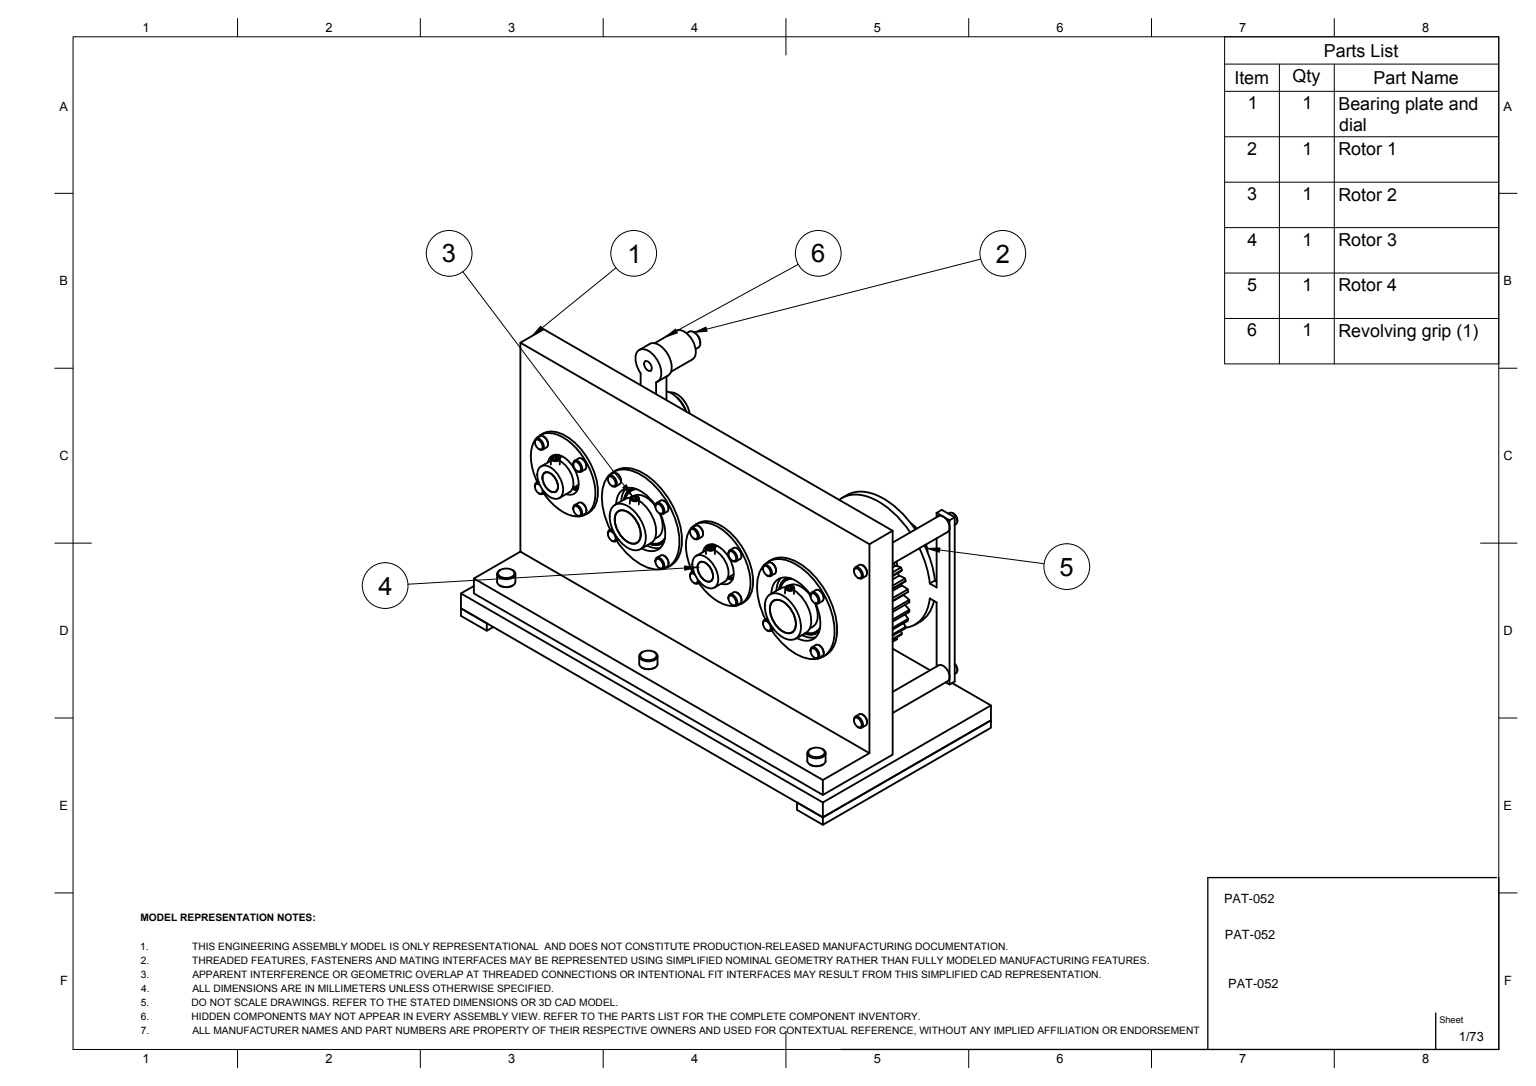
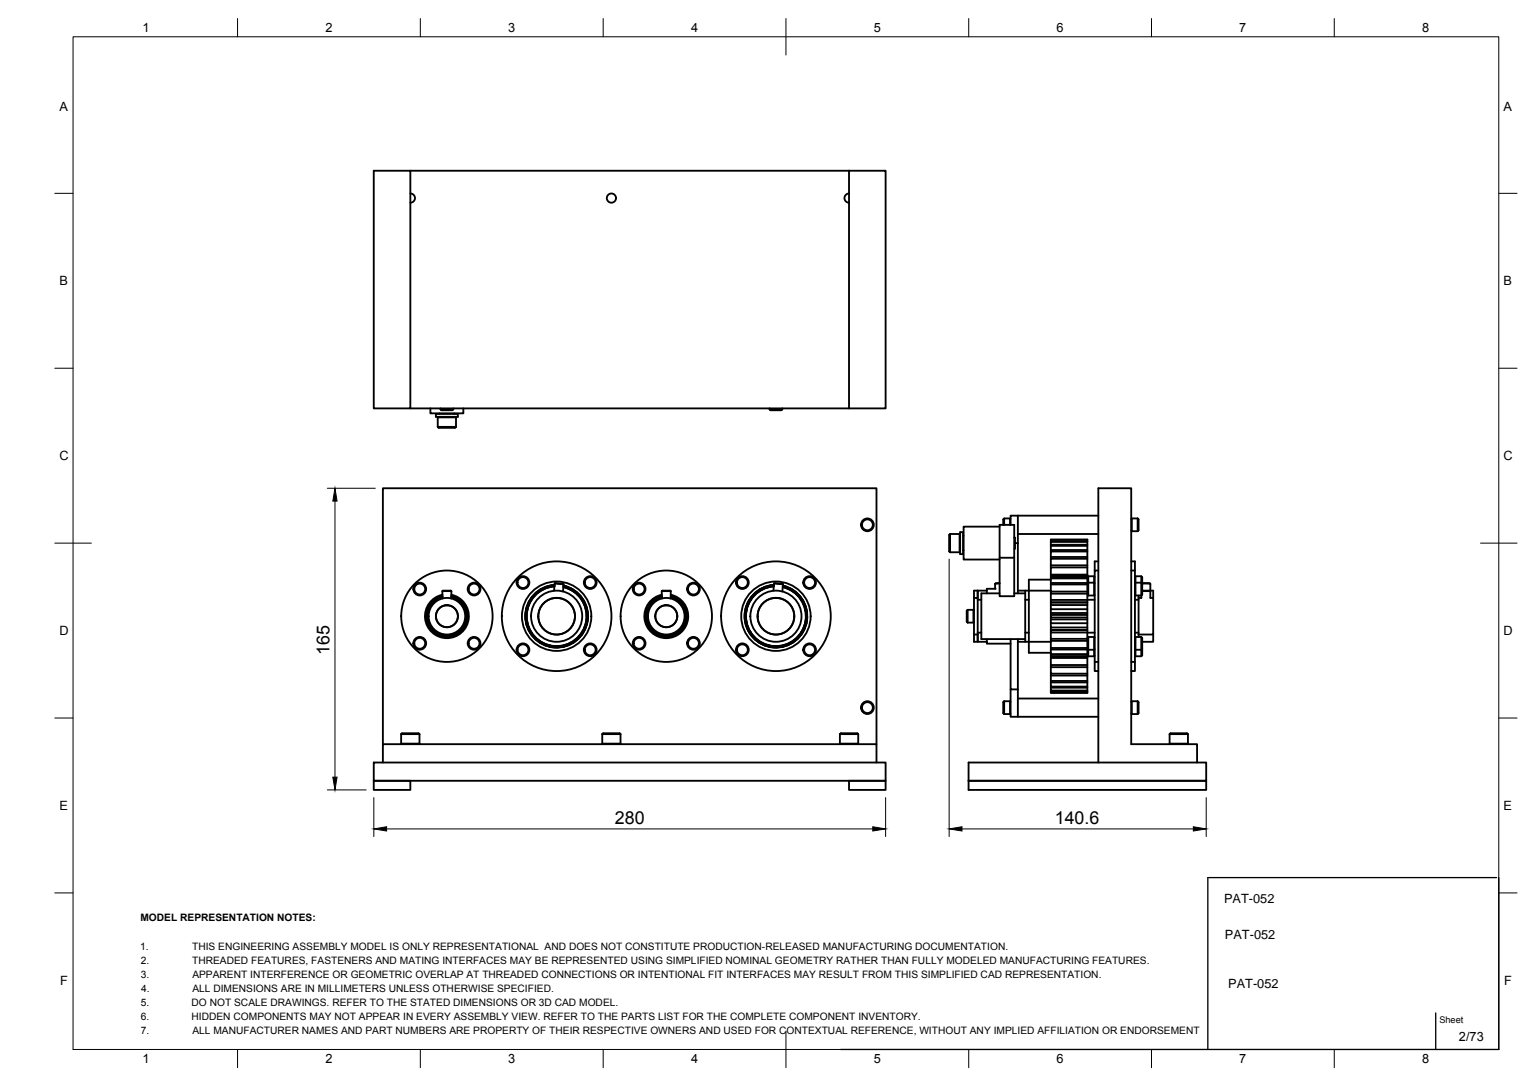
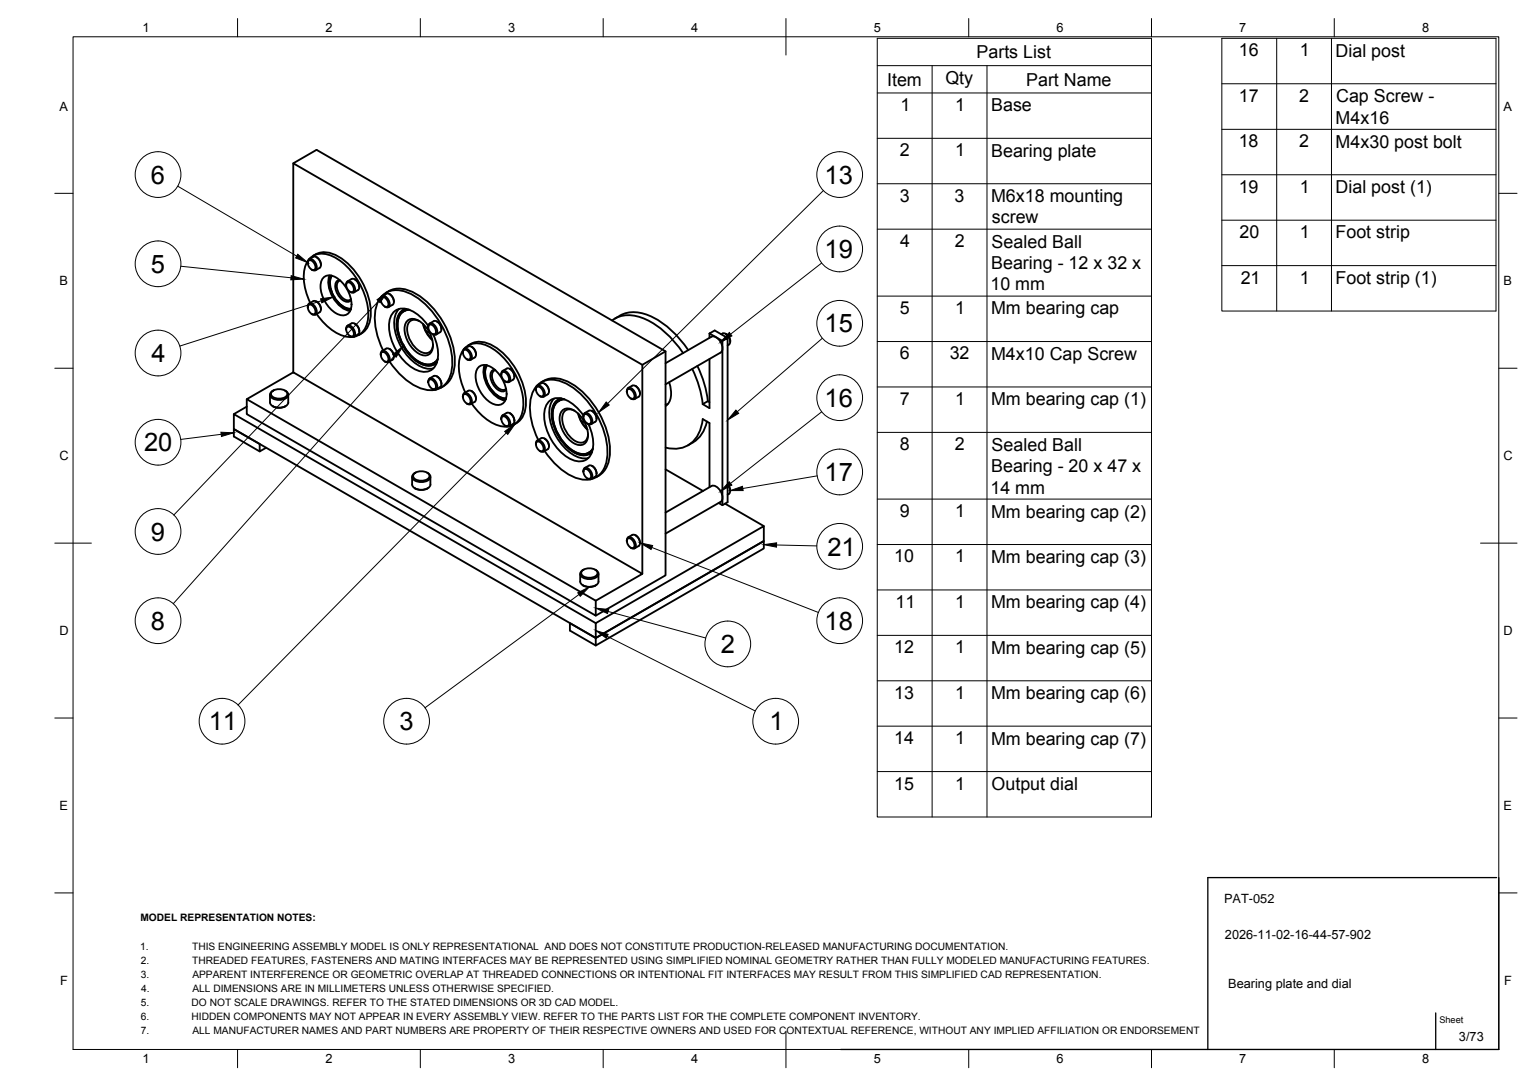
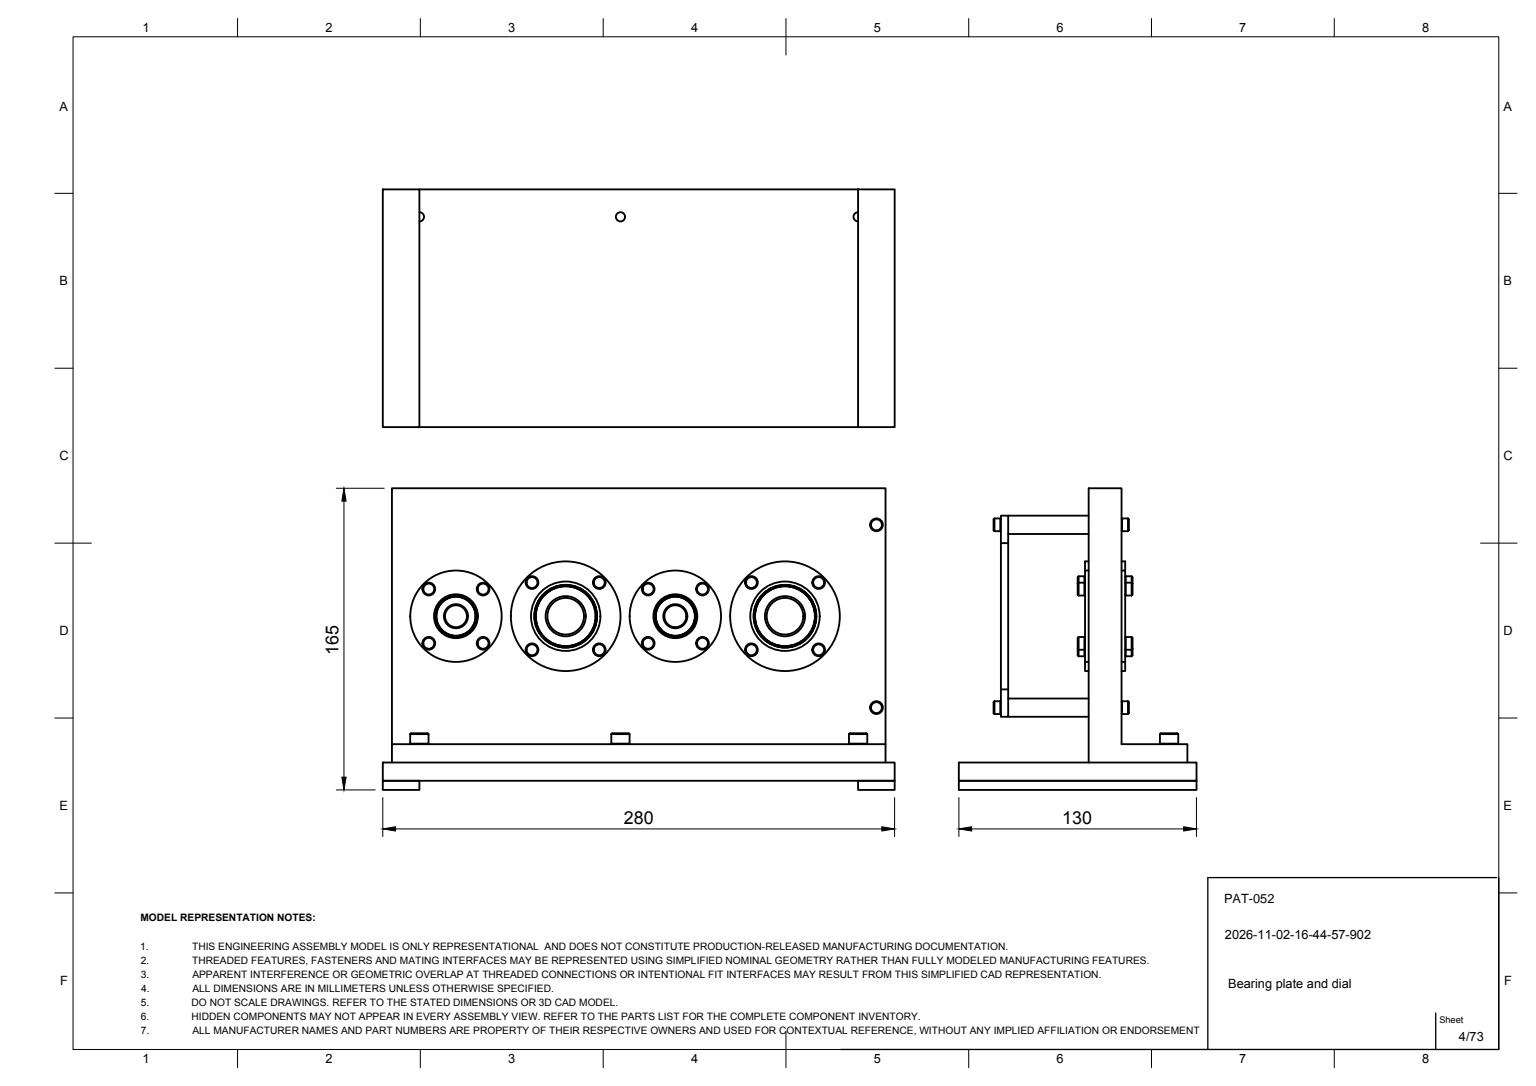
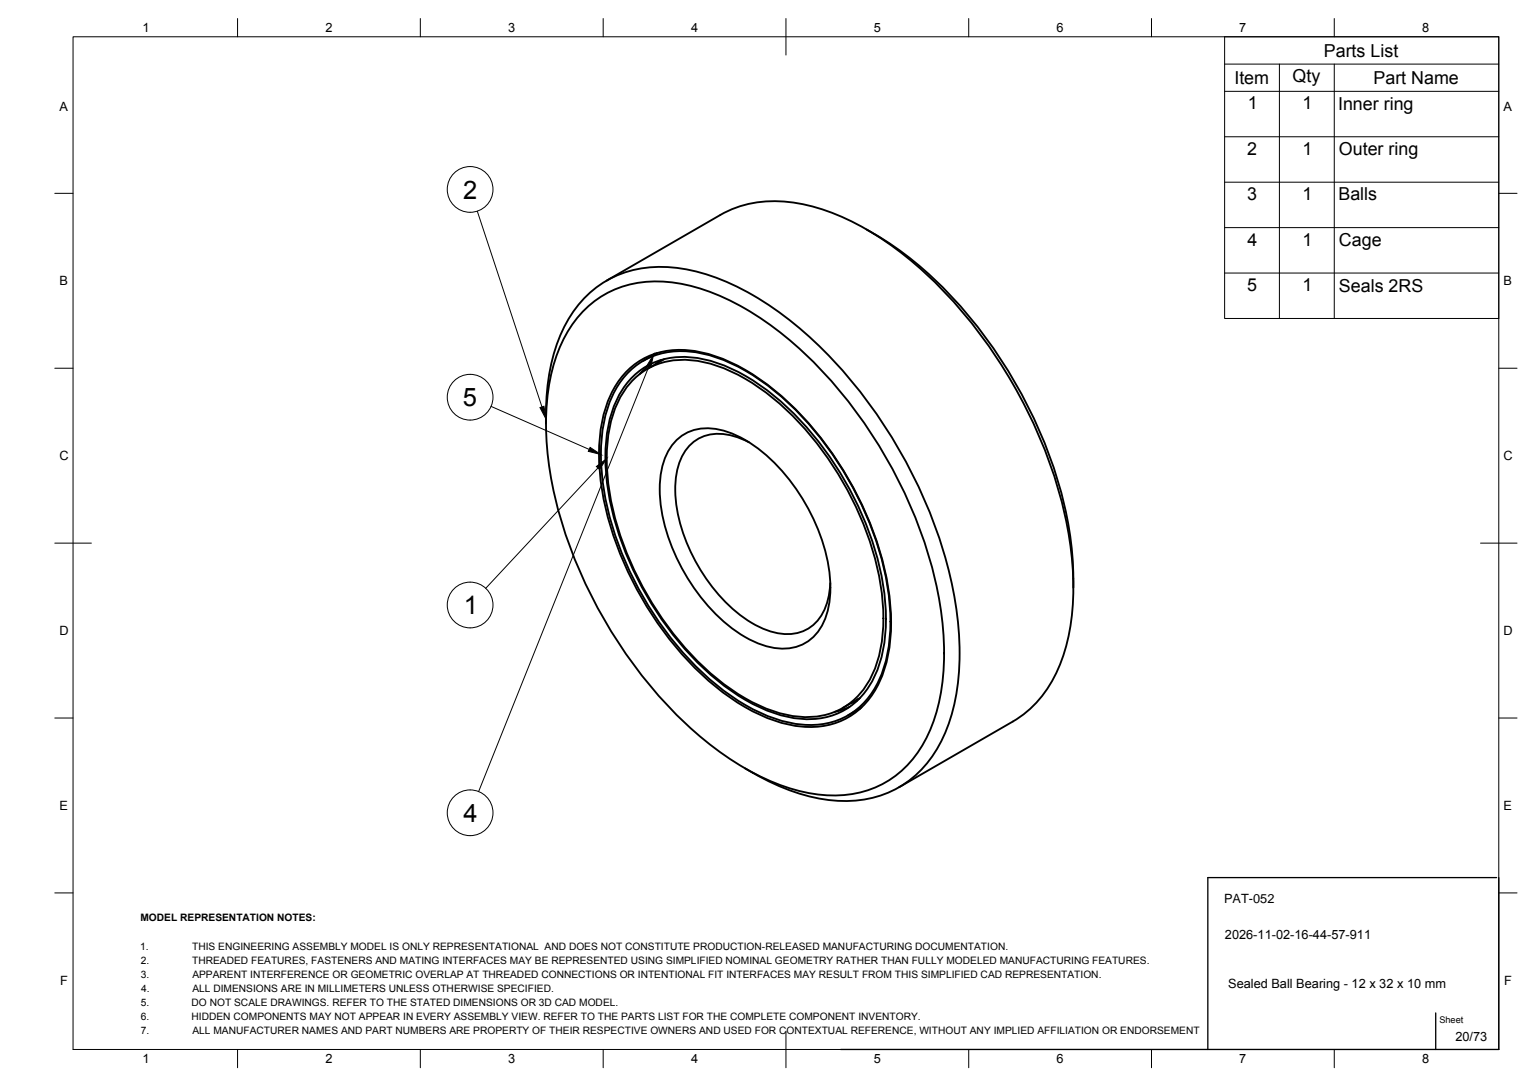
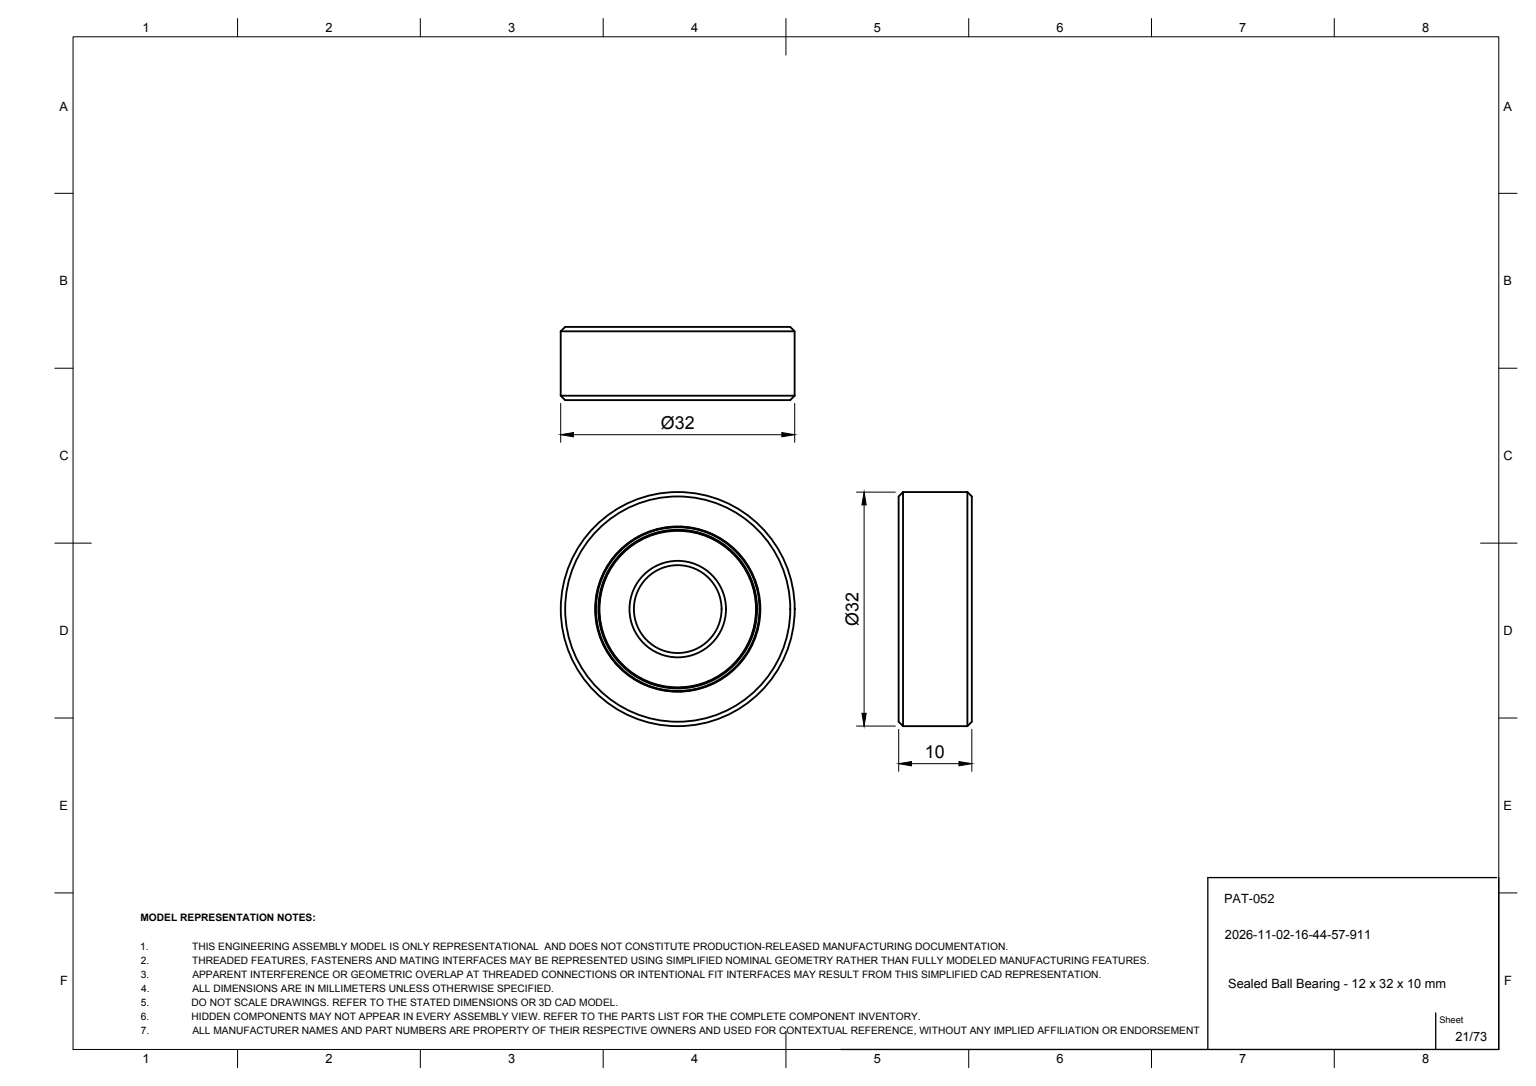
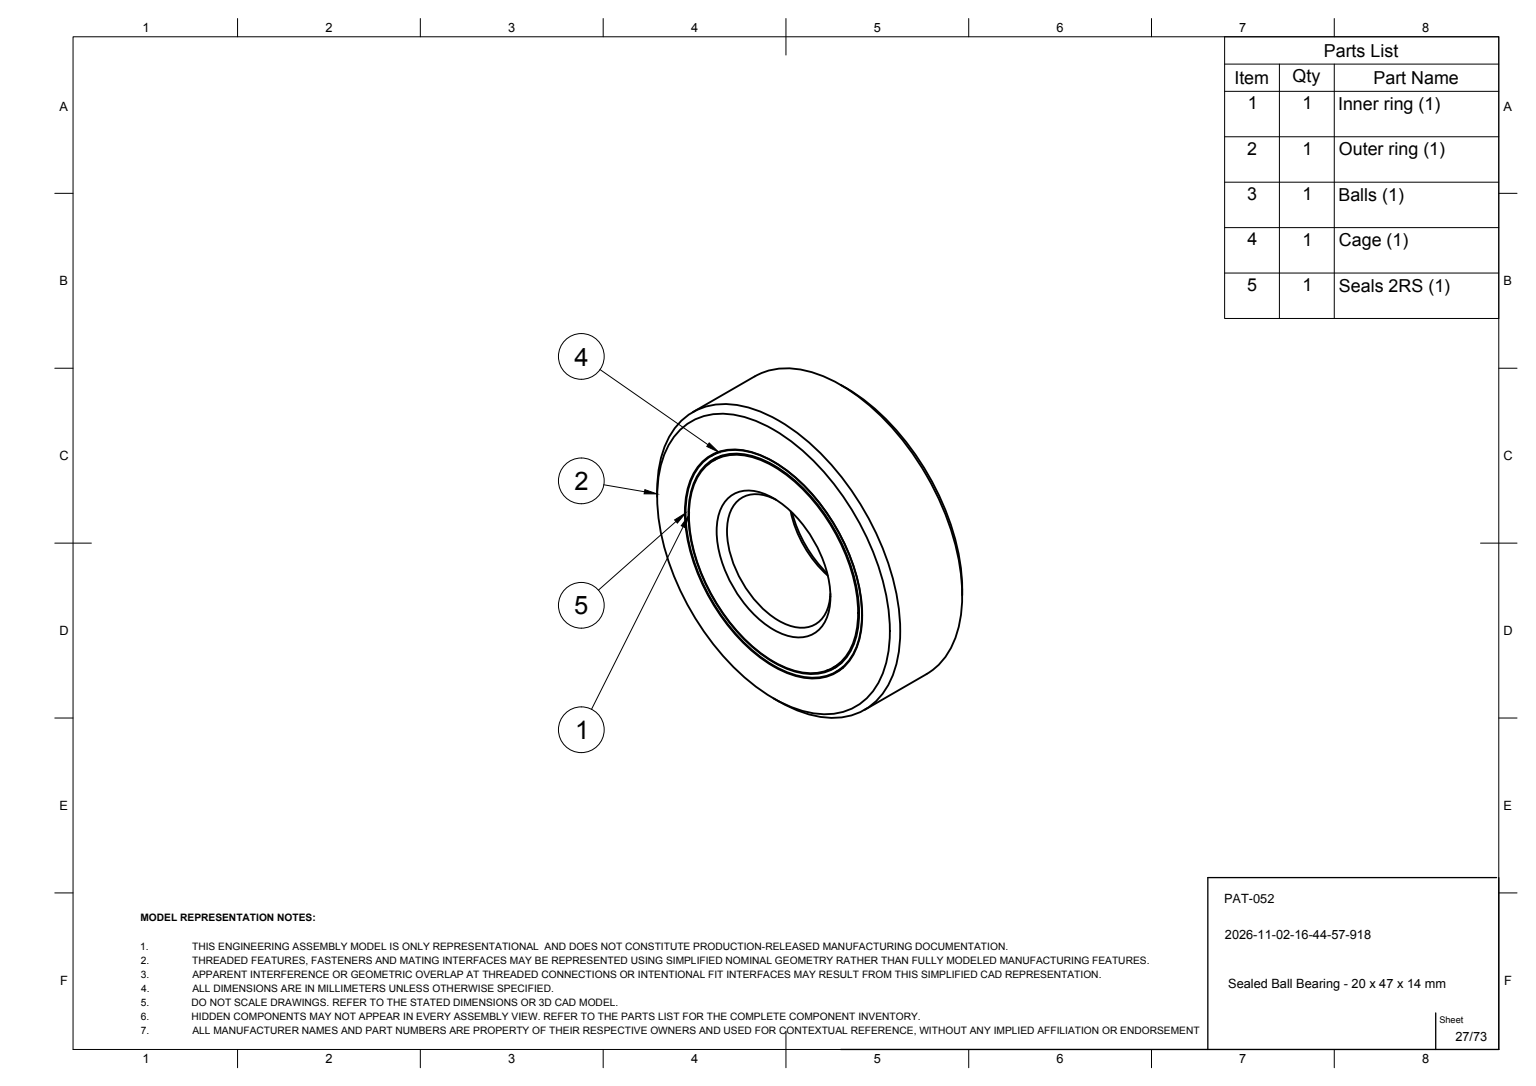
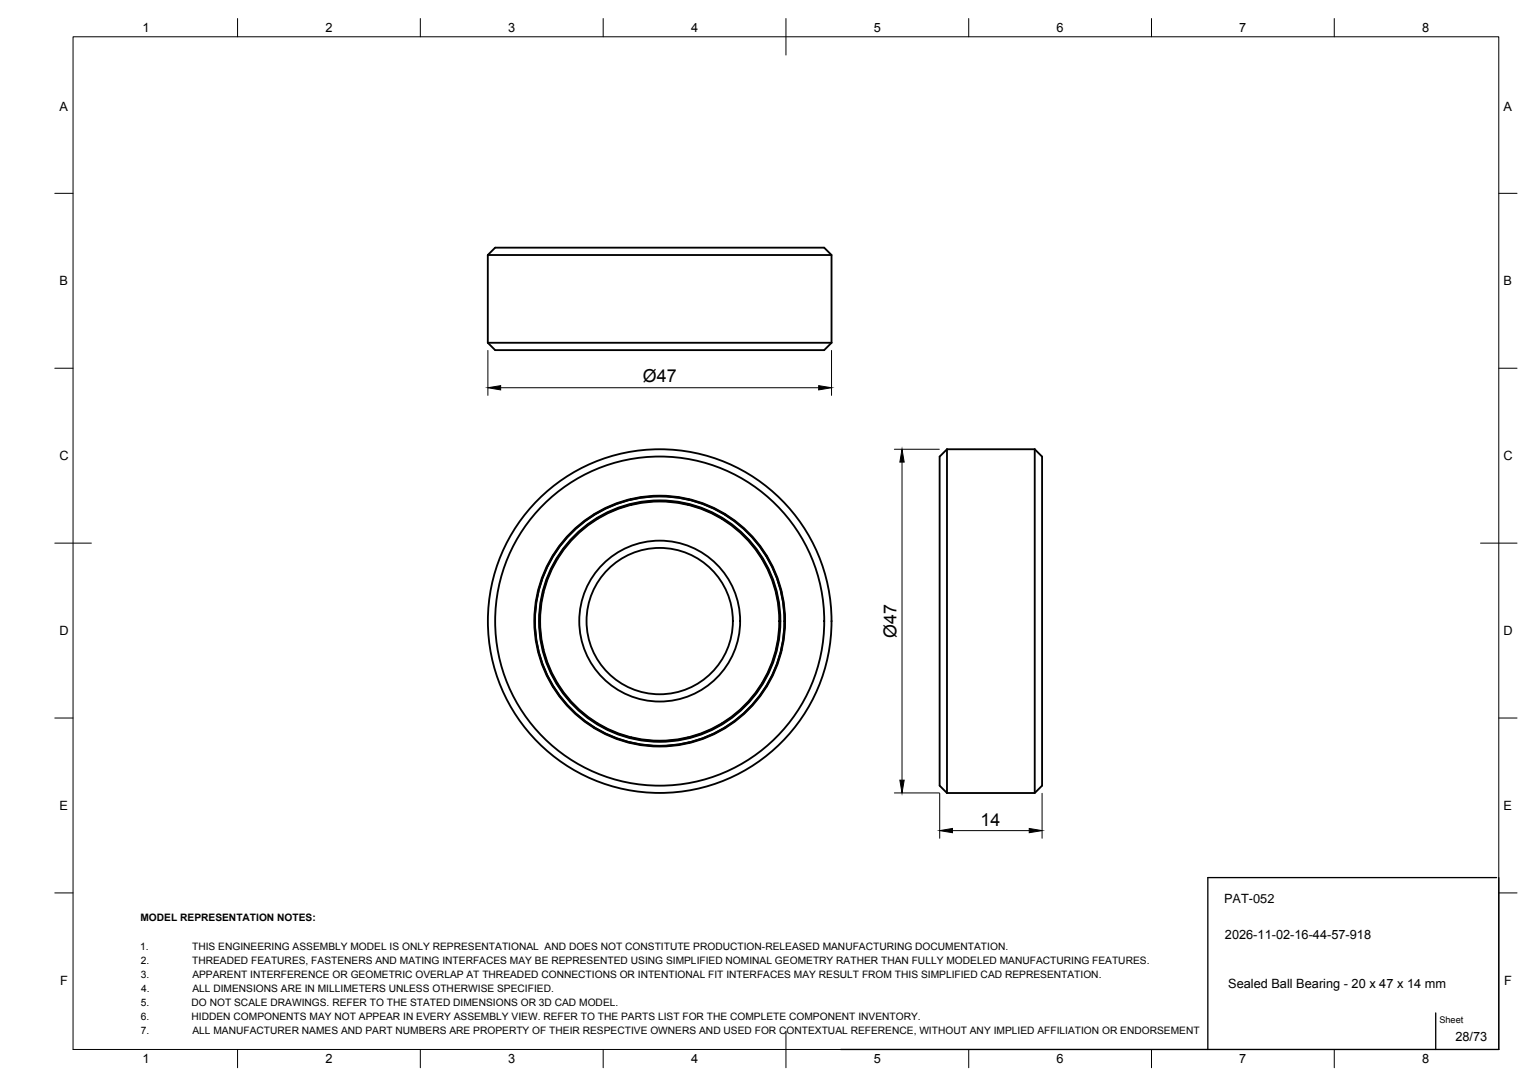
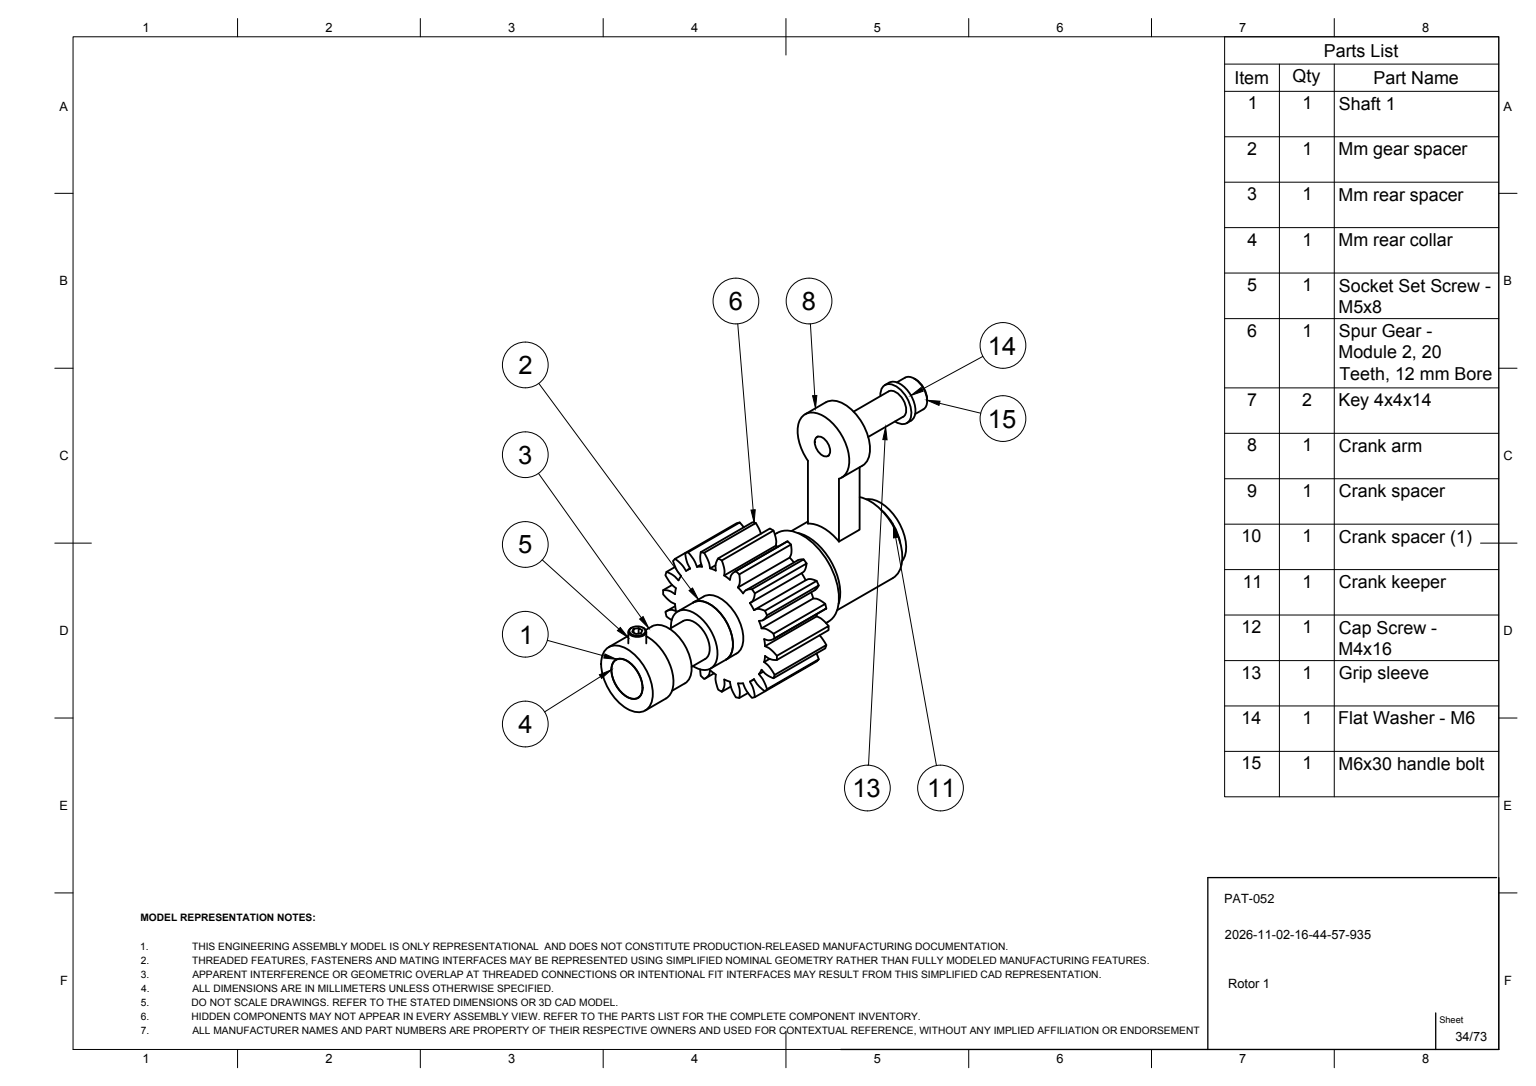
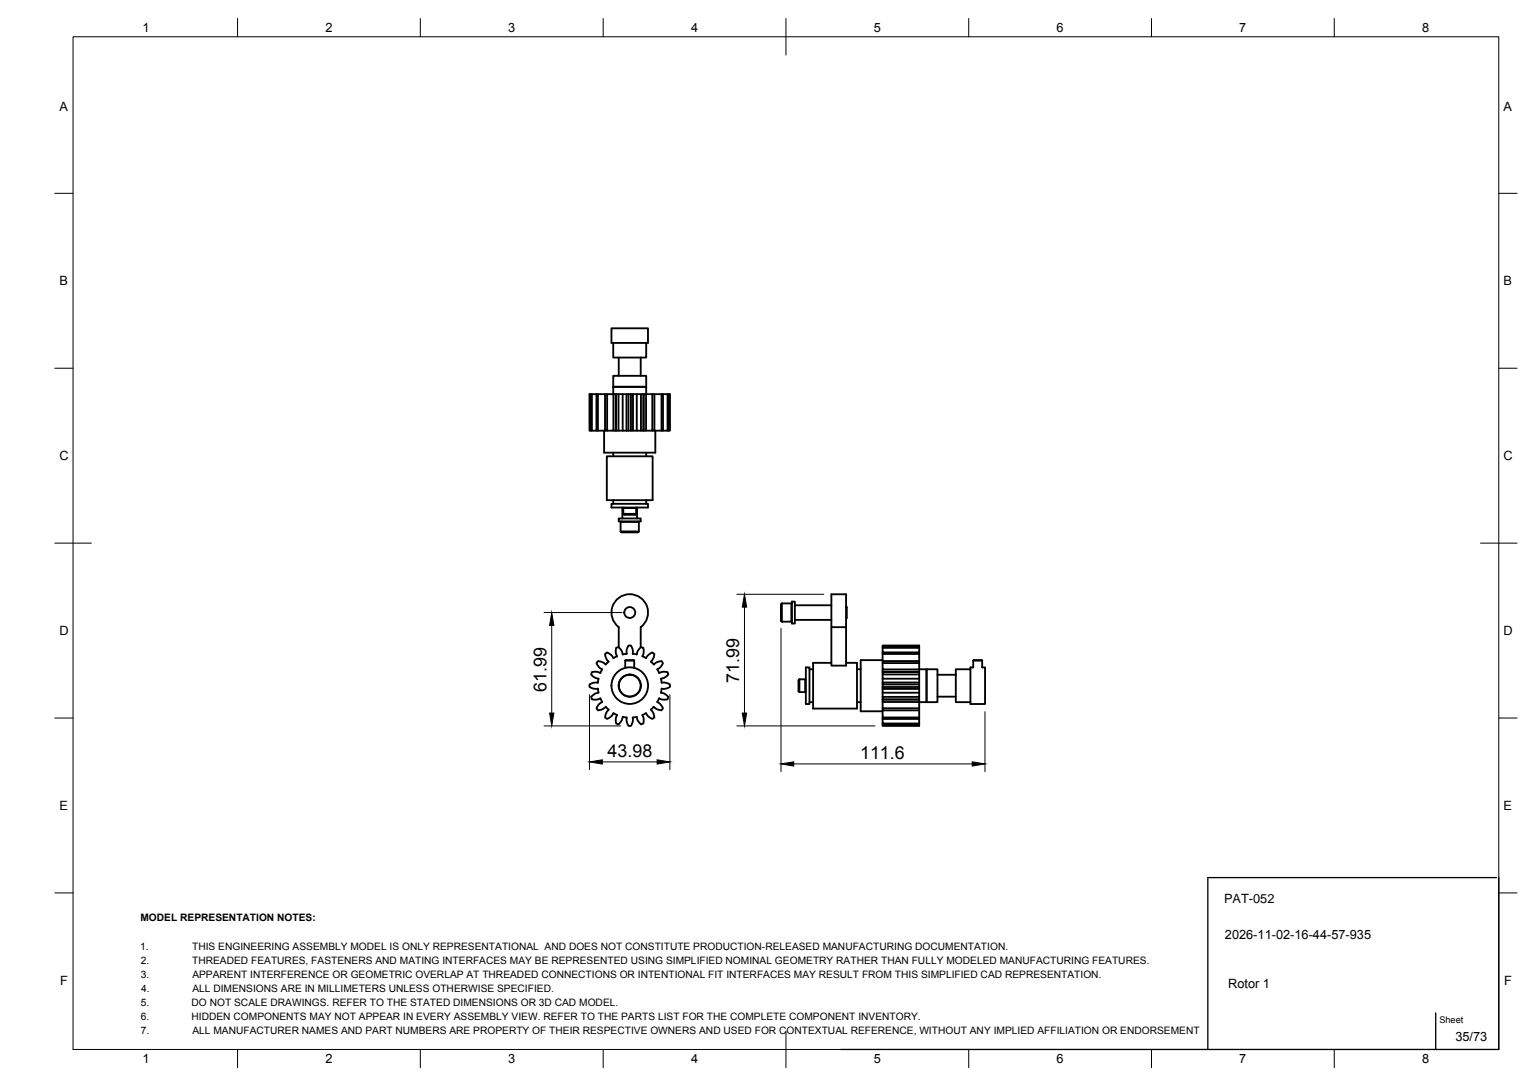
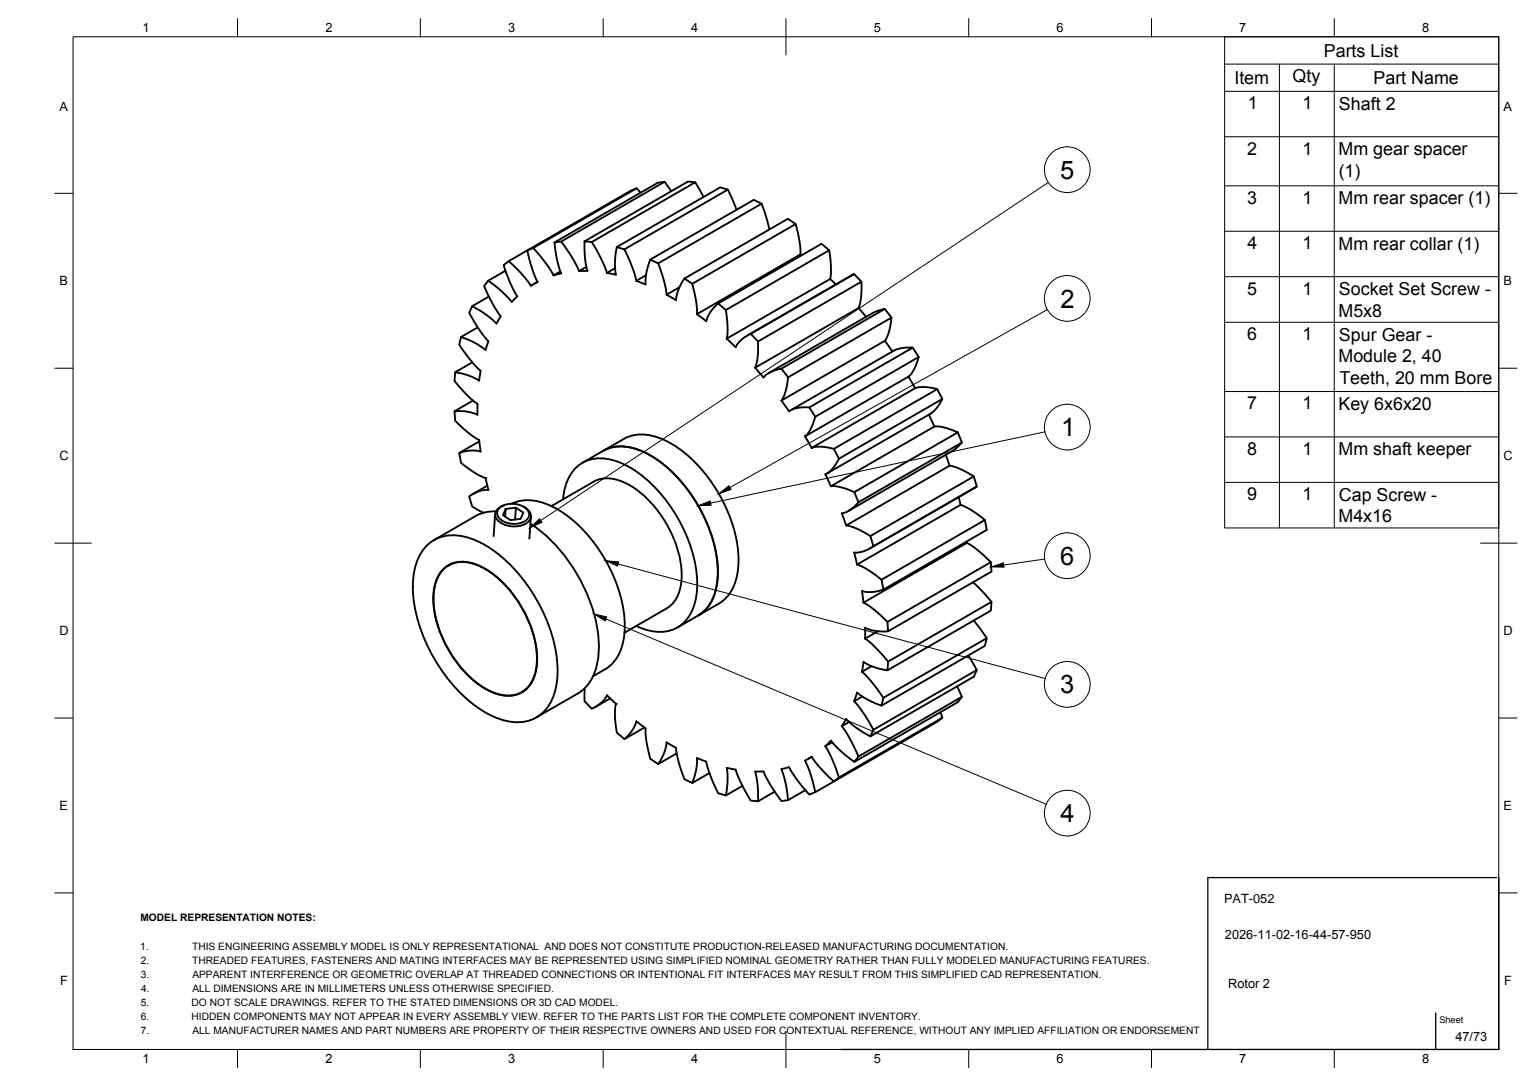
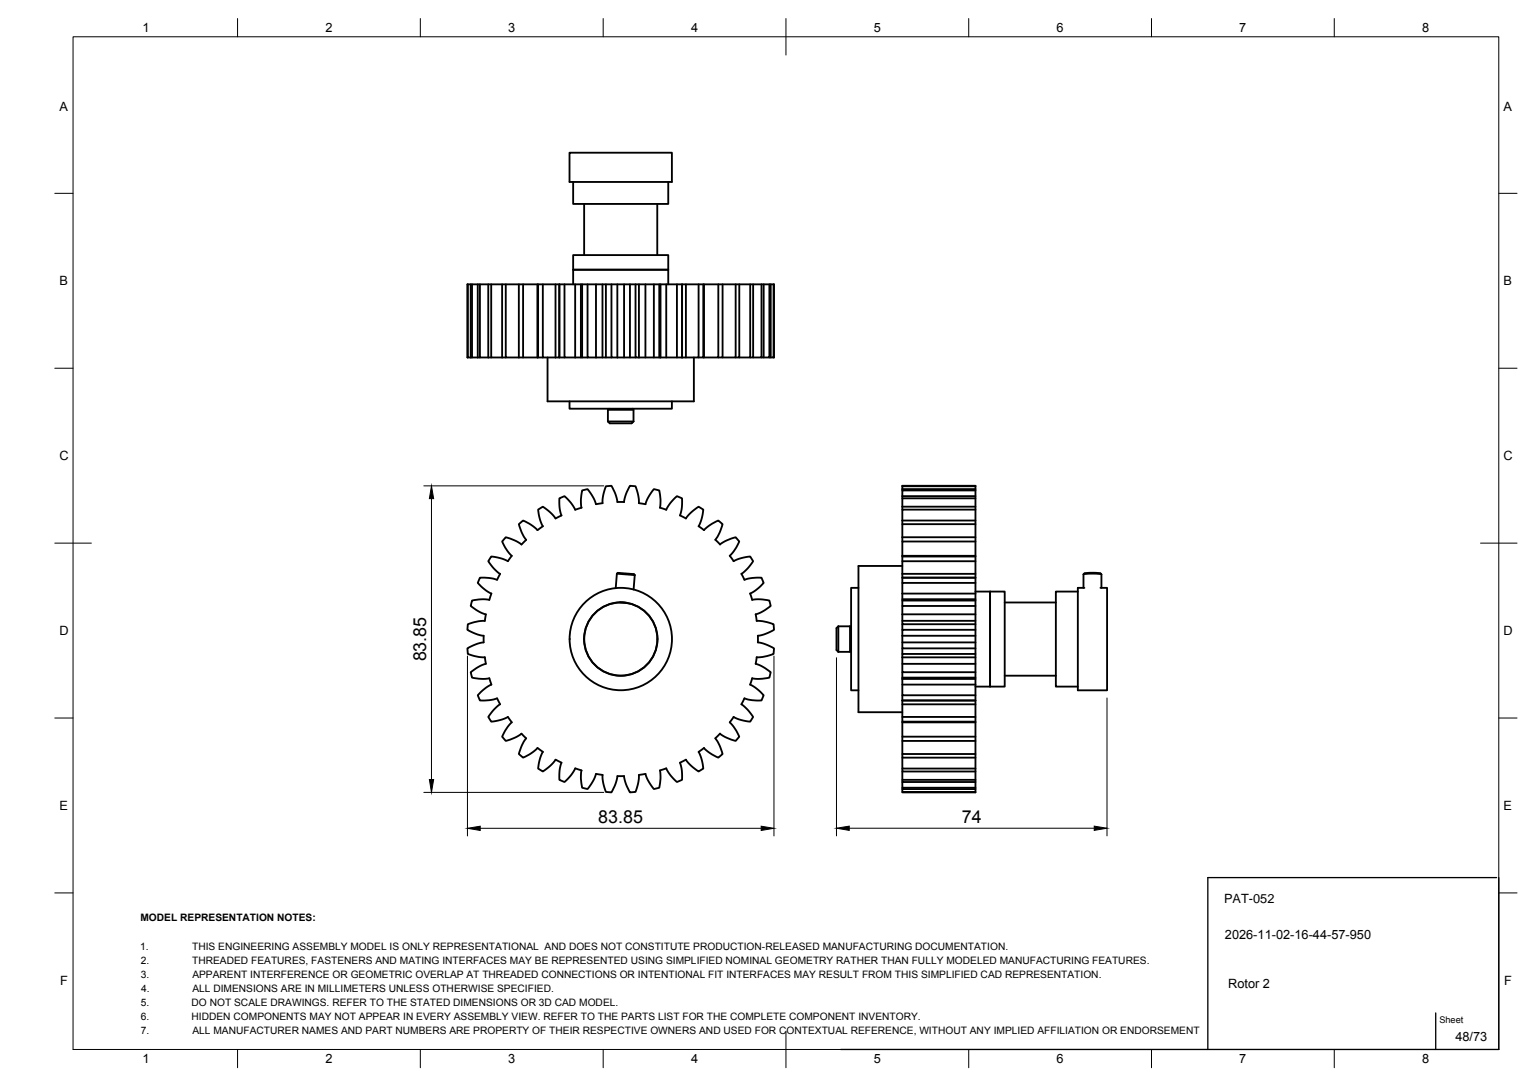
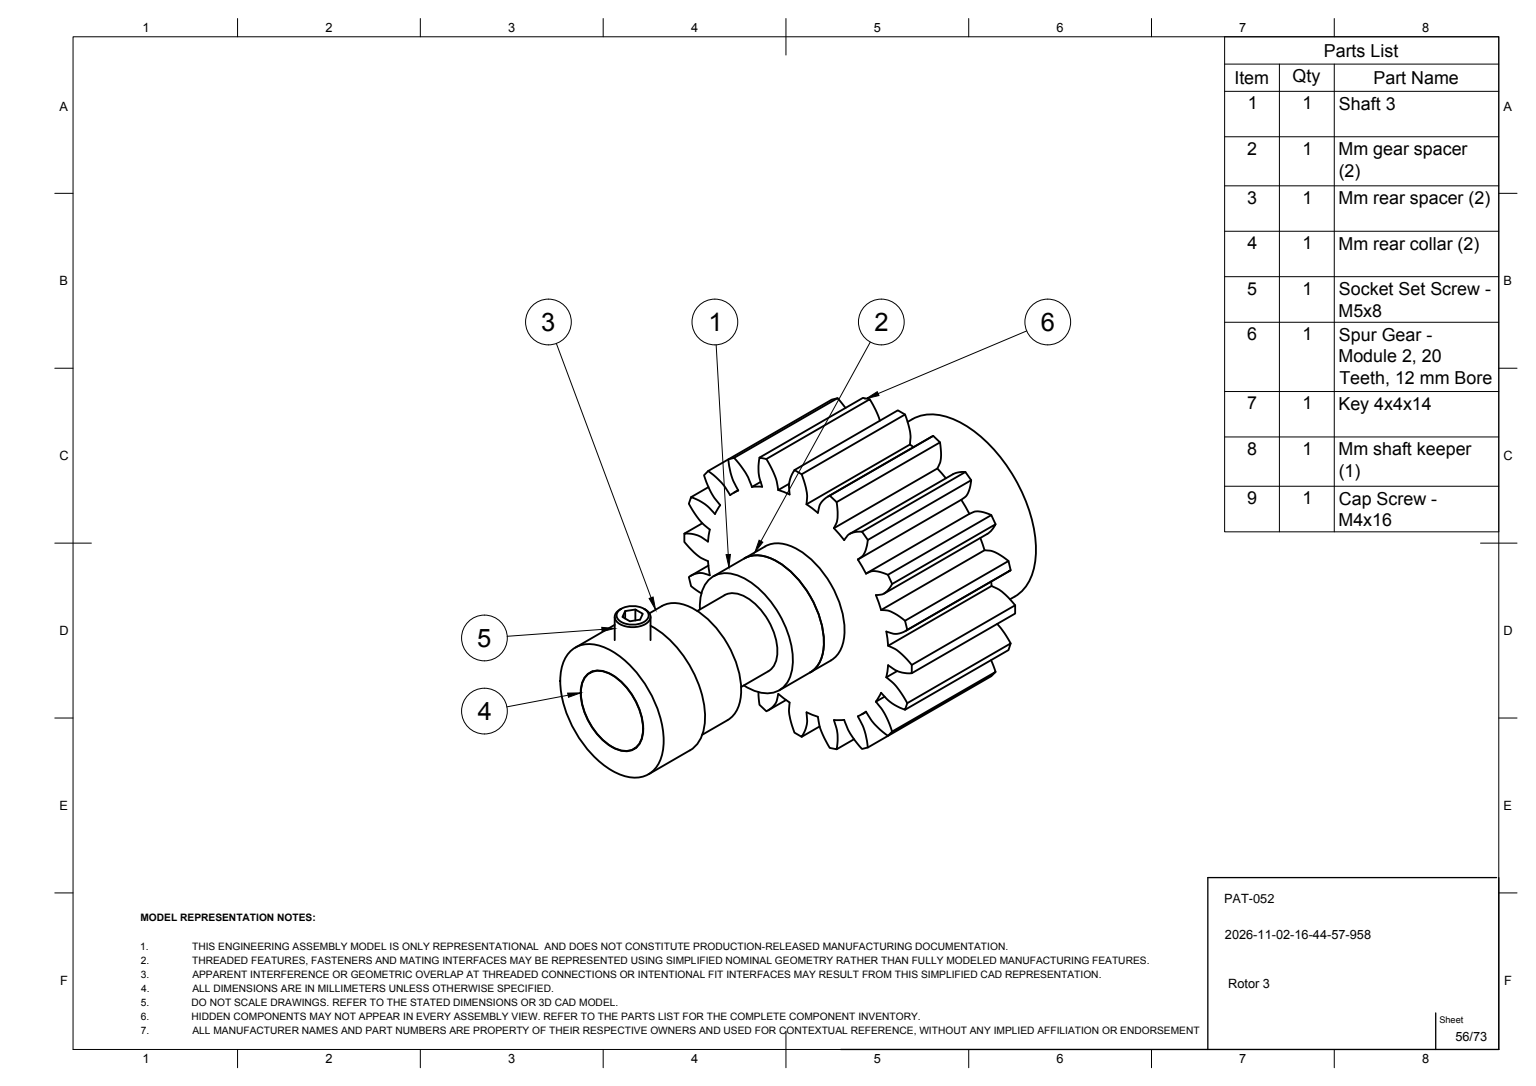
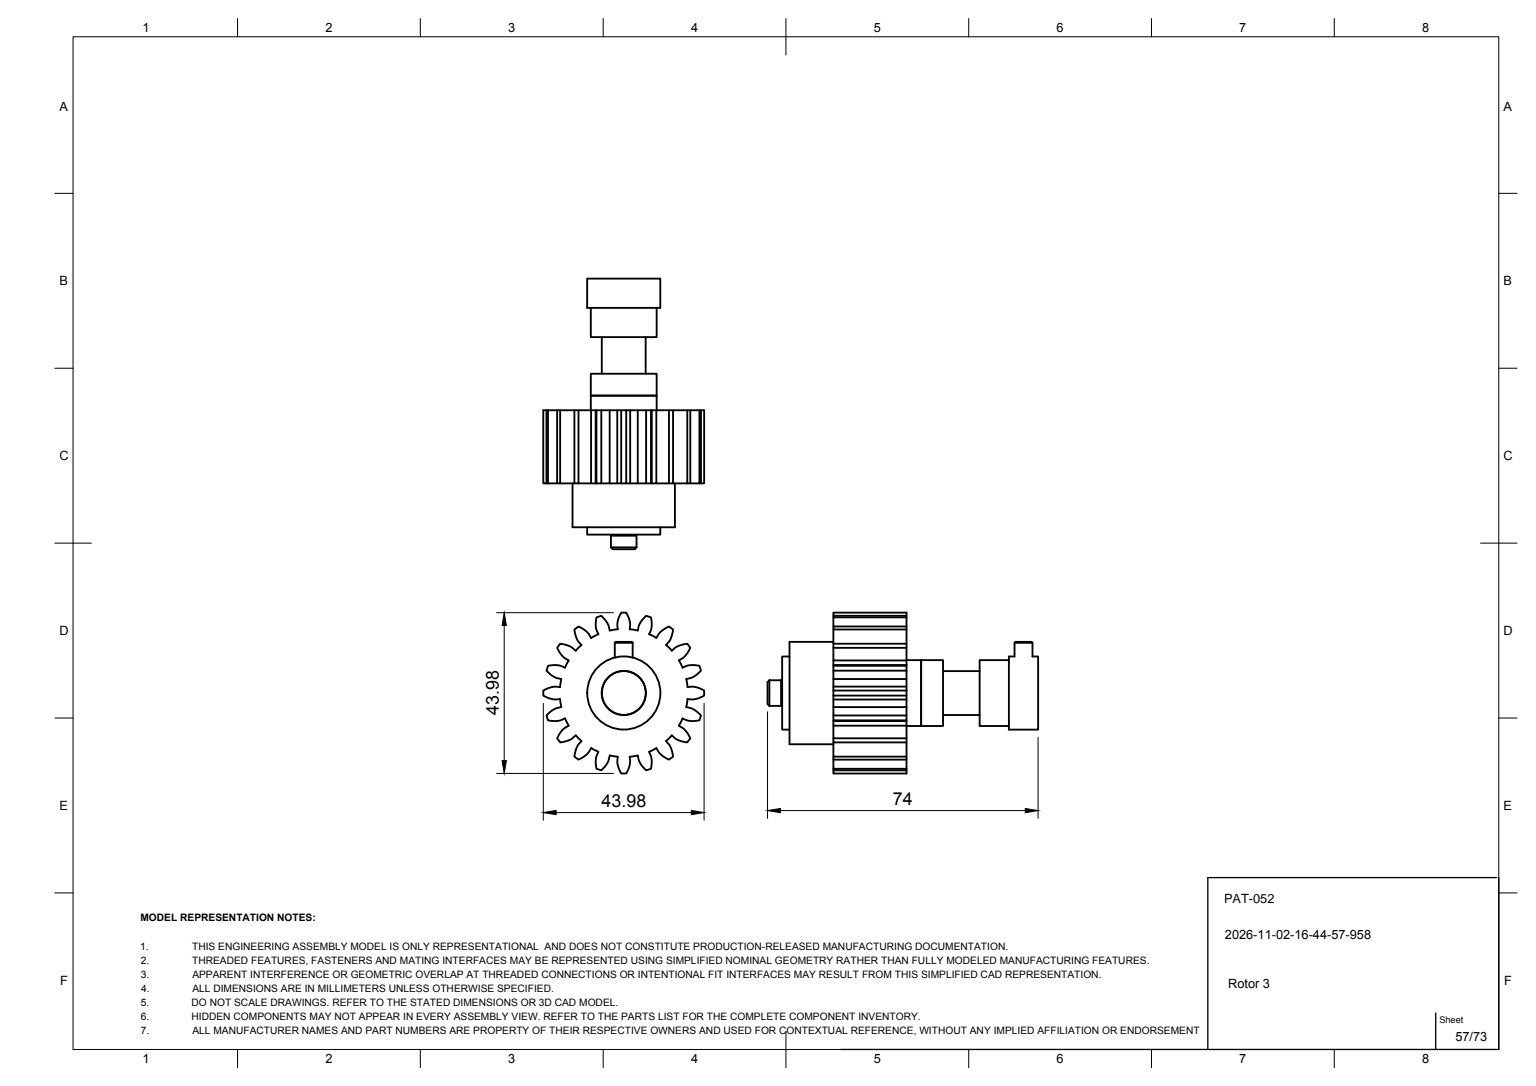
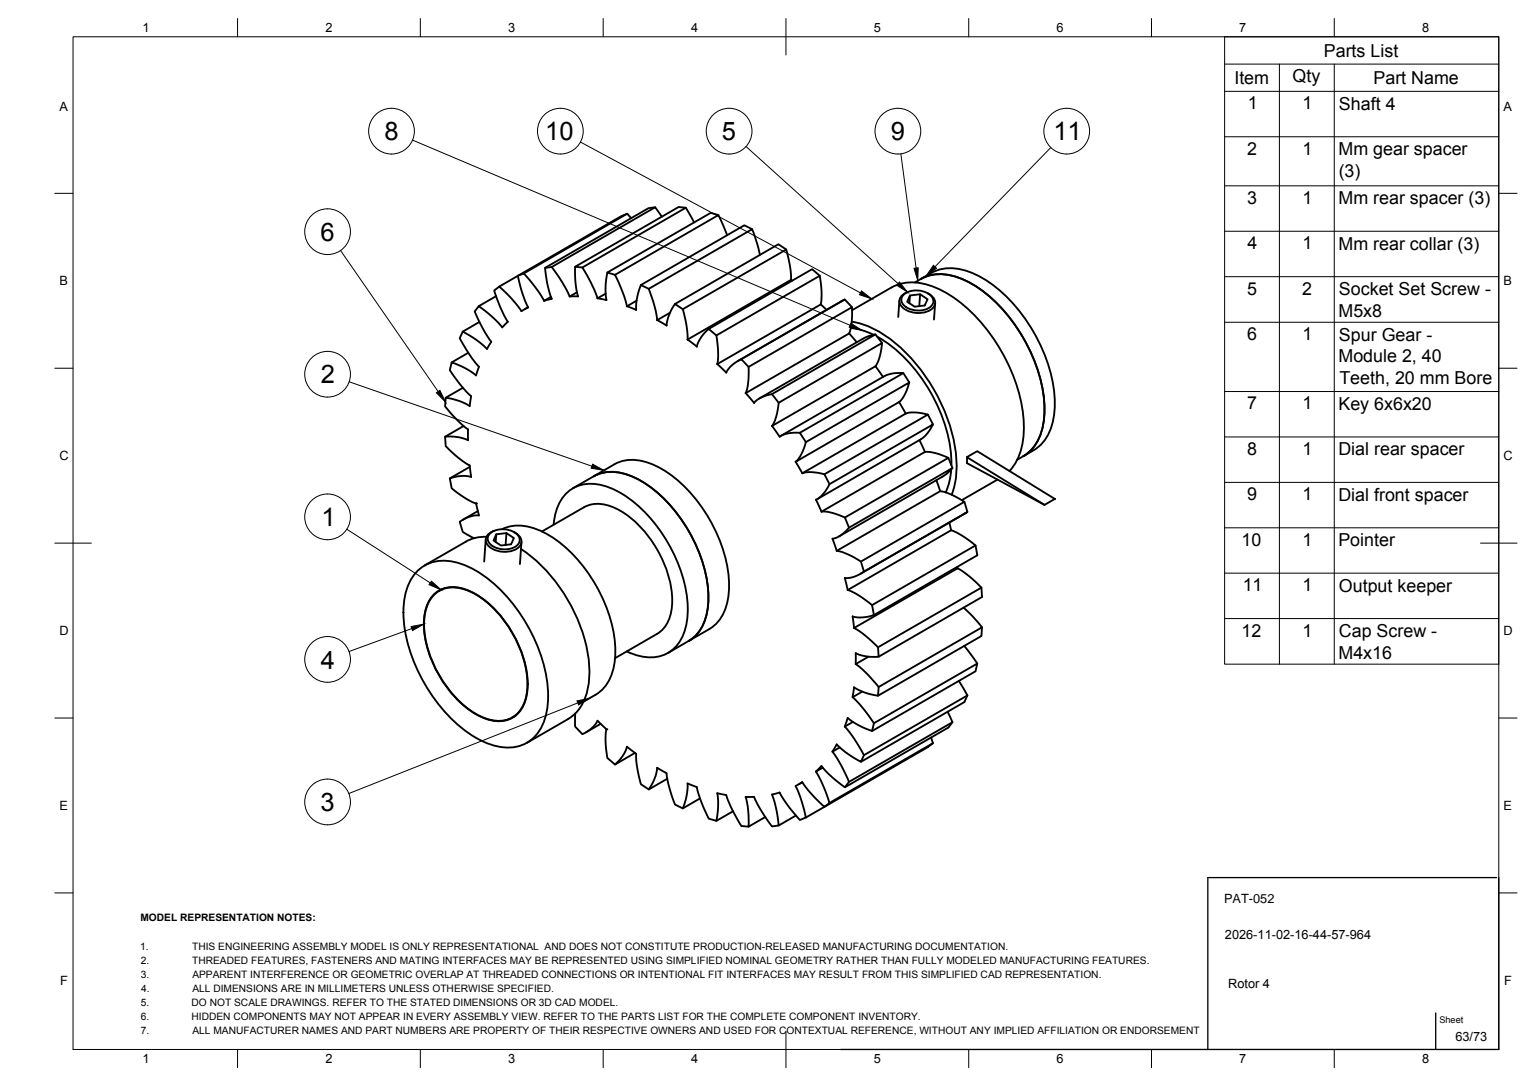
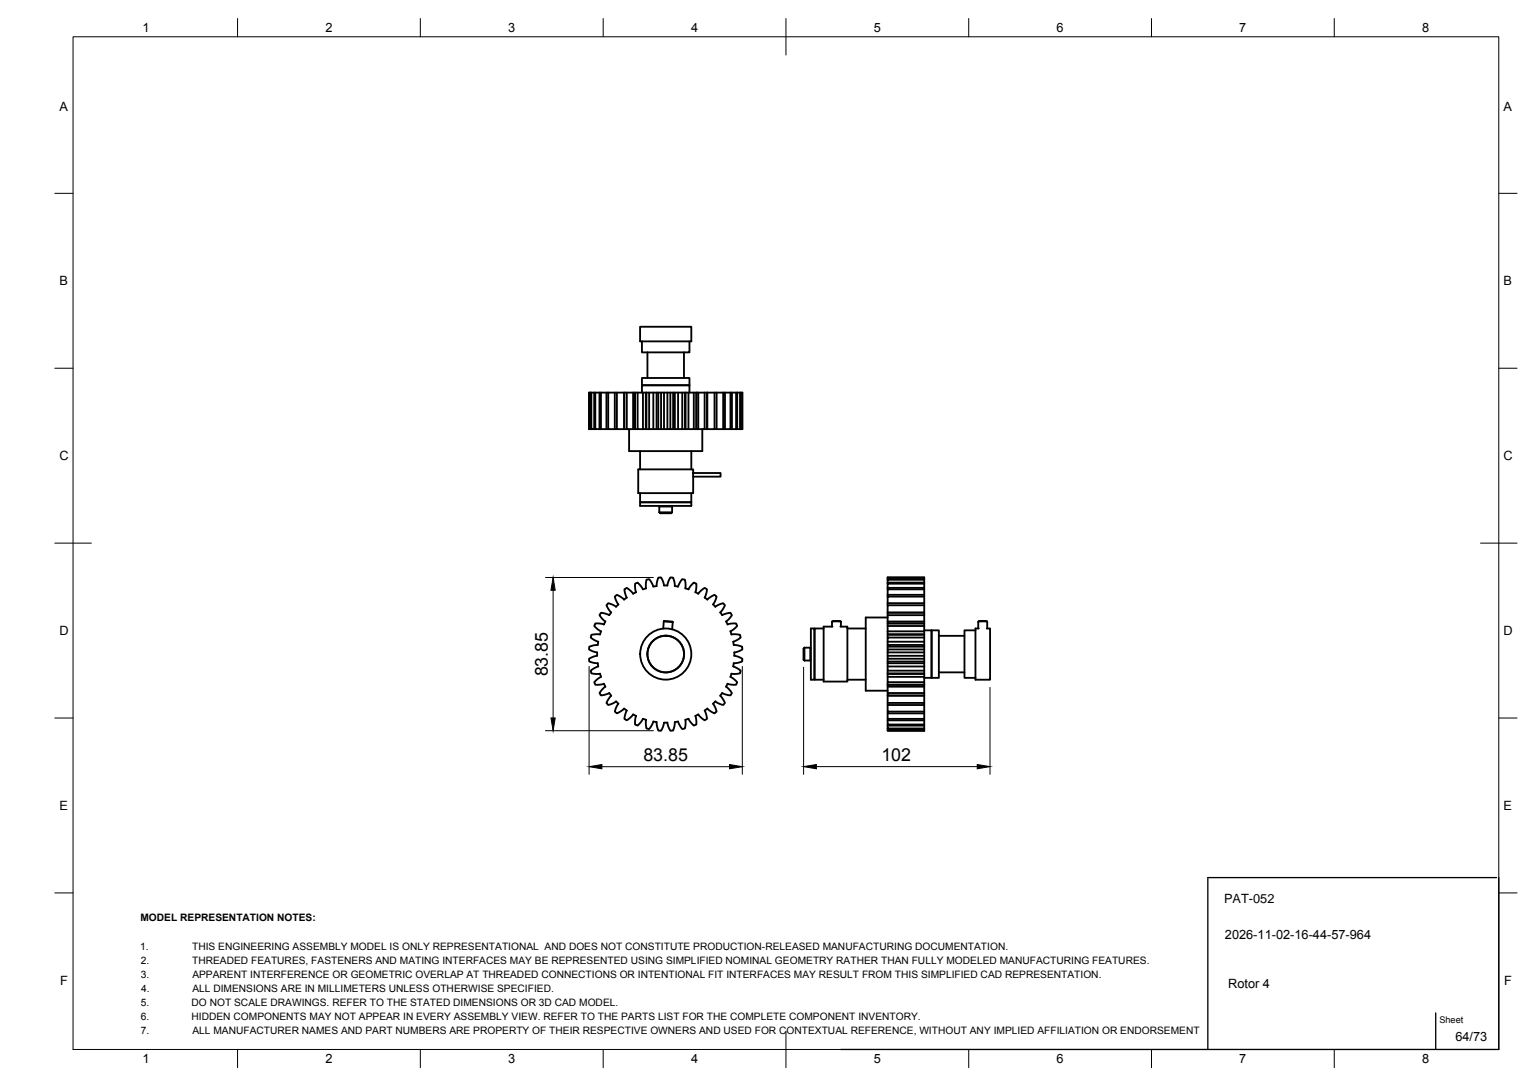
ISO-10303-21;
HEADER;
/* Generated by software containing ST-Developer
 * from STEP Tools, Inc. (www.steptools.com) 
 */

FILE_DESCRIPTION(
/* description */ ('Hand-crank gear train demonstrator'),
/* implementation_level */ '2;1');

FILE_NAME(
/* name */ 'PAT-052',
/* time_stamp */ '2026-10-28T03:22:13-07:00',
/* author */ (''),
/* organization */ (''),
/* preprocessor_version */ 'ST-DEVELOPER v20.2',
/* originating_system */ 'Autodesk Translation Framework v15.17.0.0',
/* authorisation */ '');

FILE_SCHEMA (('AUTOMOTIVE_DESIGN { 1 0 10303 214 3 1 1 }'));
ENDSEC;

DATA;
#10=MECHANICAL_DESIGN_GEOMETRIC_PRESENTATION_REPRESENTATION('',(#1189,#1190,
#1191,#1192,#1193,#1194,#1195,#1196,#1197,#1198,#1199,#1200,#1201,#1202,
#1203,#1204,#1205,#1206,#1207,#1208,#1209,#1210,#1211,#1212,#1213,#1214,
#1215,#1216,#1217,#1218,#1219,#1220,#1221,#1222,#1223,#1224,#1225,#1226,
#1227,#1228,#1229,#1230,#1231,#1232,#1233,#1234,#1235,#1236,#1237,#1238,
#1239,#1240,#1241,#1242,#1243,#1244,#1245,#1246,#1247,#1248,#1249,#1250,
#1251,#1252,#1253,#1254,#1255,#1256,#1257,#1258,#1259,#1260,#1261,#1262,
#1263,#1264,#1265,#1266,#1267),#62758);
#11=(
BOUNDED_SURFACE()
B_SPLINE_SURFACE(5,1,((#29730,#29731),(#29732,#29733),(#29734,#29735),(#29736,
#29737),(#29738,#29739),(#29740,#29741),(#29742,#29743),(#29744,#29745),
(#29746,#29747),(#29748,#29749),(#29750,#29751),(#29752,#29753),(#29754,
#29755),(#29756,#29757),(#29758,#29759),(#29760,#29761),(#29762,#29763),
(#29764,#29765),(#29766,#29767),(#29768,#29769),(#29770,#29771),(#29772,
#29773),(#29774,#29775),(#29776,#29777),(#29778,#29779),(#29780,#29781),
(#29782,#29783),(#29784,#29785),(#29786,#29787),(#29788,#29789),(#29790,
#29791),(#29792,#29793),(#29794,#29795),(#29796,#29797),(#29798,#29799),
(#29800,#29801),(#29802,#29803),(#29804,#29805),(#29806,#29807),(#29808,
#29809),(#29810,#29811),(#29812,#29813),(#29814,#29815),(#29816,#29817),
(#29818,#29819),(#29820,#29821),(#29822,#29823),(#29824,#29825),(#29826,
#29827),(#29828,#29829),(#29830,#29831),(#29832,#29833),(#29834,#29835),
(#29836,#29837),(#29838,#29839),(#29840,#29841),(#29842,#29843),(#29844,
#29845),(#29846,#29847),(#29848,#29849),(#29850,#29851),(#29852,#29853),
(#29854,#29855),(#29856,#29857),(#29858,#29859),(#29860,#29861),(#29862,
#29863),(#29864,#29865),(#29866,#29867),(#29868,#29869)),.UNSPECIFIED.,
 .F.,.F.,.F.)
B_SPLINE_SURFACE_WITH_KNOTS((6,1,1,1,1,1,1,1,1,1,1,1,1,1,1,1,1,1,1,1,1,
1,1,1,1,1,1,1,1,1,1,1,1,1,1,1,1,1,1,1,1,1,1,1,1,1,1,1,1,1,1,1,1,1,1,1,1,
1,1,1,1,1,1,1,1,6),(2,2),(-1.,-0.984615384615383,-0.969230769230768,-0.953846153846152,
-0.938461538461537,-0.923076923076922,-0.907692307692306,-0.892307692307691,
-0.876923076923076,-0.86153846153846,-0.846153846153845,-0.83076923076923,
-0.815384615384614,-0.799999999999999,-0.784615384615384,-0.769230769230768,
-0.753846153846153,-0.738461538461538,-0.723076923076922,-0.707692307692307,
-0.692307692307692,-0.676923076923076,-0.661538461538461,-0.646153846153846,
-0.63076923076923,-0.615384615384615,-0.6,-0.584615384615384,-0.569230769230769,
-0.553846153846154,-0.538461538461538,-0.523076923076923,-0.507692307692308,
-0.492307692307692,-0.476923076923077,-0.461538461538462,-0.446153846153846,
-0.430769230769231,-0.415384615384615,-0.4,-0.384615384615385,-0.369230769230769,
-0.353846153846154,-0.338461538461538,-0.323076923076923,-0.307692307692308,
-0.292307692307692,-0.276923076923077,-0.261538461538462,-0.246153846153846,
-0.230769230769231,-0.215384615384615,-0.2,-0.184615384615385,-0.169230769230769,
-0.153846153846154,-0.138461538461538,-0.123076923076923,-0.107692307692308,
-0.0923076923076923,-0.0769230769230769,-0.0615384615384615,-0.0461538461538462,
-0.0307692307692308,-0.0153846153846154,0.),(-1.,1.),.UNSPECIFIED.)
GEOMETRIC_REPRESENTATION_ITEM()
RATIONAL_B_SPLINE_SURFACE(((1.,1.),(1.,1.),(1.,1.),(1.,1.),(1.,1.),(1.,
1.),(1.,1.),(1.,1.),(1.,1.),(1.,1.),(1.,1.),(1.,1.),(1.,1.),(1.,1.),(1.,
1.),(1.,1.),(1.,1.),(1.,1.),(1.,1.),(1.,1.),(1.,1.),(1.,1.),(1.,1.),(1.,
1.),(1.,1.),(1.,1.),(1.,1.),(1.,1.),(1.,1.),(1.,1.),(1.,1.),(1.,1.),(1.,
1.),(1.,1.),(1.,1.),(1.,1.),(1.,1.),(1.,1.),(1.,1.),(1.,1.),(1.,1.),(1.,
1.),(1.,1.),(1.,1.),(1.,1.),(1.,1.),(1.,1.),(1.,1.),(1.,1.),(1.,1.),(1.,
1.),(1.,1.),(1.,1.),(1.,1.),(1.,1.),(1.,1.),(1.,1.),(1.,1.),(1.,1.),(1.,
1.),(1.,1.),(1.,1.),(1.,1.),(1.,1.),(1.,1.),(1.,1.),(1.,1.),(1.,1.),(1.,
1.),(1.,1.)))
REPRESENTATION_ITEM('')
SURFACE()
);
#12=(
BOUNDED_SURFACE()
B_SPLINE_SURFACE(5,1,((#29948,#29949),(#29950,#29951),(#29952,#29953),(#29954,
#29955),(#29956,#29957),(#29958,#29959),(#29960,#29961),(#29962,#29963),
(#29964,#29965),(#29966,#29967),(#29968,#29969),(#29970,#29971),(#29972,
#29973),(#29974,#29975),(#29976,#29977),(#29978,#29979),(#29980,#29981),
(#29982,#29983),(#29984,#29985),(#29986,#29987),(#29988,#29989),(#29990,
#29991),(#29992,#29993),(#29994,#29995),(#29996,#29997),(#29998,#29999),
(#30000,#30001),(#30002,#30003),(#30004,#30005),(#30006,#30007),(#30008,
#30009),(#30010,#30011),(#30012,#30013),(#30014,#30015),(#30016,#30017),
(#30018,#30019),(#30020,#30021),(#30022,#30023),(#30024,#30025),(#30026,
#30027),(#30028,#30029),(#30030,#30031),(#30032,#30033),(#30034,#30035),
(#30036,#30037),(#30038,#30039),(#30040,#30041),(#30042,#30043),(#30044,
#30045),(#30046,#30047),(#30048,#30049),(#30050,#30051),(#30052,#30053),
(#30054,#30055),(#30056,#30057),(#30058,#30059),(#30060,#30061),(#30062,
#30063),(#30064,#30065),(#30066,#30067),(#30068,#30069),(#30070,#30071),
(#30072,#30073),(#30074,#30075),(#30076,#30077),(#30078,#30079),(#30080,
#30081),(#30082,#30083),(#30084,#30085),(#30086,#30087)),.UNSPECIFIED.,
 .F.,.F.,.F.)
B_SPLINE_SURFACE_WITH_KNOTS((6,1,1,1,1,1,1,1,1,1,1,1,1,1,1,1,1,1,1,1,1,
1,1,1,1,1,1,1,1,1,1,1,1,1,1,1,1,1,1,1,1,1,1,1,1,1,1,1,1,1,1,1,1,1,1,1,1,
1,1,1,1,1,1,1,1,6),(2,2),(-1.,-0.984615384615383,-0.969230769230768,-0.953846153846152,
-0.938461538461537,-0.923076923076922,-0.907692307692306,-0.892307692307691,
-0.876923076923076,-0.86153846153846,-0.846153846153845,-0.83076923076923,
-0.815384615384614,-0.799999999999999,-0.784615384615384,-0.769230769230768,
-0.753846153846153,-0.738461538461538,-0.723076923076922,-0.707692307692307,
-0.692307692307692,-0.676923076923076,-0.661538461538461,-0.646153846153846,
-0.63076923076923,-0.615384615384615,-0.6,-0.584615384615384,-0.569230769230769,
-0.553846153846154,-0.538461538461538,-0.523076923076923,-0.507692307692308,
-0.492307692307692,-0.476923076923077,-0.461538461538462,-0.446153846153846,
-0.430769230769231,-0.415384615384615,-0.4,-0.384615384615385,-0.369230769230769,
-0.353846153846154,-0.338461538461538,-0.323076923076923,-0.307692307692308,
-0.292307692307692,-0.276923076923077,-0.261538461538462,-0.246153846153846,
-0.230769230769231,-0.215384615384615,-0.2,-0.184615384615385,-0.169230769230769,
-0.153846153846154,-0.138461538461538,-0.123076923076923,-0.107692307692308,
-0.0923076923076923,-0.0769230769230769,-0.0615384615384615,-0.0461538461538462,
-0.0307692307692308,-0.0153846153846154,0.),(-1.,1.),.UNSPECIFIED.)
GEOMETRIC_REPRESENTATION_ITEM()
RATIONAL_B_SPLINE_SURFACE(((1.,1.),(1.,1.),(1.,1.),(1.,1.),(1.,1.),(1.,
1.),(1.,1.),(1.,1.),(1.,1.),(1.,1.),(1.,1.),(1.,1.),(1.,1.),(1.,1.),(1.,
1.),(1.,1.),(1.,1.),(1.,1.),(1.,1.),(1.,1.),(1.,1.),(1.,1.),(1.,1.),(1.,
1.),(1.,1.),(1.,1.),(1.,1.),(1.,1.),(1.,1.),(1.,1.),(1.,1.),(1.,1.),(1.,
1.),(1.,1.),(1.,1.),(1.,1.),(1.,1.),(1.,1.),(1.,1.),(1.,1.),(1.,1.),(1.,
1.),(1.,1.),(1.,1.),(1.,1.),(1.,1.),(1.,1.),(1.,1.),(1.,1.),(1.,1.),(1.,
1.),(1.,1.),(1.,1.),(1.,1.),(1.,1.),(1.,1.),(1.,1.),(1.,1.),(1.,1.),(1.,
1.),(1.,1.),(1.,1.),(1.,1.),(1.,1.),(1.,1.),(1.,1.),(1.,1.),(1.,1.),(1.,
1.),(1.,1.)))
REPRESENTATION_ITEM('')
SURFACE()
);
#13=(
BOUNDED_SURFACE()
B_SPLINE_SURFACE(5,1,((#30164,#30165),(#30166,#30167),(#30168,#30169),(#30170,
#30171),(#30172,#30173),(#30174,#30175),(#30176,#30177),(#30178,#30179),
(#30180,#30181),(#30182,#30183),(#30184,#30185),(#30186,#30187),(#30188,
#30189),(#30190,#30191),(#30192,#30193),(#30194,#30195),(#30196,#30197),
(#30198,#30199),(#30200,#30201),(#30202,#30203),(#30204,#30205),(#30206,
#30207),(#30208,#30209),(#30210,#30211),(#30212,#30213),(#30214,#30215),
(#30216,#30217),(#30218,#30219),(#30220,#30221),(#30222,#30223),(#30224,
#30225),(#30226,#30227),(#30228,#30229),(#30230,#30231),(#30232,#30233),
(#30234,#30235),(#30236,#30237),(#30238,#30239),(#30240,#30241),(#30242,
#30243),(#30244,#30245),(#30246,#30247),(#30248,#30249),(#30250,#30251),
(#30252,#30253),(#30254,#30255),(#30256,#30257),(#30258,#30259),(#30260,
#30261),(#30262,#30263),(#30264,#30265),(#30266,#30267),(#30268,#30269),
(#30270,#30271),(#30272,#30273),(#30274,#30275),(#30276,#30277),(#30278,
#30279),(#30280,#30281),(#30282,#30283),(#30284,#30285),(#30286,#30287),
(#30288,#30289),(#30290,#30291),(#30292,#30293),(#30294,#30295),(#30296,
#30297),(#30298,#30299),(#30300,#30301),(#30302,#30303)),.UNSPECIFIED.,
 .F.,.F.,.F.)
B_SPLINE_SURFACE_WITH_KNOTS((6,1,1,1,1,1,1,1,1,1,1,1,1,1,1,1,1,1,1,1,1,
1,1,1,1,1,1,1,1,1,1,1,1,1,1,1,1,1,1,1,1,1,1,1,1,1,1,1,1,1,1,1,1,1,1,1,1,
1,1,1,1,1,1,1,1,6),(2,2),(-1.,-0.984615384615383,-0.969230769230768,-0.953846153846152,
-0.938461538461537,-0.923076923076922,-0.907692307692306,-0.892307692307691,
-0.876923076923076,-0.86153846153846,-0.846153846153845,-0.83076923076923,
-0.815384615384614,-0.799999999999999,-0.784615384615384,-0.769230769230768,
-0.753846153846153,-0.738461538461538,-0.723076923076922,-0.707692307692307,
-0.692307692307692,-0.676923076923076,-0.661538461538461,-0.646153846153846,
-0.63076923076923,-0.615384615384615,-0.6,-0.584615384615384,-0.569230769230769,
-0.553846153846154,-0.538461538461538,-0.523076923076923,-0.507692307692308,
-0.492307692307692,-0.476923076923077,-0.461538461538462,-0.446153846153846,
-0.430769230769231,-0.415384615384615,-0.4,-0.384615384615385,-0.369230769230769,
-0.353846153846154,-0.338461538461538,-0.323076923076923,-0.307692307692308,
-0.292307692307692,-0.276923076923077,-0.261538461538462,-0.246153846153846,
-0.230769230769231,-0.215384615384615,-0.2,-0.184615384615385,-0.169230769230769,
-0.153846153846154,-0.138461538461538,-0.123076923076923,-0.107692307692308,
-0.0923076923076923,-0.0769230769230769,-0.0615384615384615,-0.0461538461538462,
-0.0307692307692308,-0.0153846153846154,0.),(-1.,1.),.UNSPECIFIED.)
GEOMETRIC_REPRESENTATION_ITEM()
RATIONAL_B_SPLINE_SURFACE(((1.,1.),(1.,1.),(1.,1.),(1.,1.),(1.,1.),(1.,
1.),(1.,1.),(1.,1.),(1.,1.),(1.,1.),(1.,1.),(1.,1.),(1.,1.),(1.,1.),(1.,
1.),(1.,1.),(1.,1.),(1.,1.),(1.,1.),(1.,1.),(1.,1.),(1.,1.),(1.,1.),(1.,
1.),(1.,1.),(1.,1.),(1.,1.),(1.,1.),(1.,1.),(1.,1.),(1.,1.),(1.,1.),(1.,
1.),(1.,1.),(1.,1.),(1.,1.),(1.,1.),(1.,1.),(1.,1.),(1.,1.),(1.,1.),(1.,
1.),(1.,1.),(1.,1.),(1.,1.),(1.,1.),(1.,1.),(1.,1.),(1.,1.),(1.,1.),(1.,
1.),(1.,1.),(1.,1.),(1.,1.),(1.,1.),(1.,1.),(1.,1.),(1.,1.),(1.,1.),(1.,
1.),(1.,1.),(1.,1.),(1.,1.),(1.,1.),(1.,1.),(1.,1.),(1.,1.),(1.,1.),(1.,
1.),(1.,1.)))
REPRESENTATION_ITEM('')
SURFACE()
);
#14=(
BOUNDED_SURFACE()
B_SPLINE_SURFACE(5,1,((#30380,#30381),(#30382,#30383),(#30384,#30385),(#30386,
#30387),(#30388,#30389),(#30390,#30391),(#30392,#30393),(#30394,#30395),
(#30396,#30397),(#30398,#30399),(#30400,#30401),(#30402,#30403),(#30404,
#30405),(#30406,#30407),(#30408,#30409),(#30410,#30411),(#30412,#30413),
(#30414,#30415),(#30416,#30417),(#30418,#30419),(#30420,#30421),(#30422,
#30423),(#30424,#30425),(#30426,#30427),(#30428,#30429),(#30430,#30431),
(#30432,#30433),(#30434,#30435),(#30436,#30437),(#30438,#30439),(#30440,
#30441),(#30442,#30443),(#30444,#30445),(#30446,#30447),(#30448,#30449),
(#30450,#30451),(#30452,#30453),(#30454,#30455),(#30456,#30457),(#30458,
#30459),(#30460,#30461),(#30462,#30463),(#30464,#30465),(#30466,#30467),
(#30468,#30469),(#30470,#30471),(#30472,#30473),(#30474,#30475),(#30476,
#30477),(#30478,#30479),(#30480,#30481),(#30482,#30483),(#30484,#30485),
(#30486,#30487),(#30488,#30489),(#30490,#30491),(#30492,#30493),(#30494,
#30495),(#30496,#30497),(#30498,#30499),(#30500,#30501),(#30502,#30503),
(#30504,#30505),(#30506,#30507),(#30508,#30509),(#30510,#30511),(#30512,
#30513),(#30514,#30515),(#30516,#30517),(#30518,#30519)),.UNSPECIFIED.,
 .F.,.F.,.F.)
B_SPLINE_SURFACE_WITH_KNOTS((6,1,1,1,1,1,1,1,1,1,1,1,1,1,1,1,1,1,1,1,1,
1,1,1,1,1,1,1,1,1,1,1,1,1,1,1,1,1,1,1,1,1,1,1,1,1,1,1,1,1,1,1,1,1,1,1,1,
1,1,1,1,1,1,1,1,6),(2,2),(-1.,-0.984615384615383,-0.969230769230768,-0.953846153846152,
-0.938461538461537,-0.923076923076922,-0.907692307692306,-0.892307692307691,
-0.876923076923076,-0.86153846153846,-0.846153846153845,-0.83076923076923,
-0.815384615384614,-0.799999999999999,-0.784615384615384,-0.769230769230768,
-0.753846153846153,-0.738461538461538,-0.723076923076922,-0.707692307692307,
-0.692307692307692,-0.676923076923076,-0.661538461538461,-0.646153846153846,
-0.63076923076923,-0.615384615384615,-0.6,-0.584615384615384,-0.569230769230769,
-0.553846153846154,-0.538461538461538,-0.523076923076923,-0.507692307692308,
-0.492307692307692,-0.476923076923077,-0.461538461538462,-0.446153846153846,
-0.430769230769231,-0.415384615384615,-0.4,-0.384615384615385,-0.369230769230769,
-0.353846153846154,-0.338461538461538,-0.323076923076923,-0.307692307692308,
-0.292307692307692,-0.276923076923077,-0.261538461538462,-0.246153846153846,
-0.230769230769231,-0.215384615384615,-0.2,-0.184615384615385,-0.169230769230769,
-0.153846153846154,-0.138461538461538,-0.123076923076923,-0.107692307692308,
-0.0923076923076923,-0.0769230769230769,-0.0615384615384615,-0.0461538461538462,
-0.0307692307692308,-0.0153846153846154,0.),(-1.,1.),.UNSPECIFIED.)
GEOMETRIC_REPRESENTATION_ITEM()
RATIONAL_B_SPLINE_SURFACE(((1.,1.),(1.,1.),(1.,1.),(1.,1.),(1.,1.),(1.,
1.),(1.,1.),(1.,1.),(1.,1.),(1.,1.),(1.,1.),(1.,1.),(1.,1.),(1.,1.),(1.,
1.),(1.,1.),(1.,1.),(1.,1.),(1.,1.),(1.,1.),(1.,1.),(1.,1.),(1.,1.),(1.,
1.),(1.,1.),(1.,1.),(1.,1.),(1.,1.),(1.,1.),(1.,1.),(1.,1.),(1.,1.),(1.,
1.),(1.,1.),(1.,1.),(1.,1.),(1.,1.),(1.,1.),(1.,1.),(1.,1.),(1.,1.),(1.,
1.),(1.,1.),(1.,1.),(1.,1.),(1.,1.),(1.,1.),(1.,1.),(1.,1.),(1.,1.),(1.,
1.),(1.,1.),(1.,1.),(1.,1.),(1.,1.),(1.,1.),(1.,1.),(1.,1.),(1.,1.),(1.,
1.),(1.,1.),(1.,1.),(1.,1.),(1.,1.),(1.,1.),(1.,1.),(1.,1.),(1.,1.),(1.,
1.),(1.,1.)))
REPRESENTATION_ITEM('')
SURFACE()
);
#15=(
BOUNDED_SURFACE()
B_SPLINE_SURFACE(5,1,((#30596,#30597),(#30598,#30599),(#30600,#30601),(#30602,
#30603),(#30604,#30605),(#30606,#30607),(#30608,#30609),(#30610,#30611),
(#30612,#30613),(#30614,#30615),(#30616,#30617),(#30618,#30619),(#30620,
#30621),(#30622,#30623),(#30624,#30625),(#30626,#30627),(#30628,#30629),
(#30630,#30631),(#30632,#30633),(#30634,#30635),(#30636,#30637),(#30638,
#30639),(#30640,#30641),(#30642,#30643),(#30644,#30645),(#30646,#30647),
(#30648,#30649),(#30650,#30651),(#30652,#30653),(#30654,#30655),(#30656,
#30657),(#30658,#30659),(#30660,#30661),(#30662,#30663),(#30664,#30665),
(#30666,#30667),(#30668,#30669),(#30670,#30671),(#30672,#30673),(#30674,
#30675),(#30676,#30677),(#30678,#30679),(#30680,#30681),(#30682,#30683),
(#30684,#30685),(#30686,#30687),(#30688,#30689),(#30690,#30691),(#30692,
#30693),(#30694,#30695),(#30696,#30697),(#30698,#30699),(#30700,#30701),
(#30702,#30703),(#30704,#30705),(#30706,#30707),(#30708,#30709),(#30710,
#30711),(#30712,#30713),(#30714,#30715),(#30716,#30717),(#30718,#30719),
(#30720,#30721),(#30722,#30723),(#30724,#30725),(#30726,#30727),(#30728,
#30729),(#30730,#30731),(#30732,#30733),(#30734,#30735)),.UNSPECIFIED.,
 .F.,.F.,.F.)
B_SPLINE_SURFACE_WITH_KNOTS((6,1,1,1,1,1,1,1,1,1,1,1,1,1,1,1,1,1,1,1,1,
1,1,1,1,1,1,1,1,1,1,1,1,1,1,1,1,1,1,1,1,1,1,1,1,1,1,1,1,1,1,1,1,1,1,1,1,
1,1,1,1,1,1,1,1,6),(2,2),(-1.,-0.984615384615383,-0.969230769230768,-0.953846153846152,
-0.938461538461537,-0.923076923076922,-0.907692307692306,-0.892307692307691,
-0.876923076923076,-0.86153846153846,-0.846153846153845,-0.83076923076923,
-0.815384615384614,-0.799999999999999,-0.784615384615384,-0.769230769230768,
-0.753846153846153,-0.738461538461538,-0.723076923076922,-0.707692307692307,
-0.692307692307692,-0.676923076923076,-0.661538461538461,-0.646153846153846,
-0.63076923076923,-0.615384615384615,-0.6,-0.584615384615384,-0.569230769230769,
-0.553846153846154,-0.538461538461538,-0.523076923076923,-0.507692307692308,
-0.492307692307692,-0.476923076923077,-0.461538461538462,-0.446153846153846,
-0.430769230769231,-0.415384615384615,-0.4,-0.384615384615385,-0.369230769230769,
-0.353846153846154,-0.338461538461538,-0.323076923076923,-0.307692307692308,
-0.292307692307692,-0.276923076923077,-0.261538461538462,-0.246153846153846,
-0.230769230769231,-0.215384615384615,-0.2,-0.184615384615385,-0.169230769230769,
-0.153846153846154,-0.138461538461538,-0.123076923076923,-0.107692307692308,
-0.0923076923076923,-0.0769230769230769,-0.0615384615384615,-0.0461538461538462,
-0.0307692307692308,-0.0153846153846154,0.),(-1.,1.),.UNSPECIFIED.)
GEOMETRIC_REPRESENTATION_ITEM()
RATIONAL_B_SPLINE_SURFACE(((1.,1.),(1.,1.),(1.,1.),(1.,1.),(1.,1.),(1.,
1.),(1.,1.),(1.,1.),(1.,1.),(1.,1.),(1.,1.),(1.,1.),(1.,1.),(1.,1.),(1.,
1.),(1.,1.),(1.,1.),(1.,1.),(1.,1.),(1.,1.),(1.,1.),(1.,1.),(1.,1.),(1.,
1.),(1.,1.),(1.,1.),(1.,1.),(1.,1.),(1.,1.),(1.,1.),(1.,1.),(1.,1.),(1.,
1.),(1.,1.),(1.,1.),(1.,1.),(1.,1.),(1.,1.),(1.,1.),(1.,1.),(1.,1.),(1.,
1.),(1.,1.),(1.,1.),(1.,1.),(1.,1.),(1.,1.),(1.,1.),(1.,1.),(1.,1.),(1.,
1.),(1.,1.),(1.,1.),(1.,1.),(1.,1.),(1.,1.),(1.,1.),(1.,1.),(1.,1.),(1.,
1.),(1.,1.),(1.,1.),(1.,1.),(1.,1.),(1.,1.),(1.,1.),(1.,1.),(1.,1.),(1.,
1.),(1.,1.)))
REPRESENTATION_ITEM('')
SURFACE()
);
#16=(
BOUNDED_SURFACE()
B_SPLINE_SURFACE(5,1,((#30812,#30813),(#30814,#30815),(#30816,#30817),(#30818,
#30819),(#30820,#30821),(#30822,#30823),(#30824,#30825),(#30826,#30827),
(#30828,#30829),(#30830,#30831),(#30832,#30833),(#30834,#30835),(#30836,
#30837),(#30838,#30839),(#30840,#30841),(#30842,#30843),(#30844,#30845),
(#30846,#30847),(#30848,#30849),(#30850,#30851),(#30852,#30853),(#30854,
#30855),(#30856,#30857),(#30858,#30859),(#30860,#30861),(#30862,#30863),
(#30864,#30865),(#30866,#30867),(#30868,#30869),(#30870,#30871),(#30872,
#30873),(#30874,#30875),(#30876,#30877),(#30878,#30879),(#30880,#30881),
(#30882,#30883),(#30884,#30885),(#30886,#30887),(#30888,#30889),(#30890,
#30891),(#30892,#30893),(#30894,#30895),(#30896,#30897),(#30898,#30899),
(#30900,#30901),(#30902,#30903),(#30904,#30905),(#30906,#30907),(#30908,
#30909),(#30910,#30911),(#30912,#30913),(#30914,#30915),(#30916,#30917),
(#30918,#30919),(#30920,#30921),(#30922,#30923),(#30924,#30925),(#30926,
#30927),(#30928,#30929),(#30930,#30931),(#30932,#30933),(#30934,#30935),
(#30936,#30937),(#30938,#30939),(#30940,#30941),(#30942,#30943),(#30944,
#30945),(#30946,#30947),(#30948,#30949),(#30950,#30951)),.UNSPECIFIED.,
 .F.,.F.,.F.)
B_SPLINE_SURFACE_WITH_KNOTS((6,1,1,1,1,1,1,1,1,1,1,1,1,1,1,1,1,1,1,1,1,
1,1,1,1,1,1,1,1,1,1,1,1,1,1,1,1,1,1,1,1,1,1,1,1,1,1,1,1,1,1,1,1,1,1,1,1,
1,1,1,1,1,1,1,1,6),(2,2),(-1.,-0.984615384615383,-0.969230769230768,-0.953846153846152,
-0.938461538461537,-0.923076923076922,-0.907692307692306,-0.892307692307691,
-0.876923076923076,-0.86153846153846,-0.846153846153845,-0.83076923076923,
-0.815384615384614,-0.799999999999999,-0.784615384615384,-0.769230769230768,
-0.753846153846153,-0.738461538461538,-0.723076923076922,-0.707692307692307,
-0.692307692307692,-0.676923076923076,-0.661538461538461,-0.646153846153846,
-0.63076923076923,-0.615384615384615,-0.6,-0.584615384615384,-0.569230769230769,
-0.553846153846154,-0.538461538461538,-0.523076923076923,-0.507692307692308,
-0.492307692307692,-0.476923076923077,-0.461538461538462,-0.446153846153846,
-0.430769230769231,-0.415384615384615,-0.4,-0.384615384615385,-0.369230769230769,
-0.353846153846154,-0.338461538461538,-0.323076923076923,-0.307692307692308,
-0.292307692307692,-0.276923076923077,-0.261538461538462,-0.246153846153846,
-0.230769230769231,-0.215384615384615,-0.2,-0.184615384615385,-0.169230769230769,
-0.153846153846154,-0.138461538461538,-0.123076923076923,-0.107692307692308,
-0.0923076923076923,-0.0769230769230769,-0.0615384615384615,-0.0461538461538462,
-0.0307692307692308,-0.0153846153846154,0.),(-1.,1.),.UNSPECIFIED.)
GEOMETRIC_REPRESENTATION_ITEM()
RATIONAL_B_SPLINE_SURFACE(((1.,1.),(1.,1.),(1.,1.),(1.,1.),(1.,1.),(1.,
1.),(1.,1.),(1.,1.),(1.,1.),(1.,1.),(1.,1.),(1.,1.),(1.,1.),(1.,1.),(1.,
1.),(1.,1.),(1.,1.),(1.,1.),(1.,1.),(1.,1.),(1.,1.),(1.,1.),(1.,1.),(1.,
1.),(1.,1.),(1.,1.),(1.,1.),(1.,1.),(1.,1.),(1.,1.),(1.,1.),(1.,1.),(1.,
1.),(1.,1.),(1.,1.),(1.,1.),(1.,1.),(1.,1.),(1.,1.),(1.,1.),(1.,1.),(1.,
1.),(1.,1.),(1.,1.),(1.,1.),(1.,1.),(1.,1.),(1.,1.),(1.,1.),(1.,1.),(1.,
1.),(1.,1.),(1.,1.),(1.,1.),(1.,1.),(1.,1.),(1.,1.),(1.,1.),(1.,1.),(1.,
1.),(1.,1.),(1.,1.),(1.,1.),(1.,1.),(1.,1.),(1.,1.),(1.,1.),(1.,1.),(1.,
1.),(1.,1.)))
REPRESENTATION_ITEM('')
SURFACE()
);
#17=(
BOUNDED_SURFACE()
B_SPLINE_SURFACE(5,1,((#31028,#31029),(#31030,#31031),(#31032,#31033),(#31034,
#31035),(#31036,#31037),(#31038,#31039),(#31040,#31041),(#31042,#31043),
(#31044,#31045),(#31046,#31047),(#31048,#31049),(#31050,#31051),(#31052,
#31053),(#31054,#31055),(#31056,#31057),(#31058,#31059),(#31060,#31061),
(#31062,#31063),(#31064,#31065),(#31066,#31067),(#31068,#31069),(#31070,
#31071),(#31072,#31073),(#31074,#31075),(#31076,#31077),(#31078,#31079),
(#31080,#31081),(#31082,#31083),(#31084,#31085),(#31086,#31087),(#31088,
#31089),(#31090,#31091),(#31092,#31093),(#31094,#31095),(#31096,#31097),
(#31098,#31099),(#31100,#31101),(#31102,#31103),(#31104,#31105),(#31106,
#31107),(#31108,#31109),(#31110,#31111),(#31112,#31113),(#31114,#31115),
(#31116,#31117),(#31118,#31119),(#31120,#31121),(#31122,#31123),(#31124,
#31125),(#31126,#31127),(#31128,#31129),(#31130,#31131),(#31132,#31133),
(#31134,#31135),(#31136,#31137),(#31138,#31139),(#31140,#31141),(#31142,
#31143),(#31144,#31145),(#31146,#31147),(#31148,#31149),(#31150,#31151),
(#31152,#31153),(#31154,#31155),(#31156,#31157),(#31158,#31159),(#31160,
#31161),(#31162,#31163),(#31164,#31165),(#31166,#31167)),.UNSPECIFIED.,
 .F.,.F.,.F.)
B_SPLINE_SURFACE_WITH_KNOTS((6,1,1,1,1,1,1,1,1,1,1,1,1,1,1,1,1,1,1,1,1,
1,1,1,1,1,1,1,1,1,1,1,1,1,1,1,1,1,1,1,1,1,1,1,1,1,1,1,1,1,1,1,1,1,1,1,1,
1,1,1,1,1,1,1,1,6),(2,2),(-1.,-0.984615384615383,-0.969230769230768,-0.953846153846152,
-0.938461538461537,-0.923076923076922,-0.907692307692306,-0.892307692307691,
-0.876923076923076,-0.86153846153846,-0.846153846153845,-0.83076923076923,
-0.815384615384614,-0.799999999999999,-0.784615384615384,-0.769230769230768,
-0.753846153846153,-0.738461538461538,-0.723076923076922,-0.707692307692307,
-0.692307692307692,-0.676923076923076,-0.661538461538461,-0.646153846153846,
-0.63076923076923,-0.615384615384615,-0.6,-0.584615384615384,-0.569230769230769,
-0.553846153846154,-0.538461538461538,-0.523076923076923,-0.507692307692308,
-0.492307692307692,-0.476923076923077,-0.461538461538462,-0.446153846153846,
-0.430769230769231,-0.415384615384615,-0.4,-0.384615384615385,-0.369230769230769,
-0.353846153846154,-0.338461538461538,-0.323076923076923,-0.307692307692308,
-0.292307692307692,-0.276923076923077,-0.261538461538462,-0.246153846153846,
-0.230769230769231,-0.215384615384615,-0.2,-0.184615384615385,-0.169230769230769,
-0.153846153846154,-0.138461538461538,-0.123076923076923,-0.107692307692308,
-0.0923076923076923,-0.0769230769230769,-0.0615384615384615,-0.0461538461538462,
-0.0307692307692308,-0.0153846153846154,0.),(-1.,1.),.UNSPECIFIED.)
GEOMETRIC_REPRESENTATION_ITEM()
RATIONAL_B_SPLINE_SURFACE(((1.,1.),(1.,1.),(1.,1.),(1.,1.),(1.,1.),(1.,
1.),(1.,1.),(1.,1.),(1.,1.),(1.,1.),(1.,1.),(1.,1.),(1.,1.),(1.,1.),(1.,
1.),(1.,1.),(1.,1.),(1.,1.),(1.,1.),(1.,1.),(1.,1.),(1.,1.),(1.,1.),(1.,
1.),(1.,1.),(1.,1.),(1.,1.),(1.,1.),(1.,1.),(1.,1.),(1.,1.),(1.,1.),(1.,
1.),(1.,1.),(1.,1.),(1.,1.),(1.,1.),(1.,1.),(1.,1.),(1.,1.),(1.,1.),(1.,
1.),(1.,1.),(1.,1.),(1.,1.),(1.,1.),(1.,1.),(1.,1.),(1.,1.),(1.,1.),(1.,
1.),(1.,1.),(1.,1.),(1.,1.),(1.,1.),(1.,1.),(1.,1.),(1.,1.),(1.,1.),(1.,
1.),(1.,1.),(1.,1.),(1.,1.),(1.,1.),(1.,1.),(1.,1.),(1.,1.),(1.,1.),(1.,
1.),(1.,1.)))
REPRESENTATION_ITEM('')
SURFACE()
);
#18=(
BOUNDED_SURFACE()
B_SPLINE_SURFACE(5,1,((#31244,#31245),(#31246,#31247),(#31248,#31249),(#31250,
#31251),(#31252,#31253),(#31254,#31255),(#31256,#31257),(#31258,#31259),
(#31260,#31261),(#31262,#31263),(#31264,#31265),(#31266,#31267),(#31268,
#31269),(#31270,#31271),(#31272,#31273),(#31274,#31275),(#31276,#31277),
(#31278,#31279),(#31280,#31281),(#31282,#31283),(#31284,#31285),(#31286,
#31287),(#31288,#31289),(#31290,#31291),(#31292,#31293),(#31294,#31295),
(#31296,#31297),(#31298,#31299),(#31300,#31301),(#31302,#31303),(#31304,
#31305),(#31306,#31307),(#31308,#31309),(#31310,#31311),(#31312,#31313),
(#31314,#31315),(#31316,#31317),(#31318,#31319),(#31320,#31321),(#31322,
#31323),(#31324,#31325),(#31326,#31327),(#31328,#31329),(#31330,#31331),
(#31332,#31333),(#31334,#31335),(#31336,#31337),(#31338,#31339),(#31340,
#31341),(#31342,#31343),(#31344,#31345),(#31346,#31347),(#31348,#31349),
(#31350,#31351),(#31352,#31353),(#31354,#31355),(#31356,#31357),(#31358,
#31359),(#31360,#31361),(#31362,#31363),(#31364,#31365),(#31366,#31367),
(#31368,#31369),(#31370,#31371),(#31372,#31373),(#31374,#31375),(#31376,
#31377),(#31378,#31379),(#31380,#31381),(#31382,#31383)),.UNSPECIFIED.,
 .F.,.F.,.F.)
B_SPLINE_SURFACE_WITH_KNOTS((6,1,1,1,1,1,1,1,1,1,1,1,1,1,1,1,1,1,1,1,1,
1,1,1,1,1,1,1,1,1,1,1,1,1,1,1,1,1,1,1,1,1,1,1,1,1,1,1,1,1,1,1,1,1,1,1,1,
1,1,1,1,1,1,1,1,6),(2,2),(-1.,-0.984615384615383,-0.969230769230768,-0.953846153846152,
-0.938461538461537,-0.923076923076922,-0.907692307692306,-0.892307692307691,
-0.876923076923076,-0.86153846153846,-0.846153846153845,-0.83076923076923,
-0.815384615384614,-0.799999999999999,-0.784615384615384,-0.769230769230768,
-0.753846153846153,-0.738461538461538,-0.723076923076922,-0.707692307692307,
-0.692307692307692,-0.676923076923076,-0.661538461538461,-0.646153846153846,
-0.63076923076923,-0.615384615384615,-0.6,-0.584615384615384,-0.569230769230769,
-0.553846153846154,-0.538461538461538,-0.523076923076923,-0.507692307692308,
-0.492307692307692,-0.476923076923077,-0.461538461538462,-0.446153846153846,
-0.430769230769231,-0.415384615384615,-0.4,-0.384615384615385,-0.369230769230769,
-0.353846153846154,-0.338461538461538,-0.323076923076923,-0.307692307692308,
-0.292307692307692,-0.276923076923077,-0.261538461538462,-0.246153846153846,
-0.230769230769231,-0.215384615384615,-0.2,-0.184615384615385,-0.169230769230769,
-0.153846153846154,-0.138461538461538,-0.123076923076923,-0.107692307692308,
-0.0923076923076923,-0.0769230769230769,-0.0615384615384615,-0.0461538461538462,
-0.0307692307692308,-0.0153846153846154,0.),(-1.,1.),.UNSPECIFIED.)
GEOMETRIC_REPRESENTATION_ITEM()
RATIONAL_B_SPLINE_SURFACE(((1.,1.),(1.,1.),(1.,1.),(1.,1.),(1.,1.),(1.,
1.),(1.,1.),(1.,1.),(1.,1.),(1.,1.),(1.,1.),(1.,1.),(1.,1.),(1.,1.),(1.,
1.),(1.,1.),(1.,1.),(1.,1.),(1.,1.),(1.,1.),(1.,1.),(1.,1.),(1.,1.),(1.,
1.),(1.,1.),(1.,1.),(1.,1.),(1.,1.),(1.,1.),(1.,1.),(1.,1.),(1.,1.),(1.,
1.),(1.,1.),(1.,1.),(1.,1.),(1.,1.),(1.,1.),(1.,1.),(1.,1.),(1.,1.),(1.,
1.),(1.,1.),(1.,1.),(1.,1.),(1.,1.),(1.,1.),(1.,1.),(1.,1.),(1.,1.),(1.,
1.),(1.,1.),(1.,1.),(1.,1.),(1.,1.),(1.,1.),(1.,1.),(1.,1.),(1.,1.),(1.,
1.),(1.,1.),(1.,1.),(1.,1.),(1.,1.),(1.,1.),(1.,1.),(1.,1.),(1.,1.),(1.,
1.),(1.,1.)))
REPRESENTATION_ITEM('')
SURFACE()
);
#19=(
BOUNDED_SURFACE()
B_SPLINE_SURFACE(5,1,((#31460,#31461),(#31462,#31463),(#31464,#31465),(#31466,
#31467),(#31468,#31469),(#31470,#31471),(#31472,#31473),(#31474,#31475),
(#31476,#31477),(#31478,#31479),(#31480,#31481),(#31482,#31483),(#31484,
#31485),(#31486,#31487),(#31488,#31489),(#31490,#31491),(#31492,#31493),
(#31494,#31495),(#31496,#31497),(#31498,#31499),(#31500,#31501),(#31502,
#31503),(#31504,#31505),(#31506,#31507),(#31508,#31509),(#31510,#31511),
(#31512,#31513),(#31514,#31515),(#31516,#31517),(#31518,#31519),(#31520,
#31521),(#31522,#31523),(#31524,#31525),(#31526,#31527),(#31528,#31529),
(#31530,#31531),(#31532,#31533),(#31534,#31535),(#31536,#31537),(#31538,
#31539),(#31540,#31541),(#31542,#31543),(#31544,#31545),(#31546,#31547),
(#31548,#31549),(#31550,#31551),(#31552,#31553),(#31554,#31555),(#31556,
#31557),(#31558,#31559),(#31560,#31561),(#31562,#31563),(#31564,#31565),
(#31566,#31567),(#31568,#31569),(#31570,#31571),(#31572,#31573),(#31574,
#31575),(#31576,#31577),(#31578,#31579),(#31580,#31581),(#31582,#31583),
(#31584,#31585),(#31586,#31587),(#31588,#31589),(#31590,#31591),(#31592,
#31593),(#31594,#31595),(#31596,#31597),(#31598,#31599)),.UNSPECIFIED.,
 .F.,.F.,.F.)
B_SPLINE_SURFACE_WITH_KNOTS((6,1,1,1,1,1,1,1,1,1,1,1,1,1,1,1,1,1,1,1,1,
1,1,1,1,1,1,1,1,1,1,1,1,1,1,1,1,1,1,1,1,1,1,1,1,1,1,1,1,1,1,1,1,1,1,1,1,
1,1,1,1,1,1,1,1,6),(2,2),(-1.,-0.984615384615383,-0.969230769230768,-0.953846153846152,
-0.938461538461537,-0.923076923076922,-0.907692307692306,-0.892307692307691,
-0.876923076923076,-0.86153846153846,-0.846153846153845,-0.83076923076923,
-0.815384615384614,-0.799999999999999,-0.784615384615384,-0.769230769230768,
-0.753846153846153,-0.738461538461538,-0.723076923076922,-0.707692307692307,
-0.692307692307692,-0.676923076923076,-0.661538461538461,-0.646153846153846,
-0.63076923076923,-0.615384615384615,-0.6,-0.584615384615384,-0.569230769230769,
-0.553846153846154,-0.538461538461538,-0.523076923076923,-0.507692307692308,
-0.492307692307692,-0.476923076923077,-0.461538461538462,-0.446153846153846,
-0.430769230769231,-0.415384615384615,-0.4,-0.384615384615385,-0.369230769230769,
-0.353846153846154,-0.338461538461538,-0.323076923076923,-0.307692307692308,
-0.292307692307692,-0.276923076923077,-0.261538461538462,-0.246153846153846,
-0.230769230769231,-0.215384615384615,-0.2,-0.184615384615385,-0.169230769230769,
-0.153846153846154,-0.138461538461538,-0.123076923076923,-0.107692307692308,
-0.0923076923076923,-0.0769230769230769,-0.0615384615384615,-0.0461538461538462,
-0.0307692307692308,-0.0153846153846154,0.),(-1.,1.),.UNSPECIFIED.)
GEOMETRIC_REPRESENTATION_ITEM()
RATIONAL_B_SPLINE_SURFACE(((1.,1.),(1.,1.),(1.,1.),(1.,1.),(1.,1.),(1.,
1.),(1.,1.),(1.,1.),(1.,1.),(1.,1.),(1.,1.),(1.,1.),(1.,1.),(1.,1.),(1.,
1.),(1.,1.),(1.,1.),(1.,1.),(1.,1.),(1.,1.),(1.,1.),(1.,1.),(1.,1.),(1.,
1.),(1.,1.),(1.,1.),(1.,1.),(1.,1.),(1.,1.),(1.,1.),(1.,1.),(1.,1.),(1.,
1.),(1.,1.),(1.,1.),(1.,1.),(1.,1.),(1.,1.),(1.,1.),(1.,1.),(1.,1.),(1.,
1.),(1.,1.),(1.,1.),(1.,1.),(1.,1.),(1.,1.),(1.,1.),(1.,1.),(1.,1.),(1.,
1.),(1.,1.),(1.,1.),(1.,1.),(1.,1.),(1.,1.),(1.,1.),(1.,1.),(1.,1.),(1.,
1.),(1.,1.),(1.,1.),(1.,1.),(1.,1.),(1.,1.),(1.,1.),(1.,1.),(1.,1.),(1.,
1.),(1.,1.)))
REPRESENTATION_ITEM('')
SURFACE()
);
#20=(
BOUNDED_SURFACE()
B_SPLINE_SURFACE(5,1,((#31676,#31677),(#31678,#31679),(#31680,#31681),(#31682,
#31683),(#31684,#31685),(#31686,#31687),(#31688,#31689),(#31690,#31691),
(#31692,#31693),(#31694,#31695),(#31696,#31697),(#31698,#31699),(#31700,
#31701),(#31702,#31703),(#31704,#31705),(#31706,#31707),(#31708,#31709),
(#31710,#31711),(#31712,#31713),(#31714,#31715),(#31716,#31717),(#31718,
#31719),(#31720,#31721),(#31722,#31723),(#31724,#31725),(#31726,#31727),
(#31728,#31729),(#31730,#31731),(#31732,#31733),(#31734,#31735),(#31736,
#31737),(#31738,#31739),(#31740,#31741),(#31742,#31743),(#31744,#31745),
(#31746,#31747),(#31748,#31749),(#31750,#31751),(#31752,#31753),(#31754,
#31755),(#31756,#31757),(#31758,#31759),(#31760,#31761),(#31762,#31763),
(#31764,#31765),(#31766,#31767),(#31768,#31769),(#31770,#31771),(#31772,
#31773),(#31774,#31775),(#31776,#31777),(#31778,#31779),(#31780,#31781),
(#31782,#31783),(#31784,#31785),(#31786,#31787),(#31788,#31789),(#31790,
#31791),(#31792,#31793),(#31794,#31795),(#31796,#31797),(#31798,#31799),
(#31800,#31801),(#31802,#31803),(#31804,#31805),(#31806,#31807),(#31808,
#31809),(#31810,#31811),(#31812,#31813),(#31814,#31815)),.UNSPECIFIED.,
 .F.,.F.,.F.)
B_SPLINE_SURFACE_WITH_KNOTS((6,1,1,1,1,1,1,1,1,1,1,1,1,1,1,1,1,1,1,1,1,
1,1,1,1,1,1,1,1,1,1,1,1,1,1,1,1,1,1,1,1,1,1,1,1,1,1,1,1,1,1,1,1,1,1,1,1,
1,1,1,1,1,1,1,1,6),(2,2),(-1.,-0.984615384615383,-0.969230769230768,-0.953846153846152,
-0.938461538461537,-0.923076923076922,-0.907692307692306,-0.892307692307691,
-0.876923076923076,-0.86153846153846,-0.846153846153845,-0.83076923076923,
-0.815384615384614,-0.799999999999999,-0.784615384615384,-0.769230769230768,
-0.753846153846153,-0.738461538461538,-0.723076923076922,-0.707692307692307,
-0.692307692307692,-0.676923076923076,-0.661538461538461,-0.646153846153846,
-0.63076923076923,-0.615384615384615,-0.6,-0.584615384615384,-0.569230769230769,
-0.553846153846154,-0.538461538461538,-0.523076923076923,-0.507692307692308,
-0.492307692307692,-0.476923076923077,-0.461538461538462,-0.446153846153846,
-0.430769230769231,-0.415384615384615,-0.4,-0.384615384615385,-0.369230769230769,
-0.353846153846154,-0.338461538461538,-0.323076923076923,-0.307692307692308,
-0.292307692307692,-0.276923076923077,-0.261538461538462,-0.246153846153846,
-0.230769230769231,-0.215384615384615,-0.2,-0.184615384615385,-0.169230769230769,
-0.153846153846154,-0.138461538461538,-0.123076923076923,-0.107692307692308,
-0.0923076923076923,-0.0769230769230769,-0.0615384615384615,-0.0461538461538462,
-0.0307692307692308,-0.0153846153846154,0.),(-1.,1.),.UNSPECIFIED.)
GEOMETRIC_REPRESENTATION_ITEM()
RATIONAL_B_SPLINE_SURFACE(((1.,1.),(1.,1.),(1.,1.),(1.,1.),(1.,1.),(1.,
1.),(1.,1.),(1.,1.),(1.,1.),(1.,1.),(1.,1.),(1.,1.),(1.,1.),(1.,1.),(1.,
1.),(1.,1.),(1.,1.),(1.,1.),(1.,1.),(1.,1.),(1.,1.),(1.,1.),(1.,1.),(1.,
1.),(1.,1.),(1.,1.),(1.,1.),(1.,1.),(1.,1.),(1.,1.),(1.,1.),(1.,1.),(1.,
1.),(1.,1.),(1.,1.),(1.,1.),(1.,1.),(1.,1.),(1.,1.),(1.,1.),(1.,1.),(1.,
1.),(1.,1.),(1.,1.),(1.,1.),(1.,1.),(1.,1.),(1.,1.),(1.,1.),(1.,1.),(1.,
1.),(1.,1.),(1.,1.),(1.,1.),(1.,1.),(1.,1.),(1.,1.),(1.,1.),(1.,1.),(1.,
1.),(1.,1.),(1.,1.),(1.,1.),(1.,1.),(1.,1.),(1.,1.),(1.,1.),(1.,1.),(1.,
1.),(1.,1.)))
REPRESENTATION_ITEM('')
SURFACE()
);
#21=(
BOUNDED_SURFACE()
B_SPLINE_SURFACE(5,1,((#31892,#31893),(#31894,#31895),(#31896,#31897),(#31898,
#31899),(#31900,#31901),(#31902,#31903),(#31904,#31905),(#31906,#31907),
(#31908,#31909),(#31910,#31911),(#31912,#31913),(#31914,#31915),(#31916,
#31917),(#31918,#31919),(#31920,#31921),(#31922,#31923),(#31924,#31925),
(#31926,#31927),(#31928,#31929),(#31930,#31931),(#31932,#31933),(#31934,
#31935),(#31936,#31937),(#31938,#31939),(#31940,#31941),(#31942,#31943),
(#31944,#31945),(#31946,#31947),(#31948,#31949),(#31950,#31951),(#31952,
#31953),(#31954,#31955),(#31956,#31957),(#31958,#31959),(#31960,#31961),
(#31962,#31963),(#31964,#31965),(#31966,#31967),(#31968,#31969),(#31970,
#31971),(#31972,#31973),(#31974,#31975),(#31976,#31977),(#31978,#31979),
(#31980,#31981),(#31982,#31983),(#31984,#31985),(#31986,#31987),(#31988,
#31989),(#31990,#31991),(#31992,#31993),(#31994,#31995),(#31996,#31997),
(#31998,#31999),(#32000,#32001),(#32002,#32003),(#32004,#32005),(#32006,
#32007),(#32008,#32009),(#32010,#32011),(#32012,#32013),(#32014,#32015),
(#32016,#32017),(#32018,#32019),(#32020,#32021),(#32022,#32023),(#32024,
#32025),(#32026,#32027),(#32028,#32029),(#32030,#32031)),.UNSPECIFIED.,
 .F.,.F.,.F.)
B_SPLINE_SURFACE_WITH_KNOTS((6,1,1,1,1,1,1,1,1,1,1,1,1,1,1,1,1,1,1,1,1,
1,1,1,1,1,1,1,1,1,1,1,1,1,1,1,1,1,1,1,1,1,1,1,1,1,1,1,1,1,1,1,1,1,1,1,1,
1,1,1,1,1,1,1,1,6),(2,2),(-1.,-0.984615384615383,-0.969230769230768,-0.953846153846152,
-0.938461538461537,-0.923076923076922,-0.907692307692306,-0.892307692307691,
-0.876923076923076,-0.86153846153846,-0.846153846153845,-0.83076923076923,
-0.815384615384614,-0.799999999999999,-0.784615384615384,-0.769230769230768,
-0.753846153846153,-0.738461538461538,-0.723076923076922,-0.707692307692307,
-0.692307692307692,-0.676923076923076,-0.661538461538461,-0.646153846153846,
-0.63076923076923,-0.615384615384615,-0.6,-0.584615384615384,-0.569230769230769,
-0.553846153846154,-0.538461538461538,-0.523076923076923,-0.507692307692308,
-0.492307692307692,-0.476923076923077,-0.461538461538462,-0.446153846153846,
-0.430769230769231,-0.415384615384615,-0.4,-0.384615384615385,-0.369230769230769,
-0.353846153846154,-0.338461538461538,-0.323076923076923,-0.307692307692308,
-0.292307692307692,-0.276923076923077,-0.261538461538462,-0.246153846153846,
-0.230769230769231,-0.215384615384615,-0.2,-0.184615384615385,-0.169230769230769,
-0.153846153846154,-0.138461538461538,-0.123076923076923,-0.107692307692308,
-0.0923076923076923,-0.0769230769230769,-0.0615384615384615,-0.0461538461538462,
-0.0307692307692308,-0.0153846153846154,0.),(-1.,1.),.UNSPECIFIED.)
GEOMETRIC_REPRESENTATION_ITEM()
RATIONAL_B_SPLINE_SURFACE(((1.,1.),(1.,1.),(1.,1.),(1.,1.),(1.,1.),(1.,
1.),(1.,1.),(1.,1.),(1.,1.),(1.,1.),(1.,1.),(1.,1.),(1.,1.),(1.,1.),(1.,
1.),(1.,1.),(1.,1.),(1.,1.),(1.,1.),(1.,1.),(1.,1.),(1.,1.),(1.,1.),(1.,
1.),(1.,1.),(1.,1.),(1.,1.),(1.,1.),(1.,1.),(1.,1.),(1.,1.),(1.,1.),(1.,
1.),(1.,1.),(1.,1.),(1.,1.),(1.,1.),(1.,1.),(1.,1.),(1.,1.),(1.,1.),(1.,
1.),(1.,1.),(1.,1.),(1.,1.),(1.,1.),(1.,1.),(1.,1.),(1.,1.),(1.,1.),(1.,
1.),(1.,1.),(1.,1.),(1.,1.),(1.,1.),(1.,1.),(1.,1.),(1.,1.),(1.,1.),(1.,
1.),(1.,1.),(1.,1.),(1.,1.),(1.,1.),(1.,1.),(1.,1.),(1.,1.),(1.,1.),(1.,
1.),(1.,1.)))
REPRESENTATION_ITEM('')
SURFACE()
);
#22=(
BOUNDED_SURFACE()
B_SPLINE_SURFACE(5,1,((#32108,#32109),(#32110,#32111),(#32112,#32113),(#32114,
#32115),(#32116,#32117),(#32118,#32119),(#32120,#32121),(#32122,#32123),
(#32124,#32125),(#32126,#32127),(#32128,#32129),(#32130,#32131),(#32132,
#32133),(#32134,#32135),(#32136,#32137),(#32138,#32139),(#32140,#32141),
(#32142,#32143),(#32144,#32145),(#32146,#32147),(#32148,#32149),(#32150,
#32151),(#32152,#32153),(#32154,#32155),(#32156,#32157),(#32158,#32159),
(#32160,#32161),(#32162,#32163),(#32164,#32165),(#32166,#32167),(#32168,
#32169),(#32170,#32171),(#32172,#32173),(#32174,#32175),(#32176,#32177),
(#32178,#32179),(#32180,#32181),(#32182,#32183),(#32184,#32185),(#32186,
#32187),(#32188,#32189),(#32190,#32191),(#32192,#32193),(#32194,#32195),
(#32196,#32197),(#32198,#32199),(#32200,#32201),(#32202,#32203),(#32204,
#32205),(#32206,#32207),(#32208,#32209),(#32210,#32211),(#32212,#32213),
(#32214,#32215),(#32216,#32217),(#32218,#32219),(#32220,#32221),(#32222,
#32223),(#32224,#32225),(#32226,#32227),(#32228,#32229),(#32230,#32231),
(#32232,#32233),(#32234,#32235),(#32236,#32237),(#32238,#32239),(#32240,
#32241),(#32242,#32243),(#32244,#32245),(#32246,#32247)),.UNSPECIFIED.,
 .F.,.F.,.F.)
B_SPLINE_SURFACE_WITH_KNOTS((6,1,1,1,1,1,1,1,1,1,1,1,1,1,1,1,1,1,1,1,1,
1,1,1,1,1,1,1,1,1,1,1,1,1,1,1,1,1,1,1,1,1,1,1,1,1,1,1,1,1,1,1,1,1,1,1,1,
1,1,1,1,1,1,1,1,6),(2,2),(-1.,-0.984615384615383,-0.969230769230768,-0.953846153846152,
-0.938461538461537,-0.923076923076922,-0.907692307692306,-0.892307692307691,
-0.876923076923076,-0.86153846153846,-0.846153846153845,-0.83076923076923,
-0.815384615384614,-0.799999999999999,-0.784615384615384,-0.769230769230768,
-0.753846153846153,-0.738461538461538,-0.723076923076922,-0.707692307692307,
-0.692307692307692,-0.676923076923076,-0.661538461538461,-0.646153846153846,
-0.63076923076923,-0.615384615384615,-0.6,-0.584615384615384,-0.569230769230769,
-0.553846153846154,-0.538461538461538,-0.523076923076923,-0.507692307692308,
-0.492307692307692,-0.476923076923077,-0.461538461538462,-0.446153846153846,
-0.430769230769231,-0.415384615384615,-0.4,-0.384615384615385,-0.369230769230769,
-0.353846153846154,-0.338461538461538,-0.323076923076923,-0.307692307692308,
-0.292307692307692,-0.276923076923077,-0.261538461538462,-0.246153846153846,
-0.230769230769231,-0.215384615384615,-0.2,-0.184615384615385,-0.169230769230769,
-0.153846153846154,-0.138461538461538,-0.123076923076923,-0.107692307692308,
-0.0923076923076923,-0.0769230769230769,-0.0615384615384615,-0.0461538461538462,
-0.0307692307692308,-0.0153846153846154,0.),(-1.,1.),.UNSPECIFIED.)
GEOMETRIC_REPRESENTATION_ITEM()
RATIONAL_B_SPLINE_SURFACE(((1.,1.),(1.,1.),(1.,1.),(1.,1.),(1.,1.),(1.,
1.),(1.,1.),(1.,1.),(1.,1.),(1.,1.),(1.,1.),(1.,1.),(1.,1.),(1.,1.),(1.,
1.),(1.,1.),(1.,1.),(1.,1.),(1.,1.),(1.,1.),(1.,1.),(1.,1.),(1.,1.),(1.,
1.),(1.,1.),(1.,1.),(1.,1.),(1.,1.),(1.,1.),(1.,1.),(1.,1.),(1.,1.),(1.,
1.),(1.,1.),(1.,1.),(1.,1.),(1.,1.),(1.,1.),(1.,1.),(1.,1.),(1.,1.),(1.,
1.),(1.,1.),(1.,1.),(1.,1.),(1.,1.),(1.,1.),(1.,1.),(1.,1.),(1.,1.),(1.,
1.),(1.,1.),(1.,1.),(1.,1.),(1.,1.),(1.,1.),(1.,1.),(1.,1.),(1.,1.),(1.,
1.),(1.,1.),(1.,1.),(1.,1.),(1.,1.),(1.,1.),(1.,1.),(1.,1.),(1.,1.),(1.,
1.),(1.,1.)))
REPRESENTATION_ITEM('')
SURFACE()
);
#23=(
BOUNDED_SURFACE()
B_SPLINE_SURFACE(5,1,((#32324,#32325),(#32326,#32327),(#32328,#32329),(#32330,
#32331),(#32332,#32333),(#32334,#32335),(#32336,#32337),(#32338,#32339),
(#32340,#32341),(#32342,#32343),(#32344,#32345),(#32346,#32347),(#32348,
#32349),(#32350,#32351),(#32352,#32353),(#32354,#32355),(#32356,#32357),
(#32358,#32359),(#32360,#32361),(#32362,#32363),(#32364,#32365),(#32366,
#32367),(#32368,#32369),(#32370,#32371),(#32372,#32373),(#32374,#32375),
(#32376,#32377),(#32378,#32379),(#32380,#32381),(#32382,#32383),(#32384,
#32385),(#32386,#32387),(#32388,#32389),(#32390,#32391),(#32392,#32393),
(#32394,#32395),(#32396,#32397),(#32398,#32399),(#32400,#32401),(#32402,
#32403),(#32404,#32405),(#32406,#32407),(#32408,#32409),(#32410,#32411),
(#32412,#32413),(#32414,#32415),(#32416,#32417),(#32418,#32419),(#32420,
#32421),(#32422,#32423),(#32424,#32425),(#32426,#32427),(#32428,#32429),
(#32430,#32431),(#32432,#32433),(#32434,#32435),(#32436,#32437),(#32438,
#32439),(#32440,#32441),(#32442,#32443),(#32444,#32445),(#32446,#32447),
(#32448,#32449),(#32450,#32451),(#32452,#32453),(#32454,#32455),(#32456,
#32457),(#32458,#32459),(#32460,#32461),(#32462,#32463)),.UNSPECIFIED.,
 .F.,.F.,.F.)
B_SPLINE_SURFACE_WITH_KNOTS((6,1,1,1,1,1,1,1,1,1,1,1,1,1,1,1,1,1,1,1,1,
1,1,1,1,1,1,1,1,1,1,1,1,1,1,1,1,1,1,1,1,1,1,1,1,1,1,1,1,1,1,1,1,1,1,1,1,
1,1,1,1,1,1,1,1,6),(2,2),(-1.,-0.984615384615383,-0.969230769230768,-0.953846153846152,
-0.938461538461537,-0.923076923076922,-0.907692307692306,-0.892307692307691,
-0.876923076923076,-0.86153846153846,-0.846153846153845,-0.83076923076923,
-0.815384615384614,-0.799999999999999,-0.784615384615384,-0.769230769230768,
-0.753846153846153,-0.738461538461538,-0.723076923076922,-0.707692307692307,
-0.692307692307692,-0.676923076923076,-0.661538461538461,-0.646153846153846,
-0.63076923076923,-0.615384615384615,-0.6,-0.584615384615384,-0.569230769230769,
-0.553846153846154,-0.538461538461538,-0.523076923076923,-0.507692307692308,
-0.492307692307692,-0.476923076923077,-0.461538461538462,-0.446153846153846,
-0.430769230769231,-0.415384615384615,-0.4,-0.384615384615385,-0.369230769230769,
-0.353846153846154,-0.338461538461538,-0.323076923076923,-0.307692307692308,
-0.292307692307692,-0.276923076923077,-0.261538461538462,-0.246153846153846,
-0.230769230769231,-0.215384615384615,-0.2,-0.184615384615385,-0.169230769230769,
-0.153846153846154,-0.138461538461538,-0.123076923076923,-0.107692307692308,
-0.0923076923076923,-0.0769230769230769,-0.0615384615384615,-0.0461538461538462,
-0.0307692307692308,-0.0153846153846154,0.),(-1.,1.),.UNSPECIFIED.)
GEOMETRIC_REPRESENTATION_ITEM()
RATIONAL_B_SPLINE_SURFACE(((1.,1.),(1.,1.),(1.,1.),(1.,1.),(1.,1.),(1.,
1.),(1.,1.),(1.,1.),(1.,1.),(1.,1.),(1.,1.),(1.,1.),(1.,1.),(1.,1.),(1.,
1.),(1.,1.),(1.,1.),(1.,1.),(1.,1.),(1.,1.),(1.,1.),(1.,1.),(1.,1.),(1.,
1.),(1.,1.),(1.,1.),(1.,1.),(1.,1.),(1.,1.),(1.,1.),(1.,1.),(1.,1.),(1.,
1.),(1.,1.),(1.,1.),(1.,1.),(1.,1.),(1.,1.),(1.,1.),(1.,1.),(1.,1.),(1.,
1.),(1.,1.),(1.,1.),(1.,1.),(1.,1.),(1.,1.),(1.,1.),(1.,1.),(1.,1.),(1.,
1.),(1.,1.),(1.,1.),(1.,1.),(1.,1.),(1.,1.),(1.,1.),(1.,1.),(1.,1.),(1.,
1.),(1.,1.),(1.,1.),(1.,1.),(1.,1.),(1.,1.),(1.,1.),(1.,1.),(1.,1.),(1.,
1.),(1.,1.)))
REPRESENTATION_ITEM('')
SURFACE()
);
#24=(
BOUNDED_SURFACE()
B_SPLINE_SURFACE(5,1,((#32540,#32541),(#32542,#32543),(#32544,#32545),(#32546,
#32547),(#32548,#32549),(#32550,#32551),(#32552,#32553),(#32554,#32555),
(#32556,#32557),(#32558,#32559),(#32560,#32561),(#32562,#32563),(#32564,
#32565),(#32566,#32567),(#32568,#32569),(#32570,#32571),(#32572,#32573),
(#32574,#32575),(#32576,#32577),(#32578,#32579),(#32580,#32581),(#32582,
#32583),(#32584,#32585),(#32586,#32587),(#32588,#32589),(#32590,#32591),
(#32592,#32593),(#32594,#32595),(#32596,#32597),(#32598,#32599),(#32600,
#32601),(#32602,#32603),(#32604,#32605),(#32606,#32607),(#32608,#32609),
(#32610,#32611),(#32612,#32613),(#32614,#32615),(#32616,#32617),(#32618,
#32619),(#32620,#32621),(#32622,#32623),(#32624,#32625),(#32626,#32627),
(#32628,#32629),(#32630,#32631),(#32632,#32633),(#32634,#32635),(#32636,
#32637),(#32638,#32639),(#32640,#32641),(#32642,#32643),(#32644,#32645),
(#32646,#32647),(#32648,#32649),(#32650,#32651),(#32652,#32653),(#32654,
#32655),(#32656,#32657),(#32658,#32659),(#32660,#32661),(#32662,#32663),
(#32664,#32665),(#32666,#32667),(#32668,#32669),(#32670,#32671),(#32672,
#32673),(#32674,#32675),(#32676,#32677),(#32678,#32679)),.UNSPECIFIED.,
 .F.,.F.,.F.)
B_SPLINE_SURFACE_WITH_KNOTS((6,1,1,1,1,1,1,1,1,1,1,1,1,1,1,1,1,1,1,1,1,
1,1,1,1,1,1,1,1,1,1,1,1,1,1,1,1,1,1,1,1,1,1,1,1,1,1,1,1,1,1,1,1,1,1,1,1,
1,1,1,1,1,1,1,1,6),(2,2),(-1.,-0.984615384615383,-0.969230769230768,-0.953846153846152,
-0.938461538461537,-0.923076923076922,-0.907692307692306,-0.892307692307691,
-0.876923076923076,-0.86153846153846,-0.846153846153845,-0.83076923076923,
-0.815384615384614,-0.799999999999999,-0.784615384615384,-0.769230769230768,
-0.753846153846153,-0.738461538461538,-0.723076923076922,-0.707692307692307,
-0.692307692307692,-0.676923076923076,-0.661538461538461,-0.646153846153846,
-0.63076923076923,-0.615384615384615,-0.6,-0.584615384615384,-0.569230769230769,
-0.553846153846154,-0.538461538461538,-0.523076923076923,-0.507692307692308,
-0.492307692307692,-0.476923076923077,-0.461538461538462,-0.446153846153846,
-0.430769230769231,-0.415384615384615,-0.4,-0.384615384615385,-0.369230769230769,
-0.353846153846154,-0.338461538461538,-0.323076923076923,-0.307692307692308,
-0.292307692307692,-0.276923076923077,-0.261538461538462,-0.246153846153846,
-0.230769230769231,-0.215384615384615,-0.2,-0.184615384615385,-0.169230769230769,
-0.153846153846154,-0.138461538461538,-0.123076923076923,-0.107692307692308,
-0.0923076923076923,-0.0769230769230769,-0.0615384615384615,-0.0461538461538462,
-0.0307692307692308,-0.0153846153846154,0.),(-1.,1.),.UNSPECIFIED.)
GEOMETRIC_REPRESENTATION_ITEM()
RATIONAL_B_SPLINE_SURFACE(((1.,1.),(1.,1.),(1.,1.),(1.,1.),(1.,1.),(1.,
1.),(1.,1.),(1.,1.),(1.,1.),(1.,1.),(1.,1.),(1.,1.),(1.,1.),(1.,1.),(1.,
1.),(1.,1.),(1.,1.),(1.,1.),(1.,1.),(1.,1.),(1.,1.),(1.,1.),(1.,1.),(1.,
1.),(1.,1.),(1.,1.),(1.,1.),(1.,1.),(1.,1.),(1.,1.),(1.,1.),(1.,1.),(1.,
1.),(1.,1.),(1.,1.),(1.,1.),(1.,1.),(1.,1.),(1.,1.),(1.,1.),(1.,1.),(1.,
1.),(1.,1.),(1.,1.),(1.,1.),(1.,1.),(1.,1.),(1.,1.),(1.,1.),(1.,1.),(1.,
1.),(1.,1.),(1.,1.),(1.,1.),(1.,1.),(1.,1.),(1.,1.),(1.,1.),(1.,1.),(1.,
1.),(1.,1.),(1.,1.),(1.,1.),(1.,1.),(1.,1.),(1.,1.),(1.,1.),(1.,1.),(1.,
1.),(1.,1.)))
REPRESENTATION_ITEM('')
SURFACE()
);
#25=(
BOUNDED_SURFACE()
B_SPLINE_SURFACE(5,1,((#32756,#32757),(#32758,#32759),(#32760,#32761),(#32762,
#32763),(#32764,#32765),(#32766,#32767),(#32768,#32769),(#32770,#32771),
(#32772,#32773),(#32774,#32775),(#32776,#32777),(#32778,#32779),(#32780,
#32781),(#32782,#32783),(#32784,#32785),(#32786,#32787),(#32788,#32789),
(#32790,#32791),(#32792,#32793),(#32794,#32795),(#32796,#32797),(#32798,
#32799),(#32800,#32801),(#32802,#32803),(#32804,#32805),(#32806,#32807),
(#32808,#32809),(#32810,#32811),(#32812,#32813),(#32814,#32815),(#32816,
#32817),(#32818,#32819),(#32820,#32821),(#32822,#32823),(#32824,#32825),
(#32826,#32827),(#32828,#32829),(#32830,#32831),(#32832,#32833),(#32834,
#32835),(#32836,#32837),(#32838,#32839),(#32840,#32841),(#32842,#32843),
(#32844,#32845),(#32846,#32847),(#32848,#32849),(#32850,#32851),(#32852,
#32853),(#32854,#32855),(#32856,#32857),(#32858,#32859),(#32860,#32861),
(#32862,#32863),(#32864,#32865),(#32866,#32867),(#32868,#32869),(#32870,
#32871),(#32872,#32873),(#32874,#32875),(#32876,#32877),(#32878,#32879),
(#32880,#32881),(#32882,#32883),(#32884,#32885),(#32886,#32887),(#32888,
#32889),(#32890,#32891),(#32892,#32893),(#32894,#32895)),.UNSPECIFIED.,
 .F.,.F.,.F.)
B_SPLINE_SURFACE_WITH_KNOTS((6,1,1,1,1,1,1,1,1,1,1,1,1,1,1,1,1,1,1,1,1,
1,1,1,1,1,1,1,1,1,1,1,1,1,1,1,1,1,1,1,1,1,1,1,1,1,1,1,1,1,1,1,1,1,1,1,1,
1,1,1,1,1,1,1,1,6),(2,2),(-1.,-0.984615384615383,-0.969230769230768,-0.953846153846152,
-0.938461538461537,-0.923076923076922,-0.907692307692306,-0.892307692307691,
-0.876923076923076,-0.86153846153846,-0.846153846153845,-0.83076923076923,
-0.815384615384614,-0.799999999999999,-0.784615384615384,-0.769230769230768,
-0.753846153846153,-0.738461538461538,-0.723076923076922,-0.707692307692307,
-0.692307692307692,-0.676923076923076,-0.661538461538461,-0.646153846153846,
-0.63076923076923,-0.615384615384615,-0.6,-0.584615384615384,-0.569230769230769,
-0.553846153846154,-0.538461538461538,-0.523076923076923,-0.507692307692308,
-0.492307692307692,-0.476923076923077,-0.461538461538462,-0.446153846153846,
-0.430769230769231,-0.415384615384615,-0.4,-0.384615384615385,-0.369230769230769,
-0.353846153846154,-0.338461538461538,-0.323076923076923,-0.307692307692308,
-0.292307692307692,-0.276923076923077,-0.261538461538462,-0.246153846153846,
-0.230769230769231,-0.215384615384615,-0.2,-0.184615384615385,-0.169230769230769,
-0.153846153846154,-0.138461538461538,-0.123076923076923,-0.107692307692308,
-0.0923076923076923,-0.0769230769230769,-0.0615384615384615,-0.0461538461538462,
-0.0307692307692308,-0.0153846153846154,0.),(-1.,1.),.UNSPECIFIED.)
GEOMETRIC_REPRESENTATION_ITEM()
RATIONAL_B_SPLINE_SURFACE(((1.,1.),(1.,1.),(1.,1.),(1.,1.),(1.,1.),(1.,
1.),(1.,1.),(1.,1.),(1.,1.),(1.,1.),(1.,1.),(1.,1.),(1.,1.),(1.,1.),(1.,
1.),(1.,1.),(1.,1.),(1.,1.),(1.,1.),(1.,1.),(1.,1.),(1.,1.),(1.,1.),(1.,
1.),(1.,1.),(1.,1.),(1.,1.),(1.,1.),(1.,1.),(1.,1.),(1.,1.),(1.,1.),(1.,
1.),(1.,1.),(1.,1.),(1.,1.),(1.,1.),(1.,1.),(1.,1.),(1.,1.),(1.,1.),(1.,
1.),(1.,1.),(1.,1.),(1.,1.),(1.,1.),(1.,1.),(1.,1.),(1.,1.),(1.,1.),(1.,
1.),(1.,1.),(1.,1.),(1.,1.),(1.,1.),(1.,1.),(1.,1.),(1.,1.),(1.,1.),(1.,
1.),(1.,1.),(1.,1.),(1.,1.),(1.,1.),(1.,1.),(1.,1.),(1.,1.),(1.,1.),(1.,
1.),(1.,1.)))
REPRESENTATION_ITEM('')
SURFACE()
);
#26=(
BOUNDED_SURFACE()
B_SPLINE_SURFACE(5,1,((#32972,#32973),(#32974,#32975),(#32976,#32977),(#32978,
#32979),(#32980,#32981),(#32982,#32983),(#32984,#32985),(#32986,#32987),
(#32988,#32989),(#32990,#32991),(#32992,#32993),(#32994,#32995),(#32996,
#32997),(#32998,#32999),(#33000,#33001),(#33002,#33003),(#33004,#33005),
(#33006,#33007),(#33008,#33009),(#33010,#33011),(#33012,#33013),(#33014,
#33015),(#33016,#33017),(#33018,#33019),(#33020,#33021),(#33022,#33023),
(#33024,#33025),(#33026,#33027),(#33028,#33029),(#33030,#33031),(#33032,
#33033),(#33034,#33035),(#33036,#33037),(#33038,#33039),(#33040,#33041),
(#33042,#33043),(#33044,#33045),(#33046,#33047),(#33048,#33049),(#33050,
#33051),(#33052,#33053),(#33054,#33055),(#33056,#33057),(#33058,#33059),
(#33060,#33061),(#33062,#33063),(#33064,#33065),(#33066,#33067),(#33068,
#33069),(#33070,#33071),(#33072,#33073),(#33074,#33075),(#33076,#33077),
(#33078,#33079),(#33080,#33081),(#33082,#33083),(#33084,#33085),(#33086,
#33087),(#33088,#33089),(#33090,#33091),(#33092,#33093),(#33094,#33095),
(#33096,#33097),(#33098,#33099),(#33100,#33101),(#33102,#33103),(#33104,
#33105),(#33106,#33107),(#33108,#33109),(#33110,#33111)),.UNSPECIFIED.,
 .F.,.F.,.F.)
B_SPLINE_SURFACE_WITH_KNOTS((6,1,1,1,1,1,1,1,1,1,1,1,1,1,1,1,1,1,1,1,1,
1,1,1,1,1,1,1,1,1,1,1,1,1,1,1,1,1,1,1,1,1,1,1,1,1,1,1,1,1,1,1,1,1,1,1,1,
1,1,1,1,1,1,1,1,6),(2,2),(-1.,-0.984615384615383,-0.969230769230768,-0.953846153846152,
-0.938461538461537,-0.923076923076922,-0.907692307692306,-0.892307692307691,
-0.876923076923076,-0.86153846153846,-0.846153846153845,-0.83076923076923,
-0.815384615384614,-0.799999999999999,-0.784615384615384,-0.769230769230768,
-0.753846153846153,-0.738461538461538,-0.723076923076922,-0.707692307692307,
-0.692307692307692,-0.676923076923076,-0.661538461538461,-0.646153846153846,
-0.63076923076923,-0.615384615384615,-0.6,-0.584615384615384,-0.569230769230769,
-0.553846153846154,-0.538461538461538,-0.523076923076923,-0.507692307692308,
-0.492307692307692,-0.476923076923077,-0.461538461538462,-0.446153846153846,
-0.430769230769231,-0.415384615384615,-0.4,-0.384615384615385,-0.369230769230769,
-0.353846153846154,-0.338461538461538,-0.323076923076923,-0.307692307692308,
-0.292307692307692,-0.276923076923077,-0.261538461538462,-0.246153846153846,
-0.230769230769231,-0.215384615384615,-0.2,-0.184615384615385,-0.169230769230769,
-0.153846153846154,-0.138461538461538,-0.123076923076923,-0.107692307692308,
-0.0923076923076923,-0.0769230769230769,-0.0615384615384615,-0.0461538461538462,
-0.0307692307692308,-0.0153846153846154,0.),(-1.,1.),.UNSPECIFIED.)
GEOMETRIC_REPRESENTATION_ITEM()
RATIONAL_B_SPLINE_SURFACE(((1.,1.),(1.,1.),(1.,1.),(1.,1.),(1.,1.),(1.,
1.),(1.,1.),(1.,1.),(1.,1.),(1.,1.),(1.,1.),(1.,1.),(1.,1.),(1.,1.),(1.,
1.),(1.,1.),(1.,1.),(1.,1.),(1.,1.),(1.,1.),(1.,1.),(1.,1.),(1.,1.),(1.,
1.),(1.,1.),(1.,1.),(1.,1.),(1.,1.),(1.,1.),(1.,1.),(1.,1.),(1.,1.),(1.,
1.),(1.,1.),(1.,1.),(1.,1.),(1.,1.),(1.,1.),(1.,1.),(1.,1.),(1.,1.),(1.,
1.),(1.,1.),(1.,1.),(1.,1.),(1.,1.),(1.,1.),(1.,1.),(1.,1.),(1.,1.),(1.,
1.),(1.,1.),(1.,1.),(1.,1.),(1.,1.),(1.,1.),(1.,1.),(1.,1.),(1.,1.),(1.,
1.),(1.,1.),(1.,1.),(1.,1.),(1.,1.),(1.,1.),(1.,1.),(1.,1.),(1.,1.),(1.,
1.),(1.,1.)))
REPRESENTATION_ITEM('')
SURFACE()
);
#27=(
BOUNDED_SURFACE()
B_SPLINE_SURFACE(5,1,((#33188,#33189),(#33190,#33191),(#33192,#33193),(#33194,
#33195),(#33196,#33197),(#33198,#33199),(#33200,#33201),(#33202,#33203),
(#33204,#33205),(#33206,#33207),(#33208,#33209),(#33210,#33211),(#33212,
#33213),(#33214,#33215),(#33216,#33217),(#33218,#33219),(#33220,#33221),
(#33222,#33223),(#33224,#33225),(#33226,#33227),(#33228,#33229),(#33230,
#33231),(#33232,#33233),(#33234,#33235),(#33236,#33237),(#33238,#33239),
(#33240,#33241),(#33242,#33243),(#33244,#33245),(#33246,#33247),(#33248,
#33249),(#33250,#33251),(#33252,#33253),(#33254,#33255),(#33256,#33257),
(#33258,#33259),(#33260,#33261),(#33262,#33263),(#33264,#33265),(#33266,
#33267),(#33268,#33269),(#33270,#33271),(#33272,#33273),(#33274,#33275),
(#33276,#33277),(#33278,#33279),(#33280,#33281),(#33282,#33283),(#33284,
#33285),(#33286,#33287),(#33288,#33289),(#33290,#33291),(#33292,#33293),
(#33294,#33295),(#33296,#33297),(#33298,#33299),(#33300,#33301),(#33302,
#33303),(#33304,#33305),(#33306,#33307),(#33308,#33309),(#33310,#33311),
(#33312,#33313),(#33314,#33315),(#33316,#33317),(#33318,#33319),(#33320,
#33321),(#33322,#33323),(#33324,#33325),(#33326,#33327)),.UNSPECIFIED.,
 .F.,.F.,.F.)
B_SPLINE_SURFACE_WITH_KNOTS((6,1,1,1,1,1,1,1,1,1,1,1,1,1,1,1,1,1,1,1,1,
1,1,1,1,1,1,1,1,1,1,1,1,1,1,1,1,1,1,1,1,1,1,1,1,1,1,1,1,1,1,1,1,1,1,1,1,
1,1,1,1,1,1,1,1,6),(2,2),(-1.,-0.984615384615383,-0.969230769230768,-0.953846153846152,
-0.938461538461537,-0.923076923076922,-0.907692307692306,-0.892307692307691,
-0.876923076923076,-0.86153846153846,-0.846153846153845,-0.83076923076923,
-0.815384615384614,-0.799999999999999,-0.784615384615384,-0.769230769230768,
-0.753846153846153,-0.738461538461538,-0.723076923076922,-0.707692307692307,
-0.692307692307692,-0.676923076923076,-0.661538461538461,-0.646153846153846,
-0.63076923076923,-0.615384615384615,-0.6,-0.584615384615384,-0.569230769230769,
-0.553846153846154,-0.538461538461538,-0.523076923076923,-0.507692307692308,
-0.492307692307692,-0.476923076923077,-0.461538461538462,-0.446153846153846,
-0.430769230769231,-0.415384615384615,-0.4,-0.384615384615385,-0.369230769230769,
-0.353846153846154,-0.338461538461538,-0.323076923076923,-0.307692307692308,
-0.292307692307692,-0.276923076923077,-0.261538461538462,-0.246153846153846,
-0.230769230769231,-0.215384615384615,-0.2,-0.184615384615385,-0.169230769230769,
-0.153846153846154,-0.138461538461538,-0.123076923076923,-0.107692307692308,
-0.0923076923076923,-0.0769230769230769,-0.0615384615384615,-0.0461538461538462,
-0.0307692307692308,-0.0153846153846154,0.),(-1.,1.),.UNSPECIFIED.)
GEOMETRIC_REPRESENTATION_ITEM()
RATIONAL_B_SPLINE_SURFACE(((1.,1.),(1.,1.),(1.,1.),(1.,1.),(1.,1.),(1.,
1.),(1.,1.),(1.,1.),(1.,1.),(1.,1.),(1.,1.),(1.,1.),(1.,1.),(1.,1.),(1.,
1.),(1.,1.),(1.,1.),(1.,1.),(1.,1.),(1.,1.),(1.,1.),(1.,1.),(1.,1.),(1.,
1.),(1.,1.),(1.,1.),(1.,1.),(1.,1.),(1.,1.),(1.,1.),(1.,1.),(1.,1.),(1.,
1.),(1.,1.),(1.,1.),(1.,1.),(1.,1.),(1.,1.),(1.,1.),(1.,1.),(1.,1.),(1.,
1.),(1.,1.),(1.,1.),(1.,1.),(1.,1.),(1.,1.),(1.,1.),(1.,1.),(1.,1.),(1.,
1.),(1.,1.),(1.,1.),(1.,1.),(1.,1.),(1.,1.),(1.,1.),(1.,1.),(1.,1.),(1.,
1.),(1.,1.),(1.,1.),(1.,1.),(1.,1.),(1.,1.),(1.,1.),(1.,1.),(1.,1.),(1.,
1.),(1.,1.)))
REPRESENTATION_ITEM('')
SURFACE()
);
#28=(
BOUNDED_SURFACE()
B_SPLINE_SURFACE(5,1,((#33404,#33405),(#33406,#33407),(#33408,#33409),(#33410,
#33411),(#33412,#33413),(#33414,#33415),(#33416,#33417),(#33418,#33419),
(#33420,#33421),(#33422,#33423),(#33424,#33425),(#33426,#33427),(#33428,
#33429),(#33430,#33431),(#33432,#33433),(#33434,#33435),(#33436,#33437),
(#33438,#33439),(#33440,#33441),(#33442,#33443),(#33444,#33445),(#33446,
#33447),(#33448,#33449),(#33450,#33451),(#33452,#33453),(#33454,#33455),
(#33456,#33457),(#33458,#33459),(#33460,#33461),(#33462,#33463),(#33464,
#33465),(#33466,#33467),(#33468,#33469),(#33470,#33471),(#33472,#33473),
(#33474,#33475),(#33476,#33477),(#33478,#33479),(#33480,#33481),(#33482,
#33483),(#33484,#33485),(#33486,#33487),(#33488,#33489),(#33490,#33491),
(#33492,#33493),(#33494,#33495),(#33496,#33497),(#33498,#33499),(#33500,
#33501),(#33502,#33503),(#33504,#33505),(#33506,#33507),(#33508,#33509),
(#33510,#33511),(#33512,#33513),(#33514,#33515),(#33516,#33517),(#33518,
#33519),(#33520,#33521),(#33522,#33523),(#33524,#33525),(#33526,#33527),
(#33528,#33529),(#33530,#33531),(#33532,#33533),(#33534,#33535),(#33536,
#33537),(#33538,#33539),(#33540,#33541),(#33542,#33543)),.UNSPECIFIED.,
 .F.,.F.,.F.)
B_SPLINE_SURFACE_WITH_KNOTS((6,1,1,1,1,1,1,1,1,1,1,1,1,1,1,1,1,1,1,1,1,
1,1,1,1,1,1,1,1,1,1,1,1,1,1,1,1,1,1,1,1,1,1,1,1,1,1,1,1,1,1,1,1,1,1,1,1,
1,1,1,1,1,1,1,1,6),(2,2),(-1.,-0.984615384615383,-0.969230769230768,-0.953846153846152,
-0.938461538461537,-0.923076923076922,-0.907692307692306,-0.892307692307691,
-0.876923076923076,-0.86153846153846,-0.846153846153845,-0.83076923076923,
-0.815384615384614,-0.799999999999999,-0.784615384615384,-0.769230769230768,
-0.753846153846153,-0.738461538461538,-0.723076923076922,-0.707692307692307,
-0.692307692307692,-0.676923076923076,-0.661538461538461,-0.646153846153846,
-0.63076923076923,-0.615384615384615,-0.6,-0.584615384615384,-0.569230769230769,
-0.553846153846154,-0.538461538461538,-0.523076923076923,-0.507692307692308,
-0.492307692307692,-0.476923076923077,-0.461538461538462,-0.446153846153846,
-0.430769230769231,-0.415384615384615,-0.4,-0.384615384615385,-0.369230769230769,
-0.353846153846154,-0.338461538461538,-0.323076923076923,-0.307692307692308,
-0.292307692307692,-0.276923076923077,-0.261538461538462,-0.246153846153846,
-0.230769230769231,-0.215384615384615,-0.2,-0.184615384615385,-0.169230769230769,
-0.153846153846154,-0.138461538461538,-0.123076923076923,-0.107692307692308,
-0.0923076923076923,-0.0769230769230769,-0.0615384615384615,-0.0461538461538462,
-0.0307692307692308,-0.0153846153846154,0.),(-1.,1.),.UNSPECIFIED.)
GEOMETRIC_REPRESENTATION_ITEM()
RATIONAL_B_SPLINE_SURFACE(((1.,1.),(1.,1.),(1.,1.),(1.,1.),(1.,1.),(1.,
1.),(1.,1.),(1.,1.),(1.,1.),(1.,1.),(1.,1.),(1.,1.),(1.,1.),(1.,1.),(1.,
1.),(1.,1.),(1.,1.),(1.,1.),(1.,1.),(1.,1.),(1.,1.),(1.,1.),(1.,1.),(1.,
1.),(1.,1.),(1.,1.),(1.,1.),(1.,1.),(1.,1.),(1.,1.),(1.,1.),(1.,1.),(1.,
1.),(1.,1.),(1.,1.),(1.,1.),(1.,1.),(1.,1.),(1.,1.),(1.,1.),(1.,1.),(1.,
1.),(1.,1.),(1.,1.),(1.,1.),(1.,1.),(1.,1.),(1.,1.),(1.,1.),(1.,1.),(1.,
1.),(1.,1.),(1.,1.),(1.,1.),(1.,1.),(1.,1.),(1.,1.),(1.,1.),(1.,1.),(1.,
1.),(1.,1.),(1.,1.),(1.,1.),(1.,1.),(1.,1.),(1.,1.),(1.,1.),(1.,1.),(1.,
1.),(1.,1.)))
REPRESENTATION_ITEM('')
SURFACE()
);
#29=(
BOUNDED_SURFACE()
B_SPLINE_SURFACE(5,1,((#33620,#33621),(#33622,#33623),(#33624,#33625),(#33626,
#33627),(#33628,#33629),(#33630,#33631),(#33632,#33633),(#33634,#33635),
(#33636,#33637),(#33638,#33639),(#33640,#33641),(#33642,#33643),(#33644,
#33645),(#33646,#33647),(#33648,#33649),(#33650,#33651),(#33652,#33653),
(#33654,#33655),(#33656,#33657),(#33658,#33659),(#33660,#33661),(#33662,
#33663),(#33664,#33665),(#33666,#33667),(#33668,#33669),(#33670,#33671),
(#33672,#33673),(#33674,#33675),(#33676,#33677),(#33678,#33679),(#33680,
#33681),(#33682,#33683),(#33684,#33685),(#33686,#33687),(#33688,#33689),
(#33690,#33691),(#33692,#33693),(#33694,#33695),(#33696,#33697),(#33698,
#33699),(#33700,#33701),(#33702,#33703),(#33704,#33705),(#33706,#33707),
(#33708,#33709),(#33710,#33711),(#33712,#33713),(#33714,#33715),(#33716,
#33717),(#33718,#33719),(#33720,#33721),(#33722,#33723),(#33724,#33725),
(#33726,#33727),(#33728,#33729),(#33730,#33731),(#33732,#33733),(#33734,
#33735),(#33736,#33737),(#33738,#33739),(#33740,#33741),(#33742,#33743),
(#33744,#33745),(#33746,#33747),(#33748,#33749),(#33750,#33751),(#33752,
#33753),(#33754,#33755),(#33756,#33757),(#33758,#33759)),.UNSPECIFIED.,
 .F.,.F.,.F.)
B_SPLINE_SURFACE_WITH_KNOTS((6,1,1,1,1,1,1,1,1,1,1,1,1,1,1,1,1,1,1,1,1,
1,1,1,1,1,1,1,1,1,1,1,1,1,1,1,1,1,1,1,1,1,1,1,1,1,1,1,1,1,1,1,1,1,1,1,1,
1,1,1,1,1,1,1,1,6),(2,2),(-1.,-0.984615384615383,-0.969230769230768,-0.953846153846152,
-0.938461538461537,-0.923076923076922,-0.907692307692306,-0.892307692307691,
-0.876923076923076,-0.86153846153846,-0.846153846153845,-0.83076923076923,
-0.815384615384614,-0.799999999999999,-0.784615384615384,-0.769230769230768,
-0.753846153846153,-0.738461538461538,-0.723076923076922,-0.707692307692307,
-0.692307692307692,-0.676923076923076,-0.661538461538461,-0.646153846153846,
-0.63076923076923,-0.615384615384615,-0.6,-0.584615384615384,-0.569230769230769,
-0.553846153846154,-0.538461538461538,-0.523076923076923,-0.507692307692308,
-0.492307692307692,-0.476923076923077,-0.461538461538462,-0.446153846153846,
-0.430769230769231,-0.415384615384615,-0.4,-0.384615384615385,-0.369230769230769,
-0.353846153846154,-0.338461538461538,-0.323076923076923,-0.307692307692308,
-0.292307692307692,-0.276923076923077,-0.261538461538462,-0.246153846153846,
-0.230769230769231,-0.215384615384615,-0.2,-0.184615384615385,-0.169230769230769,
-0.153846153846154,-0.138461538461538,-0.123076923076923,-0.107692307692308,
-0.0923076923076923,-0.0769230769230769,-0.0615384615384615,-0.0461538461538462,
-0.0307692307692308,-0.0153846153846154,0.),(-1.,1.),.UNSPECIFIED.)
GEOMETRIC_REPRESENTATION_ITEM()
RATIONAL_B_SPLINE_SURFACE(((1.,1.),(1.,1.),(1.,1.),(1.,1.),(1.,1.),(1.,
1.),(1.,1.),(1.,1.),(1.,1.),(1.,1.),(1.,1.),(1.,1.),(1.,1.),(1.,1.),(1.,
1.),(1.,1.),(1.,1.),(1.,1.),(1.,1.),(1.,1.),(1.,1.),(1.,1.),(1.,1.),(1.,
1.),(1.,1.),(1.,1.),(1.,1.),(1.,1.),(1.,1.),(1.,1.),(1.,1.),(1.,1.),(1.,
1.),(1.,1.),(1.,1.),(1.,1.),(1.,1.),(1.,1.),(1.,1.),(1.,1.),(1.,1.),(1.,
1.),(1.,1.),(1.,1.),(1.,1.),(1.,1.),(1.,1.),(1.,1.),(1.,1.),(1.,1.),(1.,
1.),(1.,1.),(1.,1.),(1.,1.),(1.,1.),(1.,1.),(1.,1.),(1.,1.),(1.,1.),(1.,
1.),(1.,1.),(1.,1.),(1.,1.),(1.,1.),(1.,1.),(1.,1.),(1.,1.),(1.,1.),(1.,
1.),(1.,1.)))
REPRESENTATION_ITEM('')
SURFACE()
);
#30=(
BOUNDED_SURFACE()
B_SPLINE_SURFACE(5,1,((#33836,#33837),(#33838,#33839),(#33840,#33841),(#33842,
#33843),(#33844,#33845),(#33846,#33847),(#33848,#33849),(#33850,#33851),
(#33852,#33853),(#33854,#33855),(#33856,#33857),(#33858,#33859),(#33860,
#33861),(#33862,#33863),(#33864,#33865),(#33866,#33867),(#33868,#33869),
(#33870,#33871),(#33872,#33873),(#33874,#33875),(#33876,#33877),(#33878,
#33879),(#33880,#33881),(#33882,#33883),(#33884,#33885),(#33886,#33887),
(#33888,#33889),(#33890,#33891),(#33892,#33893),(#33894,#33895),(#33896,
#33897),(#33898,#33899),(#33900,#33901),(#33902,#33903),(#33904,#33905),
(#33906,#33907),(#33908,#33909),(#33910,#33911),(#33912,#33913),(#33914,
#33915),(#33916,#33917),(#33918,#33919),(#33920,#33921),(#33922,#33923),
(#33924,#33925),(#33926,#33927),(#33928,#33929),(#33930,#33931),(#33932,
#33933),(#33934,#33935),(#33936,#33937),(#33938,#33939),(#33940,#33941),
(#33942,#33943),(#33944,#33945),(#33946,#33947),(#33948,#33949),(#33950,
#33951),(#33952,#33953),(#33954,#33955),(#33956,#33957),(#33958,#33959),
(#33960,#33961),(#33962,#33963),(#33964,#33965),(#33966,#33967),(#33968,
#33969),(#33970,#33971),(#33972,#33973),(#33974,#33975)),.UNSPECIFIED.,
 .F.,.F.,.F.)
B_SPLINE_SURFACE_WITH_KNOTS((6,1,1,1,1,1,1,1,1,1,1,1,1,1,1,1,1,1,1,1,1,
1,1,1,1,1,1,1,1,1,1,1,1,1,1,1,1,1,1,1,1,1,1,1,1,1,1,1,1,1,1,1,1,1,1,1,1,
1,1,1,1,1,1,1,1,6),(2,2),(-1.,-0.984615384615383,-0.969230769230768,-0.953846153846152,
-0.938461538461537,-0.923076923076922,-0.907692307692306,-0.892307692307691,
-0.876923076923076,-0.86153846153846,-0.846153846153845,-0.83076923076923,
-0.815384615384614,-0.799999999999999,-0.784615384615384,-0.769230769230768,
-0.753846153846153,-0.738461538461538,-0.723076923076922,-0.707692307692307,
-0.692307692307692,-0.676923076923076,-0.661538461538461,-0.646153846153846,
-0.63076923076923,-0.615384615384615,-0.6,-0.584615384615384,-0.569230769230769,
-0.553846153846154,-0.538461538461538,-0.523076923076923,-0.507692307692308,
-0.492307692307692,-0.476923076923077,-0.461538461538462,-0.446153846153846,
-0.430769230769231,-0.415384615384615,-0.4,-0.384615384615385,-0.369230769230769,
-0.353846153846154,-0.338461538461538,-0.323076923076923,-0.307692307692308,
-0.292307692307692,-0.276923076923077,-0.261538461538462,-0.246153846153846,
-0.230769230769231,-0.215384615384615,-0.2,-0.184615384615385,-0.169230769230769,
-0.153846153846154,-0.138461538461538,-0.123076923076923,-0.107692307692308,
-0.0923076923076923,-0.0769230769230769,-0.0615384615384615,-0.0461538461538462,
-0.0307692307692308,-0.0153846153846154,0.),(-1.,1.),.UNSPECIFIED.)
GEOMETRIC_REPRESENTATION_ITEM()
RATIONAL_B_SPLINE_SURFACE(((1.,1.),(1.,1.),(1.,1.),(1.,1.),(1.,1.),(1.,
1.),(1.,1.),(1.,1.),(1.,1.),(1.,1.),(1.,1.),(1.,1.),(1.,1.),(1.,1.),(1.,
1.),(1.,1.),(1.,1.),(1.,1.),(1.,1.),(1.,1.),(1.,1.),(1.,1.),(1.,1.),(1.,
1.),(1.,1.),(1.,1.),(1.,1.),(1.,1.),(1.,1.),(1.,1.),(1.,1.),(1.,1.),(1.,
1.),(1.,1.),(1.,1.),(1.,1.),(1.,1.),(1.,1.),(1.,1.),(1.,1.),(1.,1.),(1.,
1.),(1.,1.),(1.,1.),(1.,1.),(1.,1.),(1.,1.),(1.,1.),(1.,1.),(1.,1.),(1.,
1.),(1.,1.),(1.,1.),(1.,1.),(1.,1.),(1.,1.),(1.,1.),(1.,1.),(1.,1.),(1.,
1.),(1.,1.),(1.,1.),(1.,1.),(1.,1.),(1.,1.),(1.,1.),(1.,1.),(1.,1.),(1.,
1.),(1.,1.)))
REPRESENTATION_ITEM('')
SURFACE()
);
#31=(
BOUNDED_SURFACE()
B_SPLINE_SURFACE(5,1,((#34052,#34053),(#34054,#34055),(#34056,#34057),(#34058,
#34059),(#34060,#34061),(#34062,#34063),(#34064,#34065),(#34066,#34067),
(#34068,#34069),(#34070,#34071),(#34072,#34073),(#34074,#34075),(#34076,
#34077),(#34078,#34079),(#34080,#34081),(#34082,#34083),(#34084,#34085),
(#34086,#34087),(#34088,#34089),(#34090,#34091),(#34092,#34093),(#34094,
#34095),(#34096,#34097),(#34098,#34099),(#34100,#34101),(#34102,#34103),
(#34104,#34105),(#34106,#34107),(#34108,#34109),(#34110,#34111),(#34112,
#34113),(#34114,#34115),(#34116,#34117),(#34118,#34119),(#34120,#34121),
(#34122,#34123),(#34124,#34125),(#34126,#34127),(#34128,#34129),(#34130,
#34131),(#34132,#34133),(#34134,#34135),(#34136,#34137),(#34138,#34139),
(#34140,#34141),(#34142,#34143),(#34144,#34145),(#34146,#34147),(#34148,
#34149),(#34150,#34151),(#34152,#34153),(#34154,#34155),(#34156,#34157),
(#34158,#34159),(#34160,#34161),(#34162,#34163),(#34164,#34165),(#34166,
#34167),(#34168,#34169),(#34170,#34171),(#34172,#34173),(#34174,#34175),
(#34176,#34177),(#34178,#34179),(#34180,#34181),(#34182,#34183),(#34184,
#34185),(#34186,#34187),(#34188,#34189),(#34190,#34191)),.UNSPECIFIED.,
 .F.,.F.,.F.)
B_SPLINE_SURFACE_WITH_KNOTS((6,1,1,1,1,1,1,1,1,1,1,1,1,1,1,1,1,1,1,1,1,
1,1,1,1,1,1,1,1,1,1,1,1,1,1,1,1,1,1,1,1,1,1,1,1,1,1,1,1,1,1,1,1,1,1,1,1,
1,1,1,1,1,1,1,1,6),(2,2),(-1.,-0.984615384615383,-0.969230769230768,-0.953846153846152,
-0.938461538461537,-0.923076923076922,-0.907692307692306,-0.892307692307691,
-0.876923076923076,-0.86153846153846,-0.846153846153845,-0.83076923076923,
-0.815384615384614,-0.799999999999999,-0.784615384615384,-0.769230769230768,
-0.753846153846153,-0.738461538461538,-0.723076923076922,-0.707692307692307,
-0.692307692307692,-0.676923076923076,-0.661538461538461,-0.646153846153846,
-0.63076923076923,-0.615384615384615,-0.6,-0.584615384615384,-0.569230769230769,
-0.553846153846154,-0.538461538461538,-0.523076923076923,-0.507692307692308,
-0.492307692307692,-0.476923076923077,-0.461538461538462,-0.446153846153846,
-0.430769230769231,-0.415384615384615,-0.4,-0.384615384615385,-0.369230769230769,
-0.353846153846154,-0.338461538461538,-0.323076923076923,-0.307692307692308,
-0.292307692307692,-0.276923076923077,-0.261538461538462,-0.246153846153846,
-0.230769230769231,-0.215384615384615,-0.2,-0.184615384615385,-0.169230769230769,
-0.153846153846154,-0.138461538461538,-0.123076923076923,-0.107692307692308,
-0.0923076923076923,-0.0769230769230769,-0.0615384615384615,-0.0461538461538462,
-0.0307692307692308,-0.0153846153846154,0.),(-1.,1.),.UNSPECIFIED.)
GEOMETRIC_REPRESENTATION_ITEM()
RATIONAL_B_SPLINE_SURFACE(((1.,1.),(1.,1.),(1.,1.),(1.,1.),(1.,1.),(1.,
1.),(1.,1.),(1.,1.),(1.,1.),(1.,1.),(1.,1.),(1.,1.),(1.,1.),(1.,1.),(1.,
1.),(1.,1.),(1.,1.),(1.,1.),(1.,1.),(1.,1.),(1.,1.),(1.,1.),(1.,1.),(1.,
1.),(1.,1.),(1.,1.),(1.,1.),(1.,1.),(1.,1.),(1.,1.),(1.,1.),(1.,1.),(1.,
1.),(1.,1.),(1.,1.),(1.,1.),(1.,1.),(1.,1.),(1.,1.),(1.,1.),(1.,1.),(1.,
1.),(1.,1.),(1.,1.),(1.,1.),(1.,1.),(1.,1.),(1.,1.),(1.,1.),(1.,1.),(1.,
1.),(1.,1.),(1.,1.),(1.,1.),(1.,1.),(1.,1.),(1.,1.),(1.,1.),(1.,1.),(1.,
1.),(1.,1.),(1.,1.),(1.,1.),(1.,1.),(1.,1.),(1.,1.),(1.,1.),(1.,1.),(1.,
1.),(1.,1.)))
REPRESENTATION_ITEM('')
SURFACE()
);
#32=(
BOUNDED_SURFACE()
B_SPLINE_SURFACE(5,1,((#34268,#34269),(#34270,#34271),(#34272,#34273),(#34274,
#34275),(#34276,#34277),(#34278,#34279),(#34280,#34281),(#34282,#34283),
(#34284,#34285),(#34286,#34287),(#34288,#34289),(#34290,#34291),(#34292,
#34293),(#34294,#34295),(#34296,#34297),(#34298,#34299),(#34300,#34301),
(#34302,#34303),(#34304,#34305),(#34306,#34307),(#34308,#34309),(#34310,
#34311),(#34312,#34313),(#34314,#34315),(#34316,#34317),(#34318,#34319),
(#34320,#34321),(#34322,#34323),(#34324,#34325),(#34326,#34327),(#34328,
#34329),(#34330,#34331),(#34332,#34333),(#34334,#34335),(#34336,#34337),
(#34338,#34339),(#34340,#34341),(#34342,#34343),(#34344,#34345),(#34346,
#34347),(#34348,#34349),(#34350,#34351),(#34352,#34353),(#34354,#34355),
(#34356,#34357),(#34358,#34359),(#34360,#34361),(#34362,#34363),(#34364,
#34365),(#34366,#34367),(#34368,#34369),(#34370,#34371),(#34372,#34373),
(#34374,#34375),(#34376,#34377),(#34378,#34379),(#34380,#34381),(#34382,
#34383),(#34384,#34385),(#34386,#34387),(#34388,#34389),(#34390,#34391),
(#34392,#34393),(#34394,#34395),(#34396,#34397),(#34398,#34399),(#34400,
#34401),(#34402,#34403),(#34404,#34405),(#34406,#34407)),.UNSPECIFIED.,
 .F.,.F.,.F.)
B_SPLINE_SURFACE_WITH_KNOTS((6,1,1,1,1,1,1,1,1,1,1,1,1,1,1,1,1,1,1,1,1,
1,1,1,1,1,1,1,1,1,1,1,1,1,1,1,1,1,1,1,1,1,1,1,1,1,1,1,1,1,1,1,1,1,1,1,1,
1,1,1,1,1,1,1,1,6),(2,2),(-1.,-0.984615384615383,-0.969230769230768,-0.953846153846152,
-0.938461538461537,-0.923076923076922,-0.907692307692306,-0.892307692307691,
-0.876923076923076,-0.86153846153846,-0.846153846153845,-0.83076923076923,
-0.815384615384614,-0.799999999999999,-0.784615384615384,-0.769230769230768,
-0.753846153846153,-0.738461538461538,-0.723076923076922,-0.707692307692307,
-0.692307692307692,-0.676923076923076,-0.661538461538461,-0.646153846153846,
-0.63076923076923,-0.615384615384615,-0.6,-0.584615384615384,-0.569230769230769,
-0.553846153846154,-0.538461538461538,-0.523076923076923,-0.507692307692308,
-0.492307692307692,-0.476923076923077,-0.461538461538462,-0.446153846153846,
-0.430769230769231,-0.415384615384615,-0.4,-0.384615384615385,-0.369230769230769,
-0.353846153846154,-0.338461538461538,-0.323076923076923,-0.307692307692308,
-0.292307692307692,-0.276923076923077,-0.261538461538462,-0.246153846153846,
-0.230769230769231,-0.215384615384615,-0.2,-0.184615384615385,-0.169230769230769,
-0.153846153846154,-0.138461538461538,-0.123076923076923,-0.107692307692308,
-0.0923076923076923,-0.0769230769230769,-0.0615384615384615,-0.0461538461538462,
-0.0307692307692308,-0.0153846153846154,0.),(-1.,1.),.UNSPECIFIED.)
GEOMETRIC_REPRESENTATION_ITEM()
RATIONAL_B_SPLINE_SURFACE(((1.,1.),(1.,1.),(1.,1.),(1.,1.),(1.,1.),(1.,
1.),(1.,1.),(1.,1.),(1.,1.),(1.,1.),(1.,1.),(1.,1.),(1.,1.),(1.,1.),(1.,
1.),(1.,1.),(1.,1.),(1.,1.),(1.,1.),(1.,1.),(1.,1.),(1.,1.),(1.,1.),(1.,
1.),(1.,1.),(1.,1.),(1.,1.),(1.,1.),(1.,1.),(1.,1.),(1.,1.),(1.,1.),(1.,
1.),(1.,1.),(1.,1.),(1.,1.),(1.,1.),(1.,1.),(1.,1.),(1.,1.),(1.,1.),(1.,
1.),(1.,1.),(1.,1.),(1.,1.),(1.,1.),(1.,1.),(1.,1.),(1.,1.),(1.,1.),(1.,
1.),(1.,1.),(1.,1.),(1.,1.),(1.,1.),(1.,1.),(1.,1.),(1.,1.),(1.,1.),(1.,
1.),(1.,1.),(1.,1.),(1.,1.),(1.,1.),(1.,1.),(1.,1.),(1.,1.),(1.,1.),(1.,
1.),(1.,1.)))
REPRESENTATION_ITEM('')
SURFACE()
);
#33=(
BOUNDED_SURFACE()
B_SPLINE_SURFACE(5,1,((#34484,#34485),(#34486,#34487),(#34488,#34489),(#34490,
#34491),(#34492,#34493),(#34494,#34495),(#34496,#34497),(#34498,#34499),
(#34500,#34501),(#34502,#34503),(#34504,#34505),(#34506,#34507),(#34508,
#34509),(#34510,#34511),(#34512,#34513),(#34514,#34515),(#34516,#34517),
(#34518,#34519),(#34520,#34521),(#34522,#34523),(#34524,#34525),(#34526,
#34527),(#34528,#34529),(#34530,#34531),(#34532,#34533),(#34534,#34535),
(#34536,#34537),(#34538,#34539),(#34540,#34541),(#34542,#34543),(#34544,
#34545),(#34546,#34547),(#34548,#34549),(#34550,#34551),(#34552,#34553),
(#34554,#34555),(#34556,#34557),(#34558,#34559),(#34560,#34561),(#34562,
#34563),(#34564,#34565),(#34566,#34567),(#34568,#34569),(#34570,#34571),
(#34572,#34573),(#34574,#34575),(#34576,#34577),(#34578,#34579),(#34580,
#34581),(#34582,#34583),(#34584,#34585),(#34586,#34587),(#34588,#34589),
(#34590,#34591),(#34592,#34593),(#34594,#34595),(#34596,#34597),(#34598,
#34599),(#34600,#34601),(#34602,#34603),(#34604,#34605),(#34606,#34607),
(#34608,#34609),(#34610,#34611),(#34612,#34613),(#34614,#34615),(#34616,
#34617),(#34618,#34619),(#34620,#34621),(#34622,#34623)),.UNSPECIFIED.,
 .F.,.F.,.F.)
B_SPLINE_SURFACE_WITH_KNOTS((6,1,1,1,1,1,1,1,1,1,1,1,1,1,1,1,1,1,1,1,1,
1,1,1,1,1,1,1,1,1,1,1,1,1,1,1,1,1,1,1,1,1,1,1,1,1,1,1,1,1,1,1,1,1,1,1,1,
1,1,1,1,1,1,1,1,6),(2,2),(-1.,-0.984615384615383,-0.969230769230768,-0.953846153846152,
-0.938461538461537,-0.923076923076922,-0.907692307692306,-0.892307692307691,
-0.876923076923076,-0.86153846153846,-0.846153846153845,-0.83076923076923,
-0.815384615384614,-0.799999999999999,-0.784615384615384,-0.769230769230768,
-0.753846153846153,-0.738461538461538,-0.723076923076922,-0.707692307692307,
-0.692307692307692,-0.676923076923076,-0.661538461538461,-0.646153846153846,
-0.63076923076923,-0.615384615384615,-0.6,-0.584615384615384,-0.569230769230769,
-0.553846153846154,-0.538461538461538,-0.523076923076923,-0.507692307692308,
-0.492307692307692,-0.476923076923077,-0.461538461538462,-0.446153846153846,
-0.430769230769231,-0.415384615384615,-0.4,-0.384615384615385,-0.369230769230769,
-0.353846153846154,-0.338461538461538,-0.323076923076923,-0.307692307692308,
-0.292307692307692,-0.276923076923077,-0.261538461538462,-0.246153846153846,
-0.230769230769231,-0.215384615384615,-0.2,-0.184615384615385,-0.169230769230769,
-0.153846153846154,-0.138461538461538,-0.123076923076923,-0.107692307692308,
-0.0923076923076923,-0.0769230769230769,-0.0615384615384615,-0.0461538461538462,
-0.0307692307692308,-0.0153846153846154,0.),(-1.,1.),.UNSPECIFIED.)
GEOMETRIC_REPRESENTATION_ITEM()
RATIONAL_B_SPLINE_SURFACE(((1.,1.),(1.,1.),(1.,1.),(1.,1.),(1.,1.),(1.,
1.),(1.,1.),(1.,1.),(1.,1.),(1.,1.),(1.,1.),(1.,1.),(1.,1.),(1.,1.),(1.,
1.),(1.,1.),(1.,1.),(1.,1.),(1.,1.),(1.,1.),(1.,1.),(1.,1.),(1.,1.),(1.,
1.),(1.,1.),(1.,1.),(1.,1.),(1.,1.),(1.,1.),(1.,1.),(1.,1.),(1.,1.),(1.,
1.),(1.,1.),(1.,1.),(1.,1.),(1.,1.),(1.,1.),(1.,1.),(1.,1.),(1.,1.),(1.,
1.),(1.,1.),(1.,1.),(1.,1.),(1.,1.),(1.,1.),(1.,1.),(1.,1.),(1.,1.),(1.,
1.),(1.,1.),(1.,1.),(1.,1.),(1.,1.),(1.,1.),(1.,1.),(1.,1.),(1.,1.),(1.,
1.),(1.,1.),(1.,1.),(1.,1.),(1.,1.),(1.,1.),(1.,1.),(1.,1.),(1.,1.),(1.,
1.),(1.,1.)))
REPRESENTATION_ITEM('')
SURFACE()
);
#34=(
BOUNDED_SURFACE()
B_SPLINE_SURFACE(5,1,((#34700,#34701),(#34702,#34703),(#34704,#34705),(#34706,
#34707),(#34708,#34709),(#34710,#34711),(#34712,#34713),(#34714,#34715),
(#34716,#34717),(#34718,#34719),(#34720,#34721),(#34722,#34723),(#34724,
#34725),(#34726,#34727),(#34728,#34729),(#34730,#34731),(#34732,#34733),
(#34734,#34735),(#34736,#34737),(#34738,#34739),(#34740,#34741),(#34742,
#34743),(#34744,#34745),(#34746,#34747),(#34748,#34749),(#34750,#34751),
(#34752,#34753),(#34754,#34755),(#34756,#34757),(#34758,#34759),(#34760,
#34761),(#34762,#34763),(#34764,#34765),(#34766,#34767),(#34768,#34769),
(#34770,#34771),(#34772,#34773),(#34774,#34775),(#34776,#34777),(#34778,
#34779),(#34780,#34781),(#34782,#34783),(#34784,#34785),(#34786,#34787),
(#34788,#34789),(#34790,#34791),(#34792,#34793),(#34794,#34795),(#34796,
#34797),(#34798,#34799),(#34800,#34801),(#34802,#34803),(#34804,#34805),
(#34806,#34807),(#34808,#34809),(#34810,#34811),(#34812,#34813),(#34814,
#34815),(#34816,#34817),(#34818,#34819),(#34820,#34821),(#34822,#34823),
(#34824,#34825),(#34826,#34827),(#34828,#34829),(#34830,#34831),(#34832,
#34833),(#34834,#34835),(#34836,#34837),(#34838,#34839)),.UNSPECIFIED.,
 .F.,.F.,.F.)
B_SPLINE_SURFACE_WITH_KNOTS((6,1,1,1,1,1,1,1,1,1,1,1,1,1,1,1,1,1,1,1,1,
1,1,1,1,1,1,1,1,1,1,1,1,1,1,1,1,1,1,1,1,1,1,1,1,1,1,1,1,1,1,1,1,1,1,1,1,
1,1,1,1,1,1,1,1,6),(2,2),(-1.,-0.984615384615383,-0.969230769230768,-0.953846153846152,
-0.938461538461537,-0.923076923076922,-0.907692307692306,-0.892307692307691,
-0.876923076923076,-0.86153846153846,-0.846153846153845,-0.83076923076923,
-0.815384615384614,-0.799999999999999,-0.784615384615384,-0.769230769230768,
-0.753846153846153,-0.738461538461538,-0.723076923076922,-0.707692307692307,
-0.692307692307692,-0.676923076923076,-0.661538461538461,-0.646153846153846,
-0.63076923076923,-0.615384615384615,-0.6,-0.584615384615384,-0.569230769230769,
-0.553846153846154,-0.538461538461538,-0.523076923076923,-0.507692307692308,
-0.492307692307692,-0.476923076923077,-0.461538461538462,-0.446153846153846,
-0.430769230769231,-0.415384615384615,-0.4,-0.384615384615385,-0.369230769230769,
-0.353846153846154,-0.338461538461538,-0.323076923076923,-0.307692307692308,
-0.292307692307692,-0.276923076923077,-0.261538461538462,-0.246153846153846,
-0.230769230769231,-0.215384615384615,-0.2,-0.184615384615385,-0.169230769230769,
-0.153846153846154,-0.138461538461538,-0.123076923076923,-0.107692307692308,
-0.0923076923076923,-0.0769230769230769,-0.0615384615384615,-0.0461538461538462,
-0.0307692307692308,-0.0153846153846154,0.),(-1.,1.),.UNSPECIFIED.)
GEOMETRIC_REPRESENTATION_ITEM()
RATIONAL_B_SPLINE_SURFACE(((1.,1.),(1.,1.),(1.,1.),(1.,1.),(1.,1.),(1.,
1.),(1.,1.),(1.,1.),(1.,1.),(1.,1.),(1.,1.),(1.,1.),(1.,1.),(1.,1.),(1.,
1.),(1.,1.),(1.,1.),(1.,1.),(1.,1.),(1.,1.),(1.,1.),(1.,1.),(1.,1.),(1.,
1.),(1.,1.),(1.,1.),(1.,1.),(1.,1.),(1.,1.),(1.,1.),(1.,1.),(1.,1.),(1.,
1.),(1.,1.),(1.,1.),(1.,1.),(1.,1.),(1.,1.),(1.,1.),(1.,1.),(1.,1.),(1.,
1.),(1.,1.),(1.,1.),(1.,1.),(1.,1.),(1.,1.),(1.,1.),(1.,1.),(1.,1.),(1.,
1.),(1.,1.),(1.,1.),(1.,1.),(1.,1.),(1.,1.),(1.,1.),(1.,1.),(1.,1.),(1.,
1.),(1.,1.),(1.,1.),(1.,1.),(1.,1.),(1.,1.),(1.,1.),(1.,1.),(1.,1.),(1.,
1.),(1.,1.)))
REPRESENTATION_ITEM('')
SURFACE()
);
#35=(
BOUNDED_SURFACE()
B_SPLINE_SURFACE(5,1,((#34916,#34917),(#34918,#34919),(#34920,#34921),(#34922,
#34923),(#34924,#34925),(#34926,#34927),(#34928,#34929),(#34930,#34931),
(#34932,#34933),(#34934,#34935),(#34936,#34937),(#34938,#34939),(#34940,
#34941),(#34942,#34943),(#34944,#34945),(#34946,#34947),(#34948,#34949),
(#34950,#34951),(#34952,#34953),(#34954,#34955),(#34956,#34957),(#34958,
#34959),(#34960,#34961),(#34962,#34963),(#34964,#34965),(#34966,#34967),
(#34968,#34969),(#34970,#34971),(#34972,#34973),(#34974,#34975),(#34976,
#34977),(#34978,#34979),(#34980,#34981),(#34982,#34983),(#34984,#34985),
(#34986,#34987),(#34988,#34989),(#34990,#34991),(#34992,#34993),(#34994,
#34995),(#34996,#34997),(#34998,#34999),(#35000,#35001),(#35002,#35003),
(#35004,#35005),(#35006,#35007),(#35008,#35009),(#35010,#35011),(#35012,
#35013),(#35014,#35015),(#35016,#35017),(#35018,#35019),(#35020,#35021),
(#35022,#35023),(#35024,#35025),(#35026,#35027),(#35028,#35029),(#35030,
#35031),(#35032,#35033),(#35034,#35035),(#35036,#35037),(#35038,#35039),
(#35040,#35041),(#35042,#35043),(#35044,#35045),(#35046,#35047),(#35048,
#35049),(#35050,#35051),(#35052,#35053),(#35054,#35055)),.UNSPECIFIED.,
 .F.,.F.,.F.)
B_SPLINE_SURFACE_WITH_KNOTS((6,1,1,1,1,1,1,1,1,1,1,1,1,1,1,1,1,1,1,1,1,
1,1,1,1,1,1,1,1,1,1,1,1,1,1,1,1,1,1,1,1,1,1,1,1,1,1,1,1,1,1,1,1,1,1,1,1,
1,1,1,1,1,1,1,1,6),(2,2),(-1.,-0.984615384615383,-0.969230769230768,-0.953846153846152,
-0.938461538461537,-0.923076923076922,-0.907692307692306,-0.892307692307691,
-0.876923076923076,-0.86153846153846,-0.846153846153845,-0.83076923076923,
-0.815384615384614,-0.799999999999999,-0.784615384615384,-0.769230769230768,
-0.753846153846153,-0.738461538461538,-0.723076923076922,-0.707692307692307,
-0.692307692307692,-0.676923076923076,-0.661538461538461,-0.646153846153846,
-0.63076923076923,-0.615384615384615,-0.6,-0.584615384615384,-0.569230769230769,
-0.553846153846154,-0.538461538461538,-0.523076923076923,-0.507692307692308,
-0.492307692307692,-0.476923076923077,-0.461538461538462,-0.446153846153846,
-0.430769230769231,-0.415384615384615,-0.4,-0.384615384615385,-0.369230769230769,
-0.353846153846154,-0.338461538461538,-0.323076923076923,-0.307692307692308,
-0.292307692307692,-0.276923076923077,-0.261538461538462,-0.246153846153846,
-0.230769230769231,-0.215384615384615,-0.2,-0.184615384615385,-0.169230769230769,
-0.153846153846154,-0.138461538461538,-0.123076923076923,-0.107692307692308,
-0.0923076923076923,-0.0769230769230769,-0.0615384615384615,-0.0461538461538462,
-0.0307692307692308,-0.0153846153846154,0.),(-1.,1.),.UNSPECIFIED.)
GEOMETRIC_REPRESENTATION_ITEM()
RATIONAL_B_SPLINE_SURFACE(((1.,1.),(1.,1.),(1.,1.),(1.,1.),(1.,1.),(1.,
1.),(1.,1.),(1.,1.),(1.,1.),(1.,1.),(1.,1.),(1.,1.),(1.,1.),(1.,1.),(1.,
1.),(1.,1.),(1.,1.),(1.,1.),(1.,1.),(1.,1.),(1.,1.),(1.,1.),(1.,1.),(1.,
1.),(1.,1.),(1.,1.),(1.,1.),(1.,1.),(1.,1.),(1.,1.),(1.,1.),(1.,1.),(1.,
1.),(1.,1.),(1.,1.),(1.,1.),(1.,1.),(1.,1.),(1.,1.),(1.,1.),(1.,1.),(1.,
1.),(1.,1.),(1.,1.),(1.,1.),(1.,1.),(1.,1.),(1.,1.),(1.,1.),(1.,1.),(1.,
1.),(1.,1.),(1.,1.),(1.,1.),(1.,1.),(1.,1.),(1.,1.),(1.,1.),(1.,1.),(1.,
1.),(1.,1.),(1.,1.),(1.,1.),(1.,1.),(1.,1.),(1.,1.),(1.,1.),(1.,1.),(1.,
1.),(1.,1.)))
REPRESENTATION_ITEM('')
SURFACE()
);
#36=(
BOUNDED_SURFACE()
B_SPLINE_SURFACE(5,1,((#35132,#35133),(#35134,#35135),(#35136,#35137),(#35138,
#35139),(#35140,#35141),(#35142,#35143),(#35144,#35145),(#35146,#35147),
(#35148,#35149),(#35150,#35151),(#35152,#35153),(#35154,#35155),(#35156,
#35157),(#35158,#35159),(#35160,#35161),(#35162,#35163),(#35164,#35165),
(#35166,#35167),(#35168,#35169),(#35170,#35171),(#35172,#35173),(#35174,
#35175),(#35176,#35177),(#35178,#35179),(#35180,#35181),(#35182,#35183),
(#35184,#35185),(#35186,#35187),(#35188,#35189),(#35190,#35191),(#35192,
#35193),(#35194,#35195),(#35196,#35197),(#35198,#35199),(#35200,#35201),
(#35202,#35203),(#35204,#35205),(#35206,#35207),(#35208,#35209),(#35210,
#35211),(#35212,#35213),(#35214,#35215),(#35216,#35217),(#35218,#35219),
(#35220,#35221),(#35222,#35223),(#35224,#35225),(#35226,#35227),(#35228,
#35229),(#35230,#35231),(#35232,#35233),(#35234,#35235),(#35236,#35237),
(#35238,#35239),(#35240,#35241),(#35242,#35243),(#35244,#35245),(#35246,
#35247),(#35248,#35249),(#35250,#35251),(#35252,#35253),(#35254,#35255),
(#35256,#35257),(#35258,#35259),(#35260,#35261),(#35262,#35263),(#35264,
#35265),(#35266,#35267),(#35268,#35269),(#35270,#35271)),.UNSPECIFIED.,
 .F.,.F.,.F.)
B_SPLINE_SURFACE_WITH_KNOTS((6,1,1,1,1,1,1,1,1,1,1,1,1,1,1,1,1,1,1,1,1,
1,1,1,1,1,1,1,1,1,1,1,1,1,1,1,1,1,1,1,1,1,1,1,1,1,1,1,1,1,1,1,1,1,1,1,1,
1,1,1,1,1,1,1,1,6),(2,2),(-1.,-0.984615384615383,-0.969230769230768,-0.953846153846152,
-0.938461538461537,-0.923076923076922,-0.907692307692306,-0.892307692307691,
-0.876923076923076,-0.86153846153846,-0.846153846153845,-0.83076923076923,
-0.815384615384614,-0.799999999999999,-0.784615384615384,-0.769230769230768,
-0.753846153846153,-0.738461538461538,-0.723076923076922,-0.707692307692307,
-0.692307692307692,-0.676923076923076,-0.661538461538461,-0.646153846153846,
-0.63076923076923,-0.615384615384615,-0.6,-0.584615384615384,-0.569230769230769,
-0.553846153846154,-0.538461538461538,-0.523076923076923,-0.507692307692308,
-0.492307692307692,-0.476923076923077,-0.461538461538462,-0.446153846153846,
-0.430769230769231,-0.415384615384615,-0.4,-0.384615384615385,-0.369230769230769,
-0.353846153846154,-0.338461538461538,-0.323076923076923,-0.307692307692308,
-0.292307692307692,-0.276923076923077,-0.261538461538462,-0.246153846153846,
-0.230769230769231,-0.215384615384615,-0.2,-0.184615384615385,-0.169230769230769,
-0.153846153846154,-0.138461538461538,-0.123076923076923,-0.107692307692308,
-0.0923076923076923,-0.0769230769230769,-0.0615384615384615,-0.0461538461538462,
-0.0307692307692308,-0.0153846153846154,0.),(-1.,1.),.UNSPECIFIED.)
GEOMETRIC_REPRESENTATION_ITEM()
RATIONAL_B_SPLINE_SURFACE(((1.,1.),(1.,1.),(1.,1.),(1.,1.),(1.,1.),(1.,
1.),(1.,1.),(1.,1.),(1.,1.),(1.,1.),(1.,1.),(1.,1.),(1.,1.),(1.,1.),(1.,
1.),(1.,1.),(1.,1.),(1.,1.),(1.,1.),(1.,1.),(1.,1.),(1.,1.),(1.,1.),(1.,
1.),(1.,1.),(1.,1.),(1.,1.),(1.,1.),(1.,1.),(1.,1.),(1.,1.),(1.,1.),(1.,
1.),(1.,1.),(1.,1.),(1.,1.),(1.,1.),(1.,1.),(1.,1.),(1.,1.),(1.,1.),(1.,
1.),(1.,1.),(1.,1.),(1.,1.),(1.,1.),(1.,1.),(1.,1.),(1.,1.),(1.,1.),(1.,
1.),(1.,1.),(1.,1.),(1.,1.),(1.,1.),(1.,1.),(1.,1.),(1.,1.),(1.,1.),(1.,
1.),(1.,1.),(1.,1.),(1.,1.),(1.,1.),(1.,1.),(1.,1.),(1.,1.),(1.,1.),(1.,
1.),(1.,1.)))
REPRESENTATION_ITEM('')
SURFACE()
);
#37=(
BOUNDED_SURFACE()
B_SPLINE_SURFACE(5,1,((#35348,#35349),(#35350,#35351),(#35352,#35353),(#35354,
#35355),(#35356,#35357),(#35358,#35359),(#35360,#35361),(#35362,#35363),
(#35364,#35365),(#35366,#35367),(#35368,#35369),(#35370,#35371),(#35372,
#35373),(#35374,#35375),(#35376,#35377),(#35378,#35379),(#35380,#35381),
(#35382,#35383),(#35384,#35385),(#35386,#35387),(#35388,#35389),(#35390,
#35391),(#35392,#35393),(#35394,#35395),(#35396,#35397),(#35398,#35399),
(#35400,#35401),(#35402,#35403),(#35404,#35405),(#35406,#35407),(#35408,
#35409),(#35410,#35411),(#35412,#35413),(#35414,#35415),(#35416,#35417),
(#35418,#35419),(#35420,#35421),(#35422,#35423),(#35424,#35425),(#35426,
#35427),(#35428,#35429),(#35430,#35431),(#35432,#35433),(#35434,#35435),
(#35436,#35437),(#35438,#35439),(#35440,#35441),(#35442,#35443),(#35444,
#35445),(#35446,#35447),(#35448,#35449),(#35450,#35451),(#35452,#35453),
(#35454,#35455),(#35456,#35457),(#35458,#35459),(#35460,#35461),(#35462,
#35463),(#35464,#35465),(#35466,#35467),(#35468,#35469),(#35470,#35471),
(#35472,#35473),(#35474,#35475),(#35476,#35477),(#35478,#35479),(#35480,
#35481),(#35482,#35483),(#35484,#35485),(#35486,#35487)),.UNSPECIFIED.,
 .F.,.F.,.F.)
B_SPLINE_SURFACE_WITH_KNOTS((6,1,1,1,1,1,1,1,1,1,1,1,1,1,1,1,1,1,1,1,1,
1,1,1,1,1,1,1,1,1,1,1,1,1,1,1,1,1,1,1,1,1,1,1,1,1,1,1,1,1,1,1,1,1,1,1,1,
1,1,1,1,1,1,1,1,6),(2,2),(-1.,-0.984615384615383,-0.969230769230768,-0.953846153846152,
-0.938461538461537,-0.923076923076922,-0.907692307692306,-0.892307692307691,
-0.876923076923076,-0.86153846153846,-0.846153846153845,-0.83076923076923,
-0.815384615384614,-0.799999999999999,-0.784615384615384,-0.769230769230768,
-0.753846153846153,-0.738461538461538,-0.723076923076922,-0.707692307692307,
-0.692307692307692,-0.676923076923076,-0.661538461538461,-0.646153846153846,
-0.63076923076923,-0.615384615384615,-0.6,-0.584615384615384,-0.569230769230769,
-0.553846153846154,-0.538461538461538,-0.523076923076923,-0.507692307692308,
-0.492307692307692,-0.476923076923077,-0.461538461538462,-0.446153846153846,
-0.430769230769231,-0.415384615384615,-0.4,-0.384615384615385,-0.369230769230769,
-0.353846153846154,-0.338461538461538,-0.323076923076923,-0.307692307692308,
-0.292307692307692,-0.276923076923077,-0.261538461538462,-0.246153846153846,
-0.230769230769231,-0.215384615384615,-0.2,-0.184615384615385,-0.169230769230769,
-0.153846153846154,-0.138461538461538,-0.123076923076923,-0.107692307692308,
-0.0923076923076923,-0.0769230769230769,-0.0615384615384615,-0.0461538461538462,
-0.0307692307692308,-0.0153846153846154,0.),(-1.,1.),.UNSPECIFIED.)
GEOMETRIC_REPRESENTATION_ITEM()
RATIONAL_B_SPLINE_SURFACE(((1.,1.),(1.,1.),(1.,1.),(1.,1.),(1.,1.),(1.,
1.),(1.,1.),(1.,1.),(1.,1.),(1.,1.),(1.,1.),(1.,1.),(1.,1.),(1.,1.),(1.,
1.),(1.,1.),(1.,1.),(1.,1.),(1.,1.),(1.,1.),(1.,1.),(1.,1.),(1.,1.),(1.,
1.),(1.,1.),(1.,1.),(1.,1.),(1.,1.),(1.,1.),(1.,1.),(1.,1.),(1.,1.),(1.,
1.),(1.,1.),(1.,1.),(1.,1.),(1.,1.),(1.,1.),(1.,1.),(1.,1.),(1.,1.),(1.,
1.),(1.,1.),(1.,1.),(1.,1.),(1.,1.),(1.,1.),(1.,1.),(1.,1.),(1.,1.),(1.,
1.),(1.,1.),(1.,1.),(1.,1.),(1.,1.),(1.,1.),(1.,1.),(1.,1.),(1.,1.),(1.,
1.),(1.,1.),(1.,1.),(1.,1.),(1.,1.),(1.,1.),(1.,1.),(1.,1.),(1.,1.),(1.,
1.),(1.,1.)))
REPRESENTATION_ITEM('')
SURFACE()
);
#38=(
BOUNDED_SURFACE()
B_SPLINE_SURFACE(5,1,((#35564,#35565),(#35566,#35567),(#35568,#35569),(#35570,
#35571),(#35572,#35573),(#35574,#35575),(#35576,#35577),(#35578,#35579),
(#35580,#35581),(#35582,#35583),(#35584,#35585),(#35586,#35587),(#35588,
#35589),(#35590,#35591),(#35592,#35593),(#35594,#35595),(#35596,#35597),
(#35598,#35599),(#35600,#35601),(#35602,#35603),(#35604,#35605),(#35606,
#35607),(#35608,#35609),(#35610,#35611),(#35612,#35613),(#35614,#35615),
(#35616,#35617),(#35618,#35619),(#35620,#35621),(#35622,#35623),(#35624,
#35625),(#35626,#35627),(#35628,#35629),(#35630,#35631),(#35632,#35633),
(#35634,#35635),(#35636,#35637),(#35638,#35639),(#35640,#35641),(#35642,
#35643),(#35644,#35645),(#35646,#35647),(#35648,#35649),(#35650,#35651),
(#35652,#35653),(#35654,#35655),(#35656,#35657),(#35658,#35659),(#35660,
#35661),(#35662,#35663),(#35664,#35665),(#35666,#35667),(#35668,#35669),
(#35670,#35671),(#35672,#35673),(#35674,#35675),(#35676,#35677),(#35678,
#35679),(#35680,#35681),(#35682,#35683),(#35684,#35685),(#35686,#35687),
(#35688,#35689),(#35690,#35691),(#35692,#35693),(#35694,#35695),(#35696,
#35697),(#35698,#35699),(#35700,#35701),(#35702,#35703)),.UNSPECIFIED.,
 .F.,.F.,.F.)
B_SPLINE_SURFACE_WITH_KNOTS((6,1,1,1,1,1,1,1,1,1,1,1,1,1,1,1,1,1,1,1,1,
1,1,1,1,1,1,1,1,1,1,1,1,1,1,1,1,1,1,1,1,1,1,1,1,1,1,1,1,1,1,1,1,1,1,1,1,
1,1,1,1,1,1,1,1,6),(2,2),(-1.,-0.984615384615383,-0.969230769230768,-0.953846153846152,
-0.938461538461537,-0.923076923076922,-0.907692307692306,-0.892307692307691,
-0.876923076923076,-0.86153846153846,-0.846153846153845,-0.83076923076923,
-0.815384615384614,-0.799999999999999,-0.784615384615384,-0.769230769230768,
-0.753846153846153,-0.738461538461538,-0.723076923076922,-0.707692307692307,
-0.692307692307692,-0.676923076923076,-0.661538461538461,-0.646153846153846,
-0.63076923076923,-0.615384615384615,-0.6,-0.584615384615384,-0.569230769230769,
-0.553846153846154,-0.538461538461538,-0.523076923076923,-0.507692307692308,
-0.492307692307692,-0.476923076923077,-0.461538461538462,-0.446153846153846,
-0.430769230769231,-0.415384615384615,-0.4,-0.384615384615385,-0.369230769230769,
-0.353846153846154,-0.338461538461538,-0.323076923076923,-0.307692307692308,
-0.292307692307692,-0.276923076923077,-0.261538461538462,-0.246153846153846,
-0.230769230769231,-0.215384615384615,-0.2,-0.184615384615385,-0.169230769230769,
-0.153846153846154,-0.138461538461538,-0.123076923076923,-0.107692307692308,
-0.0923076923076923,-0.0769230769230769,-0.0615384615384615,-0.0461538461538462,
-0.0307692307692308,-0.0153846153846154,0.),(-1.,1.),.UNSPECIFIED.)
GEOMETRIC_REPRESENTATION_ITEM()
RATIONAL_B_SPLINE_SURFACE(((1.,1.),(1.,1.),(1.,1.),(1.,1.),(1.,1.),(1.,
1.),(1.,1.),(1.,1.),(1.,1.),(1.,1.),(1.,1.),(1.,1.),(1.,1.),(1.,1.),(1.,
1.),(1.,1.),(1.,1.),(1.,1.),(1.,1.),(1.,1.),(1.,1.),(1.,1.),(1.,1.),(1.,
1.),(1.,1.),(1.,1.),(1.,1.),(1.,1.),(1.,1.),(1.,1.),(1.,1.),(1.,1.),(1.,
1.),(1.,1.),(1.,1.),(1.,1.),(1.,1.),(1.,1.),(1.,1.),(1.,1.),(1.,1.),(1.,
1.),(1.,1.),(1.,1.),(1.,1.),(1.,1.),(1.,1.),(1.,1.),(1.,1.),(1.,1.),(1.,
1.),(1.,1.),(1.,1.),(1.,1.),(1.,1.),(1.,1.),(1.,1.),(1.,1.),(1.,1.),(1.,
1.),(1.,1.),(1.,1.),(1.,1.),(1.,1.),(1.,1.),(1.,1.),(1.,1.),(1.,1.),(1.,
1.),(1.,1.)))
REPRESENTATION_ITEM('')
SURFACE()
);
#39=(
BOUNDED_SURFACE()
B_SPLINE_SURFACE(5,1,((#35780,#35781),(#35782,#35783),(#35784,#35785),(#35786,
#35787),(#35788,#35789),(#35790,#35791),(#35792,#35793),(#35794,#35795),
(#35796,#35797),(#35798,#35799),(#35800,#35801),(#35802,#35803),(#35804,
#35805),(#35806,#35807),(#35808,#35809),(#35810,#35811),(#35812,#35813),
(#35814,#35815),(#35816,#35817),(#35818,#35819),(#35820,#35821),(#35822,
#35823),(#35824,#35825),(#35826,#35827),(#35828,#35829),(#35830,#35831),
(#35832,#35833),(#35834,#35835),(#35836,#35837),(#35838,#35839),(#35840,
#35841),(#35842,#35843),(#35844,#35845),(#35846,#35847),(#35848,#35849),
(#35850,#35851),(#35852,#35853),(#35854,#35855),(#35856,#35857),(#35858,
#35859),(#35860,#35861),(#35862,#35863),(#35864,#35865),(#35866,#35867),
(#35868,#35869),(#35870,#35871),(#35872,#35873),(#35874,#35875),(#35876,
#35877),(#35878,#35879),(#35880,#35881),(#35882,#35883),(#35884,#35885),
(#35886,#35887),(#35888,#35889),(#35890,#35891),(#35892,#35893),(#35894,
#35895),(#35896,#35897),(#35898,#35899),(#35900,#35901),(#35902,#35903),
(#35904,#35905),(#35906,#35907),(#35908,#35909),(#35910,#35911),(#35912,
#35913),(#35914,#35915),(#35916,#35917),(#35918,#35919)),.UNSPECIFIED.,
 .F.,.F.,.F.)
B_SPLINE_SURFACE_WITH_KNOTS((6,1,1,1,1,1,1,1,1,1,1,1,1,1,1,1,1,1,1,1,1,
1,1,1,1,1,1,1,1,1,1,1,1,1,1,1,1,1,1,1,1,1,1,1,1,1,1,1,1,1,1,1,1,1,1,1,1,
1,1,1,1,1,1,1,1,6),(2,2),(-1.,-0.984615384615383,-0.969230769230768,-0.953846153846152,
-0.938461538461537,-0.923076923076922,-0.907692307692306,-0.892307692307691,
-0.876923076923076,-0.86153846153846,-0.846153846153845,-0.83076923076923,
-0.815384615384614,-0.799999999999999,-0.784615384615384,-0.769230769230768,
-0.753846153846153,-0.738461538461538,-0.723076923076922,-0.707692307692307,
-0.692307692307692,-0.676923076923076,-0.661538461538461,-0.646153846153846,
-0.63076923076923,-0.615384615384615,-0.6,-0.584615384615384,-0.569230769230769,
-0.553846153846154,-0.538461538461538,-0.523076923076923,-0.507692307692308,
-0.492307692307692,-0.476923076923077,-0.461538461538462,-0.446153846153846,
-0.430769230769231,-0.415384615384615,-0.4,-0.384615384615385,-0.369230769230769,
-0.353846153846154,-0.338461538461538,-0.323076923076923,-0.307692307692308,
-0.292307692307692,-0.276923076923077,-0.261538461538462,-0.246153846153846,
-0.230769230769231,-0.215384615384615,-0.2,-0.184615384615385,-0.169230769230769,
-0.153846153846154,-0.138461538461538,-0.123076923076923,-0.107692307692308,
-0.0923076923076923,-0.0769230769230769,-0.0615384615384615,-0.0461538461538462,
-0.0307692307692308,-0.0153846153846154,0.),(-1.,1.),.UNSPECIFIED.)
GEOMETRIC_REPRESENTATION_ITEM()
RATIONAL_B_SPLINE_SURFACE(((1.,1.),(1.,1.),(1.,1.),(1.,1.),(1.,1.),(1.,
1.),(1.,1.),(1.,1.),(1.,1.),(1.,1.),(1.,1.),(1.,1.),(1.,1.),(1.,1.),(1.,
1.),(1.,1.),(1.,1.),(1.,1.),(1.,1.),(1.,1.),(1.,1.),(1.,1.),(1.,1.),(1.,
1.),(1.,1.),(1.,1.),(1.,1.),(1.,1.),(1.,1.),(1.,1.),(1.,1.),(1.,1.),(1.,
1.),(1.,1.),(1.,1.),(1.,1.),(1.,1.),(1.,1.),(1.,1.),(1.,1.),(1.,1.),(1.,
1.),(1.,1.),(1.,1.),(1.,1.),(1.,1.),(1.,1.),(1.,1.),(1.,1.),(1.,1.),(1.,
1.),(1.,1.),(1.,1.),(1.,1.),(1.,1.),(1.,1.),(1.,1.),(1.,1.),(1.,1.),(1.,
1.),(1.,1.),(1.,1.),(1.,1.),(1.,1.),(1.,1.),(1.,1.),(1.,1.),(1.,1.),(1.,
1.),(1.,1.)))
REPRESENTATION_ITEM('')
SURFACE()
);
#40=(
BOUNDED_SURFACE()
B_SPLINE_SURFACE(5,1,((#35996,#35997),(#35998,#35999),(#36000,#36001),(#36002,
#36003),(#36004,#36005),(#36006,#36007),(#36008,#36009),(#36010,#36011),
(#36012,#36013),(#36014,#36015),(#36016,#36017),(#36018,#36019),(#36020,
#36021),(#36022,#36023),(#36024,#36025),(#36026,#36027),(#36028,#36029),
(#36030,#36031),(#36032,#36033),(#36034,#36035),(#36036,#36037),(#36038,
#36039),(#36040,#36041),(#36042,#36043),(#36044,#36045),(#36046,#36047),
(#36048,#36049),(#36050,#36051),(#36052,#36053),(#36054,#36055),(#36056,
#36057),(#36058,#36059),(#36060,#36061),(#36062,#36063),(#36064,#36065),
(#36066,#36067),(#36068,#36069),(#36070,#36071),(#36072,#36073),(#36074,
#36075),(#36076,#36077),(#36078,#36079),(#36080,#36081),(#36082,#36083),
(#36084,#36085),(#36086,#36087),(#36088,#36089),(#36090,#36091),(#36092,
#36093),(#36094,#36095),(#36096,#36097),(#36098,#36099),(#36100,#36101),
(#36102,#36103),(#36104,#36105),(#36106,#36107),(#36108,#36109),(#36110,
#36111),(#36112,#36113),(#36114,#36115),(#36116,#36117),(#36118,#36119),
(#36120,#36121),(#36122,#36123),(#36124,#36125),(#36126,#36127),(#36128,
#36129),(#36130,#36131),(#36132,#36133),(#36134,#36135)),.UNSPECIFIED.,
 .F.,.F.,.F.)
B_SPLINE_SURFACE_WITH_KNOTS((6,1,1,1,1,1,1,1,1,1,1,1,1,1,1,1,1,1,1,1,1,
1,1,1,1,1,1,1,1,1,1,1,1,1,1,1,1,1,1,1,1,1,1,1,1,1,1,1,1,1,1,1,1,1,1,1,1,
1,1,1,1,1,1,1,1,6),(2,2),(-1.,-0.984615384615383,-0.969230769230768,-0.953846153846152,
-0.938461538461537,-0.923076923076922,-0.907692307692306,-0.892307692307691,
-0.876923076923076,-0.86153846153846,-0.846153846153845,-0.83076923076923,
-0.815384615384614,-0.799999999999999,-0.784615384615384,-0.769230769230768,
-0.753846153846153,-0.738461538461538,-0.723076923076922,-0.707692307692307,
-0.692307692307692,-0.676923076923076,-0.661538461538461,-0.646153846153846,
-0.63076923076923,-0.615384615384615,-0.6,-0.584615384615384,-0.569230769230769,
-0.553846153846154,-0.538461538461538,-0.523076923076923,-0.507692307692308,
-0.492307692307692,-0.476923076923077,-0.461538461538462,-0.446153846153846,
-0.430769230769231,-0.415384615384615,-0.4,-0.384615384615385,-0.369230769230769,
-0.353846153846154,-0.338461538461538,-0.323076923076923,-0.307692307692308,
-0.292307692307692,-0.276923076923077,-0.261538461538462,-0.246153846153846,
-0.230769230769231,-0.215384615384615,-0.2,-0.184615384615385,-0.169230769230769,
-0.153846153846154,-0.138461538461538,-0.123076923076923,-0.107692307692308,
-0.0923076923076923,-0.0769230769230769,-0.0615384615384615,-0.0461538461538462,
-0.0307692307692308,-0.0153846153846154,0.),(-1.,1.),.UNSPECIFIED.)
GEOMETRIC_REPRESENTATION_ITEM()
RATIONAL_B_SPLINE_SURFACE(((1.,1.),(1.,1.),(1.,1.),(1.,1.),(1.,1.),(1.,
1.),(1.,1.),(1.,1.),(1.,1.),(1.,1.),(1.,1.),(1.,1.),(1.,1.),(1.,1.),(1.,
1.),(1.,1.),(1.,1.),(1.,1.),(1.,1.),(1.,1.),(1.,1.),(1.,1.),(1.,1.),(1.,
1.),(1.,1.),(1.,1.),(1.,1.),(1.,1.),(1.,1.),(1.,1.),(1.,1.),(1.,1.),(1.,
1.),(1.,1.),(1.,1.),(1.,1.),(1.,1.),(1.,1.),(1.,1.),(1.,1.),(1.,1.),(1.,
1.),(1.,1.),(1.,1.),(1.,1.),(1.,1.),(1.,1.),(1.,1.),(1.,1.),(1.,1.),(1.,
1.),(1.,1.),(1.,1.),(1.,1.),(1.,1.),(1.,1.),(1.,1.),(1.,1.),(1.,1.),(1.,
1.),(1.,1.),(1.,1.),(1.,1.),(1.,1.),(1.,1.),(1.,1.),(1.,1.),(1.,1.),(1.,
1.),(1.,1.)))
REPRESENTATION_ITEM('')
SURFACE()
);
#41=(
BOUNDED_SURFACE()
B_SPLINE_SURFACE(5,1,((#36212,#36213),(#36214,#36215),(#36216,#36217),(#36218,
#36219),(#36220,#36221),(#36222,#36223),(#36224,#36225),(#36226,#36227),
(#36228,#36229),(#36230,#36231),(#36232,#36233),(#36234,#36235),(#36236,
#36237),(#36238,#36239),(#36240,#36241),(#36242,#36243),(#36244,#36245),
(#36246,#36247),(#36248,#36249),(#36250,#36251),(#36252,#36253),(#36254,
#36255),(#36256,#36257),(#36258,#36259),(#36260,#36261),(#36262,#36263),
(#36264,#36265),(#36266,#36267),(#36268,#36269),(#36270,#36271),(#36272,
#36273),(#36274,#36275),(#36276,#36277),(#36278,#36279),(#36280,#36281),
(#36282,#36283),(#36284,#36285),(#36286,#36287),(#36288,#36289),(#36290,
#36291),(#36292,#36293),(#36294,#36295),(#36296,#36297),(#36298,#36299),
(#36300,#36301),(#36302,#36303),(#36304,#36305),(#36306,#36307),(#36308,
#36309),(#36310,#36311),(#36312,#36313),(#36314,#36315),(#36316,#36317),
(#36318,#36319),(#36320,#36321),(#36322,#36323),(#36324,#36325),(#36326,
#36327),(#36328,#36329),(#36330,#36331),(#36332,#36333),(#36334,#36335),
(#36336,#36337),(#36338,#36339),(#36340,#36341),(#36342,#36343),(#36344,
#36345),(#36346,#36347),(#36348,#36349),(#36350,#36351)),.UNSPECIFIED.,
 .F.,.F.,.F.)
B_SPLINE_SURFACE_WITH_KNOTS((6,1,1,1,1,1,1,1,1,1,1,1,1,1,1,1,1,1,1,1,1,
1,1,1,1,1,1,1,1,1,1,1,1,1,1,1,1,1,1,1,1,1,1,1,1,1,1,1,1,1,1,1,1,1,1,1,1,
1,1,1,1,1,1,1,1,6),(2,2),(-1.,-0.984615384615383,-0.969230769230768,-0.953846153846152,
-0.938461538461537,-0.923076923076922,-0.907692307692306,-0.892307692307691,
-0.876923076923076,-0.86153846153846,-0.846153846153845,-0.83076923076923,
-0.815384615384614,-0.799999999999999,-0.784615384615384,-0.769230769230768,
-0.753846153846153,-0.738461538461538,-0.723076923076922,-0.707692307692307,
-0.692307692307692,-0.676923076923076,-0.661538461538461,-0.646153846153846,
-0.63076923076923,-0.615384615384615,-0.6,-0.584615384615384,-0.569230769230769,
-0.553846153846154,-0.538461538461538,-0.523076923076923,-0.507692307692308,
-0.492307692307692,-0.476923076923077,-0.461538461538462,-0.446153846153846,
-0.430769230769231,-0.415384615384615,-0.4,-0.384615384615385,-0.369230769230769,
-0.353846153846154,-0.338461538461538,-0.323076923076923,-0.307692307692308,
-0.292307692307692,-0.276923076923077,-0.261538461538462,-0.246153846153846,
-0.230769230769231,-0.215384615384615,-0.2,-0.184615384615385,-0.169230769230769,
-0.153846153846154,-0.138461538461538,-0.123076923076923,-0.107692307692308,
-0.0923076923076923,-0.0769230769230769,-0.0615384615384615,-0.0461538461538462,
-0.0307692307692308,-0.0153846153846154,0.),(-1.,1.),.UNSPECIFIED.)
GEOMETRIC_REPRESENTATION_ITEM()
RATIONAL_B_SPLINE_SURFACE(((1.,1.),(1.,1.),(1.,1.),(1.,1.),(1.,1.),(1.,
1.),(1.,1.),(1.,1.),(1.,1.),(1.,1.),(1.,1.),(1.,1.),(1.,1.),(1.,1.),(1.,
1.),(1.,1.),(1.,1.),(1.,1.),(1.,1.),(1.,1.),(1.,1.),(1.,1.),(1.,1.),(1.,
1.),(1.,1.),(1.,1.),(1.,1.),(1.,1.),(1.,1.),(1.,1.),(1.,1.),(1.,1.),(1.,
1.),(1.,1.),(1.,1.),(1.,1.),(1.,1.),(1.,1.),(1.,1.),(1.,1.),(1.,1.),(1.,
1.),(1.,1.),(1.,1.),(1.,1.),(1.,1.),(1.,1.),(1.,1.),(1.,1.),(1.,1.),(1.,
1.),(1.,1.),(1.,1.),(1.,1.),(1.,1.),(1.,1.),(1.,1.),(1.,1.),(1.,1.),(1.,
1.),(1.,1.),(1.,1.),(1.,1.),(1.,1.),(1.,1.),(1.,1.),(1.,1.),(1.,1.),(1.,
1.),(1.,1.)))
REPRESENTATION_ITEM('')
SURFACE()
);
#42=(
BOUNDED_SURFACE()
B_SPLINE_SURFACE(5,1,((#36428,#36429),(#36430,#36431),(#36432,#36433),(#36434,
#36435),(#36436,#36437),(#36438,#36439),(#36440,#36441),(#36442,#36443),
(#36444,#36445),(#36446,#36447),(#36448,#36449),(#36450,#36451),(#36452,
#36453),(#36454,#36455),(#36456,#36457),(#36458,#36459),(#36460,#36461),
(#36462,#36463),(#36464,#36465),(#36466,#36467),(#36468,#36469),(#36470,
#36471),(#36472,#36473),(#36474,#36475),(#36476,#36477),(#36478,#36479),
(#36480,#36481),(#36482,#36483),(#36484,#36485),(#36486,#36487),(#36488,
#36489),(#36490,#36491),(#36492,#36493),(#36494,#36495),(#36496,#36497),
(#36498,#36499),(#36500,#36501),(#36502,#36503),(#36504,#36505),(#36506,
#36507),(#36508,#36509),(#36510,#36511),(#36512,#36513),(#36514,#36515),
(#36516,#36517),(#36518,#36519),(#36520,#36521),(#36522,#36523),(#36524,
#36525),(#36526,#36527),(#36528,#36529),(#36530,#36531),(#36532,#36533),
(#36534,#36535),(#36536,#36537),(#36538,#36539),(#36540,#36541),(#36542,
#36543),(#36544,#36545),(#36546,#36547),(#36548,#36549),(#36550,#36551),
(#36552,#36553),(#36554,#36555),(#36556,#36557),(#36558,#36559),(#36560,
#36561),(#36562,#36563),(#36564,#36565),(#36566,#36567)),.UNSPECIFIED.,
 .F.,.F.,.F.)
B_SPLINE_SURFACE_WITH_KNOTS((6,1,1,1,1,1,1,1,1,1,1,1,1,1,1,1,1,1,1,1,1,
1,1,1,1,1,1,1,1,1,1,1,1,1,1,1,1,1,1,1,1,1,1,1,1,1,1,1,1,1,1,1,1,1,1,1,1,
1,1,1,1,1,1,1,1,6),(2,2),(-1.,-0.984615384615383,-0.969230769230768,-0.953846153846152,
-0.938461538461537,-0.923076923076922,-0.907692307692306,-0.892307692307691,
-0.876923076923076,-0.86153846153846,-0.846153846153845,-0.83076923076923,
-0.815384615384614,-0.799999999999999,-0.784615384615384,-0.769230769230768,
-0.753846153846153,-0.738461538461538,-0.723076923076922,-0.707692307692307,
-0.692307692307692,-0.676923076923076,-0.661538461538461,-0.646153846153846,
-0.63076923076923,-0.615384615384615,-0.6,-0.584615384615384,-0.569230769230769,
-0.553846153846154,-0.538461538461538,-0.523076923076923,-0.507692307692308,
-0.492307692307692,-0.476923076923077,-0.461538461538462,-0.446153846153846,
-0.430769230769231,-0.415384615384615,-0.4,-0.384615384615385,-0.369230769230769,
-0.353846153846154,-0.338461538461538,-0.323076923076923,-0.307692307692308,
-0.292307692307692,-0.276923076923077,-0.261538461538462,-0.246153846153846,
-0.230769230769231,-0.215384615384615,-0.2,-0.184615384615385,-0.169230769230769,
-0.153846153846154,-0.138461538461538,-0.123076923076923,-0.107692307692308,
-0.0923076923076923,-0.0769230769230769,-0.0615384615384615,-0.0461538461538462,
-0.0307692307692308,-0.0153846153846154,0.),(-1.,1.),.UNSPECIFIED.)
GEOMETRIC_REPRESENTATION_ITEM()
RATIONAL_B_SPLINE_SURFACE(((1.,1.),(1.,1.),(1.,1.),(1.,1.),(1.,1.),(1.,
1.),(1.,1.),(1.,1.),(1.,1.),(1.,1.),(1.,1.),(1.,1.),(1.,1.),(1.,1.),(1.,
1.),(1.,1.),(1.,1.),(1.,1.),(1.,1.),(1.,1.),(1.,1.),(1.,1.),(1.,1.),(1.,
1.),(1.,1.),(1.,1.),(1.,1.),(1.,1.),(1.,1.),(1.,1.),(1.,1.),(1.,1.),(1.,
1.),(1.,1.),(1.,1.),(1.,1.),(1.,1.),(1.,1.),(1.,1.),(1.,1.),(1.,1.),(1.,
1.),(1.,1.),(1.,1.),(1.,1.),(1.,1.),(1.,1.),(1.,1.),(1.,1.),(1.,1.),(1.,
1.),(1.,1.),(1.,1.),(1.,1.),(1.,1.),(1.,1.),(1.,1.),(1.,1.),(1.,1.),(1.,
1.),(1.,1.),(1.,1.),(1.,1.),(1.,1.),(1.,1.),(1.,1.),(1.,1.),(1.,1.),(1.,
1.),(1.,1.)))
REPRESENTATION_ITEM('')
SURFACE()
);
#43=(
BOUNDED_SURFACE()
B_SPLINE_SURFACE(5,1,((#36644,#36645),(#36646,#36647),(#36648,#36649),(#36650,
#36651),(#36652,#36653),(#36654,#36655),(#36656,#36657),(#36658,#36659),
(#36660,#36661),(#36662,#36663),(#36664,#36665),(#36666,#36667),(#36668,
#36669),(#36670,#36671),(#36672,#36673),(#36674,#36675),(#36676,#36677),
(#36678,#36679),(#36680,#36681),(#36682,#36683),(#36684,#36685),(#36686,
#36687),(#36688,#36689),(#36690,#36691),(#36692,#36693),(#36694,#36695),
(#36696,#36697),(#36698,#36699),(#36700,#36701),(#36702,#36703),(#36704,
#36705),(#36706,#36707),(#36708,#36709),(#36710,#36711),(#36712,#36713),
(#36714,#36715),(#36716,#36717),(#36718,#36719),(#36720,#36721),(#36722,
#36723),(#36724,#36725),(#36726,#36727),(#36728,#36729),(#36730,#36731),
(#36732,#36733),(#36734,#36735),(#36736,#36737),(#36738,#36739),(#36740,
#36741),(#36742,#36743),(#36744,#36745),(#36746,#36747),(#36748,#36749),
(#36750,#36751),(#36752,#36753),(#36754,#36755),(#36756,#36757),(#36758,
#36759),(#36760,#36761),(#36762,#36763),(#36764,#36765),(#36766,#36767),
(#36768,#36769),(#36770,#36771),(#36772,#36773),(#36774,#36775),(#36776,
#36777),(#36778,#36779),(#36780,#36781),(#36782,#36783)),.UNSPECIFIED.,
 .F.,.F.,.F.)
B_SPLINE_SURFACE_WITH_KNOTS((6,1,1,1,1,1,1,1,1,1,1,1,1,1,1,1,1,1,1,1,1,
1,1,1,1,1,1,1,1,1,1,1,1,1,1,1,1,1,1,1,1,1,1,1,1,1,1,1,1,1,1,1,1,1,1,1,1,
1,1,1,1,1,1,1,1,6),(2,2),(-1.,-0.984615384615383,-0.969230769230768,-0.953846153846152,
-0.938461538461537,-0.923076923076922,-0.907692307692306,-0.892307692307691,
-0.876923076923076,-0.86153846153846,-0.846153846153845,-0.83076923076923,
-0.815384615384614,-0.799999999999999,-0.784615384615384,-0.769230769230768,
-0.753846153846153,-0.738461538461538,-0.723076923076922,-0.707692307692307,
-0.692307692307692,-0.676923076923076,-0.661538461538461,-0.646153846153846,
-0.63076923076923,-0.615384615384615,-0.6,-0.584615384615384,-0.569230769230769,
-0.553846153846154,-0.538461538461538,-0.523076923076923,-0.507692307692308,
-0.492307692307692,-0.476923076923077,-0.461538461538462,-0.446153846153846,
-0.430769230769231,-0.415384615384615,-0.4,-0.384615384615385,-0.369230769230769,
-0.353846153846154,-0.338461538461538,-0.323076923076923,-0.307692307692308,
-0.292307692307692,-0.276923076923077,-0.261538461538462,-0.246153846153846,
-0.230769230769231,-0.215384615384615,-0.2,-0.184615384615385,-0.169230769230769,
-0.153846153846154,-0.138461538461538,-0.123076923076923,-0.107692307692308,
-0.0923076923076923,-0.0769230769230769,-0.0615384615384615,-0.0461538461538462,
-0.0307692307692308,-0.0153846153846154,0.),(-1.,1.),.UNSPECIFIED.)
GEOMETRIC_REPRESENTATION_ITEM()
RATIONAL_B_SPLINE_SURFACE(((1.,1.),(1.,1.),(1.,1.),(1.,1.),(1.,1.),(1.,
1.),(1.,1.),(1.,1.),(1.,1.),(1.,1.),(1.,1.),(1.,1.),(1.,1.),(1.,1.),(1.,
1.),(1.,1.),(1.,1.),(1.,1.),(1.,1.),(1.,1.),(1.,1.),(1.,1.),(1.,1.),(1.,
1.),(1.,1.),(1.,1.),(1.,1.),(1.,1.),(1.,1.),(1.,1.),(1.,1.),(1.,1.),(1.,
1.),(1.,1.),(1.,1.),(1.,1.),(1.,1.),(1.,1.),(1.,1.),(1.,1.),(1.,1.),(1.,
1.),(1.,1.),(1.,1.),(1.,1.),(1.,1.),(1.,1.),(1.,1.),(1.,1.),(1.,1.),(1.,
1.),(1.,1.),(1.,1.),(1.,1.),(1.,1.),(1.,1.),(1.,1.),(1.,1.),(1.,1.),(1.,
1.),(1.,1.),(1.,1.),(1.,1.),(1.,1.),(1.,1.),(1.,1.),(1.,1.),(1.,1.),(1.,
1.),(1.,1.)))
REPRESENTATION_ITEM('')
SURFACE()
);
#44=(
BOUNDED_SURFACE()
B_SPLINE_SURFACE(5,1,((#36860,#36861),(#36862,#36863),(#36864,#36865),(#36866,
#36867),(#36868,#36869),(#36870,#36871),(#36872,#36873),(#36874,#36875),
(#36876,#36877),(#36878,#36879),(#36880,#36881),(#36882,#36883),(#36884,
#36885),(#36886,#36887),(#36888,#36889),(#36890,#36891),(#36892,#36893),
(#36894,#36895),(#36896,#36897),(#36898,#36899),(#36900,#36901),(#36902,
#36903),(#36904,#36905),(#36906,#36907),(#36908,#36909),(#36910,#36911),
(#36912,#36913),(#36914,#36915),(#36916,#36917),(#36918,#36919),(#36920,
#36921),(#36922,#36923),(#36924,#36925),(#36926,#36927),(#36928,#36929),
(#36930,#36931),(#36932,#36933),(#36934,#36935),(#36936,#36937),(#36938,
#36939),(#36940,#36941),(#36942,#36943),(#36944,#36945),(#36946,#36947),
(#36948,#36949),(#36950,#36951),(#36952,#36953),(#36954,#36955),(#36956,
#36957),(#36958,#36959),(#36960,#36961),(#36962,#36963),(#36964,#36965),
(#36966,#36967),(#36968,#36969),(#36970,#36971),(#36972,#36973),(#36974,
#36975),(#36976,#36977),(#36978,#36979),(#36980,#36981),(#36982,#36983),
(#36984,#36985),(#36986,#36987),(#36988,#36989),(#36990,#36991),(#36992,
#36993),(#36994,#36995),(#36996,#36997),(#36998,#36999)),.UNSPECIFIED.,
 .F.,.F.,.F.)
B_SPLINE_SURFACE_WITH_KNOTS((6,1,1,1,1,1,1,1,1,1,1,1,1,1,1,1,1,1,1,1,1,
1,1,1,1,1,1,1,1,1,1,1,1,1,1,1,1,1,1,1,1,1,1,1,1,1,1,1,1,1,1,1,1,1,1,1,1,
1,1,1,1,1,1,1,1,6),(2,2),(-1.,-0.984615384615383,-0.969230769230768,-0.953846153846152,
-0.938461538461537,-0.923076923076922,-0.907692307692306,-0.892307692307691,
-0.876923076923076,-0.86153846153846,-0.846153846153845,-0.83076923076923,
-0.815384615384614,-0.799999999999999,-0.784615384615384,-0.769230769230768,
-0.753846153846153,-0.738461538461538,-0.723076923076922,-0.707692307692307,
-0.692307692307692,-0.676923076923076,-0.661538461538461,-0.646153846153846,
-0.63076923076923,-0.615384615384615,-0.6,-0.584615384615384,-0.569230769230769,
-0.553846153846154,-0.538461538461538,-0.523076923076923,-0.507692307692308,
-0.492307692307692,-0.476923076923077,-0.461538461538462,-0.446153846153846,
-0.430769230769231,-0.415384615384615,-0.4,-0.384615384615385,-0.369230769230769,
-0.353846153846154,-0.338461538461538,-0.323076923076923,-0.307692307692308,
-0.292307692307692,-0.276923076923077,-0.261538461538462,-0.246153846153846,
-0.230769230769231,-0.215384615384615,-0.2,-0.184615384615385,-0.169230769230769,
-0.153846153846154,-0.138461538461538,-0.123076923076923,-0.107692307692308,
-0.0923076923076923,-0.0769230769230769,-0.0615384615384615,-0.0461538461538462,
-0.0307692307692308,-0.0153846153846154,0.),(-1.,1.),.UNSPECIFIED.)
GEOMETRIC_REPRESENTATION_ITEM()
RATIONAL_B_SPLINE_SURFACE(((1.,1.),(1.,1.),(1.,1.),(1.,1.),(1.,1.),(1.,
1.),(1.,1.),(1.,1.),(1.,1.),(1.,1.),(1.,1.),(1.,1.),(1.,1.),(1.,1.),(1.,
1.),(1.,1.),(1.,1.),(1.,1.),(1.,1.),(1.,1.),(1.,1.),(1.,1.),(1.,1.),(1.,
1.),(1.,1.),(1.,1.),(1.,1.),(1.,1.),(1.,1.),(1.,1.),(1.,1.),(1.,1.),(1.,
1.),(1.,1.),(1.,1.),(1.,1.),(1.,1.),(1.,1.),(1.,1.),(1.,1.),(1.,1.),(1.,
1.),(1.,1.),(1.,1.),(1.,1.),(1.,1.),(1.,1.),(1.,1.),(1.,1.),(1.,1.),(1.,
1.),(1.,1.),(1.,1.),(1.,1.),(1.,1.),(1.,1.),(1.,1.),(1.,1.),(1.,1.),(1.,
1.),(1.,1.),(1.,1.),(1.,1.),(1.,1.),(1.,1.),(1.,1.),(1.,1.),(1.,1.),(1.,
1.),(1.,1.)))
REPRESENTATION_ITEM('')
SURFACE()
);
#45=(
BOUNDED_SURFACE()
B_SPLINE_SURFACE(5,1,((#37076,#37077),(#37078,#37079),(#37080,#37081),(#37082,
#37083),(#37084,#37085),(#37086,#37087),(#37088,#37089),(#37090,#37091),
(#37092,#37093),(#37094,#37095),(#37096,#37097),(#37098,#37099),(#37100,
#37101),(#37102,#37103),(#37104,#37105),(#37106,#37107),(#37108,#37109),
(#37110,#37111),(#37112,#37113),(#37114,#37115),(#37116,#37117),(#37118,
#37119),(#37120,#37121),(#37122,#37123),(#37124,#37125),(#37126,#37127),
(#37128,#37129),(#37130,#37131),(#37132,#37133),(#37134,#37135),(#37136,
#37137),(#37138,#37139),(#37140,#37141),(#37142,#37143),(#37144,#37145),
(#37146,#37147),(#37148,#37149),(#37150,#37151),(#37152,#37153),(#37154,
#37155),(#37156,#37157),(#37158,#37159),(#37160,#37161),(#37162,#37163),
(#37164,#37165),(#37166,#37167),(#37168,#37169),(#37170,#37171),(#37172,
#37173),(#37174,#37175),(#37176,#37177),(#37178,#37179),(#37180,#37181),
(#37182,#37183),(#37184,#37185),(#37186,#37187),(#37188,#37189),(#37190,
#37191),(#37192,#37193),(#37194,#37195),(#37196,#37197),(#37198,#37199),
(#37200,#37201),(#37202,#37203),(#37204,#37205),(#37206,#37207),(#37208,
#37209),(#37210,#37211),(#37212,#37213),(#37214,#37215)),.UNSPECIFIED.,
 .F.,.F.,.F.)
B_SPLINE_SURFACE_WITH_KNOTS((6,1,1,1,1,1,1,1,1,1,1,1,1,1,1,1,1,1,1,1,1,
1,1,1,1,1,1,1,1,1,1,1,1,1,1,1,1,1,1,1,1,1,1,1,1,1,1,1,1,1,1,1,1,1,1,1,1,
1,1,1,1,1,1,1,1,6),(2,2),(-1.,-0.984615384615383,-0.969230769230768,-0.953846153846152,
-0.938461538461537,-0.923076923076922,-0.907692307692306,-0.892307692307691,
-0.876923076923076,-0.86153846153846,-0.846153846153845,-0.83076923076923,
-0.815384615384614,-0.799999999999999,-0.784615384615384,-0.769230769230768,
-0.753846153846153,-0.738461538461538,-0.723076923076922,-0.707692307692307,
-0.692307692307692,-0.676923076923076,-0.661538461538461,-0.646153846153846,
-0.63076923076923,-0.615384615384615,-0.6,-0.584615384615384,-0.569230769230769,
-0.553846153846154,-0.538461538461538,-0.523076923076923,-0.507692307692308,
-0.492307692307692,-0.476923076923077,-0.461538461538462,-0.446153846153846,
-0.430769230769231,-0.415384615384615,-0.4,-0.384615384615385,-0.369230769230769,
-0.353846153846154,-0.338461538461538,-0.323076923076923,-0.307692307692308,
-0.292307692307692,-0.276923076923077,-0.261538461538462,-0.246153846153846,
-0.230769230769231,-0.215384615384615,-0.2,-0.184615384615385,-0.169230769230769,
-0.153846153846154,-0.138461538461538,-0.123076923076923,-0.107692307692308,
-0.0923076923076923,-0.0769230769230769,-0.0615384615384615,-0.0461538461538462,
-0.0307692307692308,-0.0153846153846154,0.),(-1.,1.),.UNSPECIFIED.)
GEOMETRIC_REPRESENTATION_ITEM()
RATIONAL_B_SPLINE_SURFACE(((1.,1.),(1.,1.),(1.,1.),(1.,1.),(1.,1.),(1.,
1.),(1.,1.),(1.,1.),(1.,1.),(1.,1.),(1.,1.),(1.,1.),(1.,1.),(1.,1.),(1.,
1.),(1.,1.),(1.,1.),(1.,1.),(1.,1.),(1.,1.),(1.,1.),(1.,1.),(1.,1.),(1.,
1.),(1.,1.),(1.,1.),(1.,1.),(1.,1.),(1.,1.),(1.,1.),(1.,1.),(1.,1.),(1.,
1.),(1.,1.),(1.,1.),(1.,1.),(1.,1.),(1.,1.),(1.,1.),(1.,1.),(1.,1.),(1.,
1.),(1.,1.),(1.,1.),(1.,1.),(1.,1.),(1.,1.),(1.,1.),(1.,1.),(1.,1.),(1.,
1.),(1.,1.),(1.,1.),(1.,1.),(1.,1.),(1.,1.),(1.,1.),(1.,1.),(1.,1.),(1.,
1.),(1.,1.),(1.,1.),(1.,1.),(1.,1.),(1.,1.),(1.,1.),(1.,1.),(1.,1.),(1.,
1.),(1.,1.)))
REPRESENTATION_ITEM('')
SURFACE()
);
#46=(
BOUNDED_SURFACE()
B_SPLINE_SURFACE(5,1,((#37292,#37293),(#37294,#37295),(#37296,#37297),(#37298,
#37299),(#37300,#37301),(#37302,#37303),(#37304,#37305),(#37306,#37307),
(#37308,#37309),(#37310,#37311),(#37312,#37313),(#37314,#37315),(#37316,
#37317),(#37318,#37319),(#37320,#37321),(#37322,#37323),(#37324,#37325),
(#37326,#37327),(#37328,#37329),(#37330,#37331),(#37332,#37333),(#37334,
#37335),(#37336,#37337),(#37338,#37339),(#37340,#37341),(#37342,#37343),
(#37344,#37345),(#37346,#37347),(#37348,#37349),(#37350,#37351),(#37352,
#37353),(#37354,#37355),(#37356,#37357),(#37358,#37359),(#37360,#37361),
(#37362,#37363),(#37364,#37365),(#37366,#37367),(#37368,#37369),(#37370,
#37371),(#37372,#37373),(#37374,#37375),(#37376,#37377),(#37378,#37379),
(#37380,#37381),(#37382,#37383),(#37384,#37385),(#37386,#37387),(#37388,
#37389),(#37390,#37391),(#37392,#37393),(#37394,#37395),(#37396,#37397),
(#37398,#37399),(#37400,#37401),(#37402,#37403),(#37404,#37405),(#37406,
#37407),(#37408,#37409),(#37410,#37411),(#37412,#37413),(#37414,#37415),
(#37416,#37417),(#37418,#37419),(#37420,#37421),(#37422,#37423),(#37424,
#37425),(#37426,#37427),(#37428,#37429),(#37430,#37431)),.UNSPECIFIED.,
 .F.,.F.,.F.)
B_SPLINE_SURFACE_WITH_KNOTS((6,1,1,1,1,1,1,1,1,1,1,1,1,1,1,1,1,1,1,1,1,
1,1,1,1,1,1,1,1,1,1,1,1,1,1,1,1,1,1,1,1,1,1,1,1,1,1,1,1,1,1,1,1,1,1,1,1,
1,1,1,1,1,1,1,1,6),(2,2),(-1.,-0.984615384615383,-0.969230769230768,-0.953846153846152,
-0.938461538461537,-0.923076923076922,-0.907692307692306,-0.892307692307691,
-0.876923076923076,-0.86153846153846,-0.846153846153845,-0.83076923076923,
-0.815384615384614,-0.799999999999999,-0.784615384615384,-0.769230769230768,
-0.753846153846153,-0.738461538461538,-0.723076923076922,-0.707692307692307,
-0.692307692307692,-0.676923076923076,-0.661538461538461,-0.646153846153846,
-0.63076923076923,-0.615384615384615,-0.6,-0.584615384615384,-0.569230769230769,
-0.553846153846154,-0.538461538461538,-0.523076923076923,-0.507692307692308,
-0.492307692307692,-0.476923076923077,-0.461538461538462,-0.446153846153846,
-0.430769230769231,-0.415384615384615,-0.4,-0.384615384615385,-0.369230769230769,
-0.353846153846154,-0.338461538461538,-0.323076923076923,-0.307692307692308,
-0.292307692307692,-0.276923076923077,-0.261538461538462,-0.246153846153846,
-0.230769230769231,-0.215384615384615,-0.2,-0.184615384615385,-0.169230769230769,
-0.153846153846154,-0.138461538461538,-0.123076923076923,-0.107692307692308,
-0.0923076923076923,-0.0769230769230769,-0.0615384615384615,-0.0461538461538462,
-0.0307692307692308,-0.0153846153846154,0.),(-1.,1.),.UNSPECIFIED.)
GEOMETRIC_REPRESENTATION_ITEM()
RATIONAL_B_SPLINE_SURFACE(((1.,1.),(1.,1.),(1.,1.),(1.,1.),(1.,1.),(1.,
1.),(1.,1.),(1.,1.),(1.,1.),(1.,1.),(1.,1.),(1.,1.),(1.,1.),(1.,1.),(1.,
1.),(1.,1.),(1.,1.),(1.,1.),(1.,1.),(1.,1.),(1.,1.),(1.,1.),(1.,1.),(1.,
1.),(1.,1.),(1.,1.),(1.,1.),(1.,1.),(1.,1.),(1.,1.),(1.,1.),(1.,1.),(1.,
1.),(1.,1.),(1.,1.),(1.,1.),(1.,1.),(1.,1.),(1.,1.),(1.,1.),(1.,1.),(1.,
1.),(1.,1.),(1.,1.),(1.,1.),(1.,1.),(1.,1.),(1.,1.),(1.,1.),(1.,1.),(1.,
1.),(1.,1.),(1.,1.),(1.,1.),(1.,1.),(1.,1.),(1.,1.),(1.,1.),(1.,1.),(1.,
1.),(1.,1.),(1.,1.),(1.,1.),(1.,1.),(1.,1.),(1.,1.),(1.,1.),(1.,1.),(1.,
1.),(1.,1.)))
REPRESENTATION_ITEM('')
SURFACE()
);
#47=(
BOUNDED_SURFACE()
B_SPLINE_SURFACE(5,1,((#37508,#37509),(#37510,#37511),(#37512,#37513),(#37514,
#37515),(#37516,#37517),(#37518,#37519),(#37520,#37521),(#37522,#37523),
(#37524,#37525),(#37526,#37527),(#37528,#37529),(#37530,#37531),(#37532,
#37533),(#37534,#37535),(#37536,#37537),(#37538,#37539),(#37540,#37541),
(#37542,#37543),(#37544,#37545),(#37546,#37547),(#37548,#37549),(#37550,
#37551),(#37552,#37553),(#37554,#37555),(#37556,#37557),(#37558,#37559),
(#37560,#37561),(#37562,#37563),(#37564,#37565),(#37566,#37567),(#37568,
#37569),(#37570,#37571),(#37572,#37573),(#37574,#37575),(#37576,#37577),
(#37578,#37579),(#37580,#37581),(#37582,#37583),(#37584,#37585),(#37586,
#37587),(#37588,#37589),(#37590,#37591),(#37592,#37593),(#37594,#37595),
(#37596,#37597),(#37598,#37599),(#37600,#37601),(#37602,#37603),(#37604,
#37605),(#37606,#37607),(#37608,#37609),(#37610,#37611),(#37612,#37613),
(#37614,#37615),(#37616,#37617),(#37618,#37619),(#37620,#37621),(#37622,
#37623),(#37624,#37625),(#37626,#37627),(#37628,#37629),(#37630,#37631),
(#37632,#37633),(#37634,#37635),(#37636,#37637),(#37638,#37639),(#37640,
#37641),(#37642,#37643),(#37644,#37645),(#37646,#37647)),.UNSPECIFIED.,
 .F.,.F.,.F.)
B_SPLINE_SURFACE_WITH_KNOTS((6,1,1,1,1,1,1,1,1,1,1,1,1,1,1,1,1,1,1,1,1,
1,1,1,1,1,1,1,1,1,1,1,1,1,1,1,1,1,1,1,1,1,1,1,1,1,1,1,1,1,1,1,1,1,1,1,1,
1,1,1,1,1,1,1,1,6),(2,2),(-1.,-0.984615384615383,-0.969230769230768,-0.953846153846152,
-0.938461538461537,-0.923076923076922,-0.907692307692306,-0.892307692307691,
-0.876923076923076,-0.86153846153846,-0.846153846153845,-0.83076923076923,
-0.815384615384614,-0.799999999999999,-0.784615384615384,-0.769230769230768,
-0.753846153846153,-0.738461538461538,-0.723076923076922,-0.707692307692307,
-0.692307692307692,-0.676923076923076,-0.661538461538461,-0.646153846153846,
-0.63076923076923,-0.615384615384615,-0.6,-0.584615384615384,-0.569230769230769,
-0.553846153846154,-0.538461538461538,-0.523076923076923,-0.507692307692308,
-0.492307692307692,-0.476923076923077,-0.461538461538462,-0.446153846153846,
-0.430769230769231,-0.415384615384615,-0.4,-0.384615384615385,-0.369230769230769,
-0.353846153846154,-0.338461538461538,-0.323076923076923,-0.307692307692308,
-0.292307692307692,-0.276923076923077,-0.261538461538462,-0.246153846153846,
-0.230769230769231,-0.215384615384615,-0.2,-0.184615384615385,-0.169230769230769,
-0.153846153846154,-0.138461538461538,-0.123076923076923,-0.107692307692308,
-0.0923076923076923,-0.0769230769230769,-0.0615384615384615,-0.0461538461538462,
-0.0307692307692308,-0.0153846153846154,0.),(-1.,1.),.UNSPECIFIED.)
GEOMETRIC_REPRESENTATION_ITEM()
RATIONAL_B_SPLINE_SURFACE(((1.,1.),(1.,1.),(1.,1.),(1.,1.),(1.,1.),(1.,
1.),(1.,1.),(1.,1.),(1.,1.),(1.,1.),(1.,1.),(1.,1.),(1.,1.),(1.,1.),(1.,
1.),(1.,1.),(1.,1.),(1.,1.),(1.,1.),(1.,1.),(1.,1.),(1.,1.),(1.,1.),(1.,
1.),(1.,1.),(1.,1.),(1.,1.),(1.,1.),(1.,1.),(1.,1.),(1.,1.),(1.,1.),(1.,
1.),(1.,1.),(1.,1.),(1.,1.),(1.,1.),(1.,1.),(1.,1.),(1.,1.),(1.,1.),(1.,
1.),(1.,1.),(1.,1.),(1.,1.),(1.,1.),(1.,1.),(1.,1.),(1.,1.),(1.,1.),(1.,
1.),(1.,1.),(1.,1.),(1.,1.),(1.,1.),(1.,1.),(1.,1.),(1.,1.),(1.,1.),(1.,
1.),(1.,1.),(1.,1.),(1.,1.),(1.,1.),(1.,1.),(1.,1.),(1.,1.),(1.,1.),(1.,
1.),(1.,1.)))
REPRESENTATION_ITEM('')
SURFACE()
);
#48=(
BOUNDED_SURFACE()
B_SPLINE_SURFACE(5,1,((#37724,#37725),(#37726,#37727),(#37728,#37729),(#37730,
#37731),(#37732,#37733),(#37734,#37735),(#37736,#37737),(#37738,#37739),
(#37740,#37741),(#37742,#37743),(#37744,#37745),(#37746,#37747),(#37748,
#37749),(#37750,#37751),(#37752,#37753),(#37754,#37755),(#37756,#37757),
(#37758,#37759),(#37760,#37761),(#37762,#37763),(#37764,#37765),(#37766,
#37767),(#37768,#37769),(#37770,#37771),(#37772,#37773),(#37774,#37775),
(#37776,#37777),(#37778,#37779),(#37780,#37781),(#37782,#37783),(#37784,
#37785),(#37786,#37787),(#37788,#37789),(#37790,#37791),(#37792,#37793),
(#37794,#37795),(#37796,#37797),(#37798,#37799),(#37800,#37801),(#37802,
#37803),(#37804,#37805),(#37806,#37807),(#37808,#37809),(#37810,#37811),
(#37812,#37813),(#37814,#37815),(#37816,#37817),(#37818,#37819),(#37820,
#37821),(#37822,#37823),(#37824,#37825),(#37826,#37827),(#37828,#37829),
(#37830,#37831),(#37832,#37833),(#37834,#37835),(#37836,#37837),(#37838,
#37839),(#37840,#37841),(#37842,#37843),(#37844,#37845),(#37846,#37847),
(#37848,#37849),(#37850,#37851),(#37852,#37853),(#37854,#37855),(#37856,
#37857),(#37858,#37859),(#37860,#37861),(#37862,#37863)),.UNSPECIFIED.,
 .F.,.F.,.F.)
B_SPLINE_SURFACE_WITH_KNOTS((6,1,1,1,1,1,1,1,1,1,1,1,1,1,1,1,1,1,1,1,1,
1,1,1,1,1,1,1,1,1,1,1,1,1,1,1,1,1,1,1,1,1,1,1,1,1,1,1,1,1,1,1,1,1,1,1,1,
1,1,1,1,1,1,1,1,6),(2,2),(-1.,-0.984615384615383,-0.969230769230768,-0.953846153846152,
-0.938461538461537,-0.923076923076922,-0.907692307692306,-0.892307692307691,
-0.876923076923076,-0.86153846153846,-0.846153846153845,-0.83076923076923,
-0.815384615384614,-0.799999999999999,-0.784615384615384,-0.769230769230768,
-0.753846153846153,-0.738461538461538,-0.723076923076922,-0.707692307692307,
-0.692307692307692,-0.676923076923076,-0.661538461538461,-0.646153846153846,
-0.63076923076923,-0.615384615384615,-0.6,-0.584615384615384,-0.569230769230769,
-0.553846153846154,-0.538461538461538,-0.523076923076923,-0.507692307692308,
-0.492307692307692,-0.476923076923077,-0.461538461538462,-0.446153846153846,
-0.430769230769231,-0.415384615384615,-0.4,-0.384615384615385,-0.369230769230769,
-0.353846153846154,-0.338461538461538,-0.323076923076923,-0.307692307692308,
-0.292307692307692,-0.276923076923077,-0.261538461538462,-0.246153846153846,
-0.230769230769231,-0.215384615384615,-0.2,-0.184615384615385,-0.169230769230769,
-0.153846153846154,-0.138461538461538,-0.123076923076923,-0.107692307692308,
-0.0923076923076923,-0.0769230769230769,-0.0615384615384615,-0.0461538461538462,
-0.0307692307692308,-0.0153846153846154,0.),(-1.,1.),.UNSPECIFIED.)
GEOMETRIC_REPRESENTATION_ITEM()
RATIONAL_B_SPLINE_SURFACE(((1.,1.),(1.,1.),(1.,1.),(1.,1.),(1.,1.),(1.,
1.),(1.,1.),(1.,1.),(1.,1.),(1.,1.),(1.,1.),(1.,1.),(1.,1.),(1.,1.),(1.,
1.),(1.,1.),(1.,1.),(1.,1.),(1.,1.),(1.,1.),(1.,1.),(1.,1.),(1.,1.),(1.,
1.),(1.,1.),(1.,1.),(1.,1.),(1.,1.),(1.,1.),(1.,1.),(1.,1.),(1.,1.),(1.,
1.),(1.,1.),(1.,1.),(1.,1.),(1.,1.),(1.,1.),(1.,1.),(1.,1.),(1.,1.),(1.,
1.),(1.,1.),(1.,1.),(1.,1.),(1.,1.),(1.,1.),(1.,1.),(1.,1.),(1.,1.),(1.,
1.),(1.,1.),(1.,1.),(1.,1.),(1.,1.),(1.,1.),(1.,1.),(1.,1.),(1.,1.),(1.,
1.),(1.,1.),(1.,1.),(1.,1.),(1.,1.),(1.,1.),(1.,1.),(1.,1.),(1.,1.),(1.,
1.),(1.,1.)))
REPRESENTATION_ITEM('')
SURFACE()
);
#49=(
BOUNDED_SURFACE()
B_SPLINE_SURFACE(5,1,((#37940,#37941),(#37942,#37943),(#37944,#37945),(#37946,
#37947),(#37948,#37949),(#37950,#37951),(#37952,#37953),(#37954,#37955),
(#37956,#37957),(#37958,#37959),(#37960,#37961),(#37962,#37963),(#37964,
#37965),(#37966,#37967),(#37968,#37969),(#37970,#37971),(#37972,#37973),
(#37974,#37975),(#37976,#37977),(#37978,#37979),(#37980,#37981),(#37982,
#37983),(#37984,#37985),(#37986,#37987),(#37988,#37989),(#37990,#37991),
(#37992,#37993),(#37994,#37995),(#37996,#37997),(#37998,#37999),(#38000,
#38001),(#38002,#38003),(#38004,#38005),(#38006,#38007),(#38008,#38009),
(#38010,#38011),(#38012,#38013),(#38014,#38015),(#38016,#38017),(#38018,
#38019),(#38020,#38021),(#38022,#38023),(#38024,#38025),(#38026,#38027),
(#38028,#38029),(#38030,#38031),(#38032,#38033),(#38034,#38035),(#38036,
#38037),(#38038,#38039),(#38040,#38041),(#38042,#38043),(#38044,#38045),
(#38046,#38047),(#38048,#38049),(#38050,#38051),(#38052,#38053),(#38054,
#38055),(#38056,#38057),(#38058,#38059),(#38060,#38061),(#38062,#38063),
(#38064,#38065),(#38066,#38067),(#38068,#38069),(#38070,#38071),(#38072,
#38073),(#38074,#38075),(#38076,#38077),(#38078,#38079)),.UNSPECIFIED.,
 .F.,.F.,.F.)
B_SPLINE_SURFACE_WITH_KNOTS((6,1,1,1,1,1,1,1,1,1,1,1,1,1,1,1,1,1,1,1,1,
1,1,1,1,1,1,1,1,1,1,1,1,1,1,1,1,1,1,1,1,1,1,1,1,1,1,1,1,1,1,1,1,1,1,1,1,
1,1,1,1,1,1,1,1,6),(2,2),(-1.,-0.984615384615383,-0.969230769230768,-0.953846153846152,
-0.938461538461537,-0.923076923076922,-0.907692307692306,-0.892307692307691,
-0.876923076923076,-0.86153846153846,-0.846153846153845,-0.83076923076923,
-0.815384615384614,-0.799999999999999,-0.784615384615384,-0.769230769230768,
-0.753846153846153,-0.738461538461538,-0.723076923076922,-0.707692307692307,
-0.692307692307692,-0.676923076923076,-0.661538461538461,-0.646153846153846,
-0.63076923076923,-0.615384615384615,-0.6,-0.584615384615384,-0.569230769230769,
-0.553846153846154,-0.538461538461538,-0.523076923076923,-0.507692307692308,
-0.492307692307692,-0.476923076923077,-0.461538461538462,-0.446153846153846,
-0.430769230769231,-0.415384615384615,-0.4,-0.384615384615385,-0.369230769230769,
-0.353846153846154,-0.338461538461538,-0.323076923076923,-0.307692307692308,
-0.292307692307692,-0.276923076923077,-0.261538461538462,-0.246153846153846,
-0.230769230769231,-0.215384615384615,-0.2,-0.184615384615385,-0.169230769230769,
-0.153846153846154,-0.138461538461538,-0.123076923076923,-0.107692307692308,
-0.0923076923076923,-0.0769230769230769,-0.0615384615384615,-0.0461538461538462,
-0.0307692307692308,-0.0153846153846154,0.),(-1.,1.),.UNSPECIFIED.)
GEOMETRIC_REPRESENTATION_ITEM()
RATIONAL_B_SPLINE_SURFACE(((1.,1.),(1.,1.),(1.,1.),(1.,1.),(1.,1.),(1.,
1.),(1.,1.),(1.,1.),(1.,1.),(1.,1.),(1.,1.),(1.,1.),(1.,1.),(1.,1.),(1.,
1.),(1.,1.),(1.,1.),(1.,1.),(1.,1.),(1.,1.),(1.,1.),(1.,1.),(1.,1.),(1.,
1.),(1.,1.),(1.,1.),(1.,1.),(1.,1.),(1.,1.),(1.,1.),(1.,1.),(1.,1.),(1.,
1.),(1.,1.),(1.,1.),(1.,1.),(1.,1.),(1.,1.),(1.,1.),(1.,1.),(1.,1.),(1.,
1.),(1.,1.),(1.,1.),(1.,1.),(1.,1.),(1.,1.),(1.,1.),(1.,1.),(1.,1.),(1.,
1.),(1.,1.),(1.,1.),(1.,1.),(1.,1.),(1.,1.),(1.,1.),(1.,1.),(1.,1.),(1.,
1.),(1.,1.),(1.,1.),(1.,1.),(1.,1.),(1.,1.),(1.,1.),(1.,1.),(1.,1.),(1.,
1.),(1.,1.)))
REPRESENTATION_ITEM('')
SURFACE()
);
#50=(
BOUNDED_SURFACE()
B_SPLINE_SURFACE(5,1,((#38156,#38157),(#38158,#38159),(#38160,#38161),(#38162,
#38163),(#38164,#38165),(#38166,#38167),(#38168,#38169),(#38170,#38171),
(#38172,#38173),(#38174,#38175),(#38176,#38177),(#38178,#38179),(#38180,
#38181),(#38182,#38183),(#38184,#38185),(#38186,#38187),(#38188,#38189),
(#38190,#38191),(#38192,#38193),(#38194,#38195),(#38196,#38197),(#38198,
#38199),(#38200,#38201),(#38202,#38203),(#38204,#38205),(#38206,#38207),
(#38208,#38209),(#38210,#38211),(#38212,#38213),(#38214,#38215),(#38216,
#38217),(#38218,#38219),(#38220,#38221),(#38222,#38223),(#38224,#38225),
(#38226,#38227),(#38228,#38229),(#38230,#38231),(#38232,#38233),(#38234,
#38235),(#38236,#38237),(#38238,#38239),(#38240,#38241),(#38242,#38243),
(#38244,#38245),(#38246,#38247),(#38248,#38249),(#38250,#38251),(#38252,
#38253),(#38254,#38255),(#38256,#38257),(#38258,#38259),(#38260,#38261),
(#38262,#38263),(#38264,#38265),(#38266,#38267),(#38268,#38269),(#38270,
#38271),(#38272,#38273),(#38274,#38275),(#38276,#38277),(#38278,#38279),
(#38280,#38281),(#38282,#38283),(#38284,#38285),(#38286,#38287),(#38288,
#38289),(#38290,#38291),(#38292,#38293),(#38294,#38295)),.UNSPECIFIED.,
 .F.,.F.,.F.)
B_SPLINE_SURFACE_WITH_KNOTS((6,1,1,1,1,1,1,1,1,1,1,1,1,1,1,1,1,1,1,1,1,
1,1,1,1,1,1,1,1,1,1,1,1,1,1,1,1,1,1,1,1,1,1,1,1,1,1,1,1,1,1,1,1,1,1,1,1,
1,1,1,1,1,1,1,1,6),(2,2),(-1.,-0.984615384615383,-0.969230769230768,-0.953846153846152,
-0.938461538461537,-0.923076923076922,-0.907692307692306,-0.892307692307691,
-0.876923076923076,-0.86153846153846,-0.846153846153845,-0.83076923076923,
-0.815384615384614,-0.799999999999999,-0.784615384615384,-0.769230769230768,
-0.753846153846153,-0.738461538461538,-0.723076923076922,-0.707692307692307,
-0.692307692307692,-0.676923076923076,-0.661538461538461,-0.646153846153846,
-0.63076923076923,-0.615384615384615,-0.6,-0.584615384615384,-0.569230769230769,
-0.553846153846154,-0.538461538461538,-0.523076923076923,-0.507692307692308,
-0.492307692307692,-0.476923076923077,-0.461538461538462,-0.446153846153846,
-0.430769230769231,-0.415384615384615,-0.4,-0.384615384615385,-0.369230769230769,
-0.353846153846154,-0.338461538461538,-0.323076923076923,-0.307692307692308,
-0.292307692307692,-0.276923076923077,-0.261538461538462,-0.246153846153846,
-0.230769230769231,-0.215384615384615,-0.2,-0.184615384615385,-0.169230769230769,
-0.153846153846154,-0.138461538461538,-0.123076923076923,-0.107692307692308,
-0.0923076923076923,-0.0769230769230769,-0.0615384615384615,-0.0461538461538462,
-0.0307692307692308,-0.0153846153846154,0.),(-1.,1.),.UNSPECIFIED.)
GEOMETRIC_REPRESENTATION_ITEM()
RATIONAL_B_SPLINE_SURFACE(((1.,1.),(1.,1.),(1.,1.),(1.,1.),(1.,1.),(1.,
1.),(1.,1.),(1.,1.),(1.,1.),(1.,1.),(1.,1.),(1.,1.),(1.,1.),(1.,1.),(1.,
1.),(1.,1.),(1.,1.),(1.,1.),(1.,1.),(1.,1.),(1.,1.),(1.,1.),(1.,1.),(1.,
1.),(1.,1.),(1.,1.),(1.,1.),(1.,1.),(1.,1.),(1.,1.),(1.,1.),(1.,1.),(1.,
1.),(1.,1.),(1.,1.),(1.,1.),(1.,1.),(1.,1.),(1.,1.),(1.,1.),(1.,1.),(1.,
1.),(1.,1.),(1.,1.),(1.,1.),(1.,1.),(1.,1.),(1.,1.),(1.,1.),(1.,1.),(1.,
1.),(1.,1.),(1.,1.),(1.,1.),(1.,1.),(1.,1.),(1.,1.),(1.,1.),(1.,1.),(1.,
1.),(1.,1.),(1.,1.),(1.,1.),(1.,1.),(1.,1.),(1.,1.),(1.,1.),(1.,1.),(1.,
1.),(1.,1.)))
REPRESENTATION_ITEM('')
SURFACE()
);
#51=(
BOUNDED_SURFACE()
B_SPLINE_SURFACE(5,1,((#44627,#44628),(#44629,#44630),(#44631,#44632),(#44633,
#44634),(#44635,#44636),(#44637,#44638),(#44639,#44640),(#44641,#44642),
(#44643,#44644),(#44645,#44646),(#44647,#44648),(#44649,#44650),(#44651,
#44652),(#44653,#44654),(#44655,#44656),(#44657,#44658),(#44659,#44660),
(#44661,#44662),(#44663,#44664),(#44665,#44666),(#44667,#44668),(#44669,
#44670),(#44671,#44672),(#44673,#44674),(#44675,#44676),(#44677,#44678),
(#44679,#44680),(#44681,#44682),(#44683,#44684),(#44685,#44686),(#44687,
#44688),(#44689,#44690),(#44691,#44692),(#44693,#44694),(#44695,#44696),
(#44697,#44698),(#44699,#44700),(#44701,#44702),(#44703,#44704),(#44705,
#44706),(#44707,#44708),(#44709,#44710),(#44711,#44712),(#44713,#44714),
(#44715,#44716),(#44717,#44718),(#44719,#44720),(#44721,#44722),(#44723,
#44724),(#44725,#44726),(#44727,#44728),(#44729,#44730),(#44731,#44732),
(#44733,#44734),(#44735,#44736),(#44737,#44738),(#44739,#44740),(#44741,
#44742),(#44743,#44744),(#44745,#44746),(#44747,#44748),(#44749,#44750),
(#44751,#44752),(#44753,#44754),(#44755,#44756),(#44757,#44758),(#44759,
#44760),(#44761,#44762),(#44763,#44764),(#44765,#44766)),.UNSPECIFIED.,
 .F.,.F.,.F.)
B_SPLINE_SURFACE_WITH_KNOTS((6,1,1,1,1,1,1,1,1,1,1,1,1,1,1,1,1,1,1,1,1,
1,1,1,1,1,1,1,1,1,1,1,1,1,1,1,1,1,1,1,1,1,1,1,1,1,1,1,1,1,1,1,1,1,1,1,1,
1,1,1,1,1,1,1,1,6),(2,2),(-1.,-0.984615384615383,-0.969230769230768,-0.953846153846152,
-0.938461538461537,-0.923076923076922,-0.907692307692306,-0.892307692307691,
-0.876923076923076,-0.86153846153846,-0.846153846153845,-0.83076923076923,
-0.815384615384614,-0.799999999999999,-0.784615384615384,-0.769230769230768,
-0.753846153846153,-0.738461538461538,-0.723076923076922,-0.707692307692307,
-0.692307692307692,-0.676923076923076,-0.661538461538461,-0.646153846153846,
-0.63076923076923,-0.615384615384615,-0.6,-0.584615384615384,-0.569230769230769,
-0.553846153846154,-0.538461538461538,-0.523076923076923,-0.507692307692308,
-0.492307692307692,-0.476923076923077,-0.461538461538462,-0.446153846153846,
-0.430769230769231,-0.415384615384615,-0.4,-0.384615384615385,-0.369230769230769,
-0.353846153846154,-0.338461538461538,-0.323076923076923,-0.307692307692308,
-0.292307692307692,-0.276923076923077,-0.261538461538462,-0.246153846153846,
-0.230769230769231,-0.215384615384615,-0.2,-0.184615384615385,-0.169230769230769,
-0.153846153846154,-0.138461538461538,-0.123076923076923,-0.107692307692308,
-0.0923076923076923,-0.0769230769230769,-0.0615384615384615,-0.0461538461538462,
-0.0307692307692308,-0.0153846153846154,0.),(-1.,1.),.UNSPECIFIED.)
GEOMETRIC_REPRESENTATION_ITEM()
RATIONAL_B_SPLINE_SURFACE(((1.,1.),(1.,1.),(1.,1.),(1.,1.),(1.,1.),(1.,
1.),(1.,1.),(1.,1.),(1.,1.),(1.,1.),(1.,1.),(1.,1.),(1.,1.),(1.,1.),(1.,
1.),(1.,1.),(1.,1.),(1.,1.),(1.,1.),(1.,1.),(1.,1.),(1.,1.),(1.,1.),(1.,
1.),(1.,1.),(1.,1.),(1.,1.),(1.,1.),(1.,1.),(1.,1.),(1.,1.),(1.,1.),(1.,
1.),(1.,1.),(1.,1.),(1.,1.),(1.,1.),(1.,1.),(1.,1.),(1.,1.),(1.,1.),(1.,
1.),(1.,1.),(1.,1.),(1.,1.),(1.,1.),(1.,1.),(1.,1.),(1.,1.),(1.,1.),(1.,
1.),(1.,1.),(1.,1.),(1.,1.),(1.,1.),(1.,1.),(1.,1.),(1.,1.),(1.,1.),(1.,
1.),(1.,1.),(1.,1.),(1.,1.),(1.,1.),(1.,1.),(1.,1.),(1.,1.),(1.,1.),(1.,
1.),(1.,1.)))
REPRESENTATION_ITEM('')
SURFACE()
);
#52=(
BOUNDED_SURFACE()
B_SPLINE_SURFACE(5,1,((#44846,#44847),(#44848,#44849),(#44850,#44851),(#44852,
#44853),(#44854,#44855),(#44856,#44857),(#44858,#44859),(#44860,#44861),
(#44862,#44863),(#44864,#44865),(#44866,#44867),(#44868,#44869),(#44870,
#44871),(#44872,#44873),(#44874,#44875),(#44876,#44877),(#44878,#44879),
(#44880,#44881),(#44882,#44883),(#44884,#44885),(#44886,#44887),(#44888,
#44889),(#44890,#44891),(#44892,#44893),(#44894,#44895),(#44896,#44897),
(#44898,#44899),(#44900,#44901),(#44902,#44903),(#44904,#44905),(#44906,
#44907),(#44908,#44909),(#44910,#44911),(#44912,#44913),(#44914,#44915),
(#44916,#44917),(#44918,#44919),(#44920,#44921),(#44922,#44923),(#44924,
#44925),(#44926,#44927),(#44928,#44929),(#44930,#44931),(#44932,#44933),
(#44934,#44935),(#44936,#44937),(#44938,#44939),(#44940,#44941),(#44942,
#44943),(#44944,#44945),(#44946,#44947),(#44948,#44949),(#44950,#44951),
(#44952,#44953),(#44954,#44955),(#44956,#44957),(#44958,#44959),(#44960,
#44961),(#44962,#44963),(#44964,#44965),(#44966,#44967),(#44968,#44969),
(#44970,#44971),(#44972,#44973),(#44974,#44975),(#44976,#44977),(#44978,
#44979),(#44980,#44981),(#44982,#44983),(#44984,#44985)),.UNSPECIFIED.,
 .F.,.F.,.F.)
B_SPLINE_SURFACE_WITH_KNOTS((6,1,1,1,1,1,1,1,1,1,1,1,1,1,1,1,1,1,1,1,1,
1,1,1,1,1,1,1,1,1,1,1,1,1,1,1,1,1,1,1,1,1,1,1,1,1,1,1,1,1,1,1,1,1,1,1,1,
1,1,1,1,1,1,1,1,6),(2,2),(-1.,-0.984615384615383,-0.969230769230768,-0.953846153846152,
-0.938461538461537,-0.923076923076922,-0.907692307692306,-0.892307692307691,
-0.876923076923076,-0.86153846153846,-0.846153846153845,-0.83076923076923,
-0.815384615384614,-0.799999999999999,-0.784615384615384,-0.769230769230768,
-0.753846153846153,-0.738461538461538,-0.723076923076922,-0.707692307692307,
-0.692307692307692,-0.676923076923076,-0.661538461538461,-0.646153846153846,
-0.63076923076923,-0.615384615384615,-0.6,-0.584615384615384,-0.569230769230769,
-0.553846153846154,-0.538461538461538,-0.523076923076923,-0.507692307692308,
-0.492307692307692,-0.476923076923077,-0.461538461538462,-0.446153846153846,
-0.430769230769231,-0.415384615384615,-0.4,-0.384615384615385,-0.369230769230769,
-0.353846153846154,-0.338461538461538,-0.323076923076923,-0.307692307692308,
-0.292307692307692,-0.276923076923077,-0.261538461538462,-0.246153846153846,
-0.230769230769231,-0.215384615384615,-0.2,-0.184615384615385,-0.169230769230769,
-0.153846153846154,-0.138461538461538,-0.123076923076923,-0.107692307692308,
-0.0923076923076923,-0.0769230769230769,-0.0615384615384615,-0.0461538461538462,
-0.0307692307692308,-0.0153846153846154,0.),(-1.,1.),.UNSPECIFIED.)
GEOMETRIC_REPRESENTATION_ITEM()
RATIONAL_B_SPLINE_SURFACE(((1.,1.),(1.,1.),(1.,1.),(1.,1.),(1.,1.),(1.,
1.),(1.,1.),(1.,1.),(1.,1.),(1.,1.),(1.,1.),(1.,1.),(1.,1.),(1.,1.),(1.,
1.),(1.,1.),(1.,1.),(1.,1.),(1.,1.),(1.,1.),(1.,1.),(1.,1.),(1.,1.),(1.,
1.),(1.,1.),(1.,1.),(1.,1.),(1.,1.),(1.,1.),(1.,1.),(1.,1.),(1.,1.),(1.,
1.),(1.,1.),(1.,1.),(1.,1.),(1.,1.),(1.,1.),(1.,1.),(1.,1.),(1.,1.),(1.,
1.),(1.,1.),(1.,1.),(1.,1.),(1.,1.),(1.,1.),(1.,1.),(1.,1.),(1.,1.),(1.,
1.),(1.,1.),(1.,1.),(1.,1.),(1.,1.),(1.,1.),(1.,1.),(1.,1.),(1.,1.),(1.,
1.),(1.,1.),(1.,1.),(1.,1.),(1.,1.),(1.,1.),(1.,1.),(1.,1.),(1.,1.),(1.,
1.),(1.,1.)))
REPRESENTATION_ITEM('')
SURFACE()
);
#53=(
BOUNDED_SURFACE()
B_SPLINE_SURFACE(5,1,((#45076,#45077),(#45078,#45079),(#45080,#45081),(#45082,
#45083),(#45084,#45085),(#45086,#45087),(#45088,#45089),(#45090,#45091),
(#45092,#45093),(#45094,#45095),(#45096,#45097),(#45098,#45099),(#45100,
#45101),(#45102,#45103),(#45104,#45105),(#45106,#45107),(#45108,#45109),
(#45110,#45111),(#45112,#45113),(#45114,#45115),(#45116,#45117),(#45118,
#45119),(#45120,#45121),(#45122,#45123),(#45124,#45125),(#45126,#45127),
(#45128,#45129),(#45130,#45131),(#45132,#45133),(#45134,#45135),(#45136,
#45137),(#45138,#45139),(#45140,#45141),(#45142,#45143),(#45144,#45145),
(#45146,#45147),(#45148,#45149),(#45150,#45151),(#45152,#45153),(#45154,
#45155),(#45156,#45157),(#45158,#45159),(#45160,#45161),(#45162,#45163),
(#45164,#45165),(#45166,#45167),(#45168,#45169),(#45170,#45171),(#45172,
#45173),(#45174,#45175),(#45176,#45177),(#45178,#45179),(#45180,#45181),
(#45182,#45183),(#45184,#45185),(#45186,#45187),(#45188,#45189),(#45190,
#45191),(#45192,#45193),(#45194,#45195),(#45196,#45197),(#45198,#45199),
(#45200,#45201),(#45202,#45203),(#45204,#45205),(#45206,#45207),(#45208,
#45209),(#45210,#45211),(#45212,#45213),(#45214,#45215)),.UNSPECIFIED.,
 .F.,.F.,.F.)
B_SPLINE_SURFACE_WITH_KNOTS((6,1,1,1,1,1,1,1,1,1,1,1,1,1,1,1,1,1,1,1,1,
1,1,1,1,1,1,1,1,1,1,1,1,1,1,1,1,1,1,1,1,1,1,1,1,1,1,1,1,1,1,1,1,1,1,1,1,
1,1,1,1,1,1,1,1,6),(2,2),(-1.,-0.984615384615383,-0.969230769230768,-0.953846153846152,
-0.938461538461537,-0.923076923076922,-0.907692307692306,-0.892307692307691,
-0.876923076923076,-0.86153846153846,-0.846153846153845,-0.83076923076923,
-0.815384615384614,-0.799999999999999,-0.784615384615384,-0.769230769230768,
-0.753846153846153,-0.738461538461538,-0.723076923076922,-0.707692307692307,
-0.692307692307692,-0.676923076923076,-0.661538461538461,-0.646153846153846,
-0.63076923076923,-0.615384615384615,-0.6,-0.584615384615384,-0.569230769230769,
-0.553846153846154,-0.538461538461538,-0.523076923076923,-0.507692307692308,
-0.492307692307692,-0.476923076923077,-0.461538461538462,-0.446153846153846,
-0.430769230769231,-0.415384615384615,-0.4,-0.384615384615385,-0.369230769230769,
-0.353846153846154,-0.338461538461538,-0.323076923076923,-0.307692307692308,
-0.292307692307692,-0.276923076923077,-0.261538461538462,-0.246153846153846,
-0.230769230769231,-0.215384615384615,-0.2,-0.184615384615385,-0.169230769230769,
-0.153846153846154,-0.138461538461538,-0.123076923076923,-0.107692307692308,
-0.0923076923076923,-0.0769230769230769,-0.0615384615384615,-0.0461538461538462,
-0.0307692307692308,-0.0153846153846154,0.),(-1.,1.),.UNSPECIFIED.)
GEOMETRIC_REPRESENTATION_ITEM()
RATIONAL_B_SPLINE_SURFACE(((1.,1.),(1.,1.),(1.,1.),(1.,1.),(1.,1.),(1.,
1.),(1.,1.),(1.,1.),(1.,1.),(1.,1.),(1.,1.),(1.,1.),(1.,1.),(1.,1.),(1.,
1.),(1.,1.),(1.,1.),(1.,1.),(1.,1.),(1.,1.),(1.,1.),(1.,1.),(1.,1.),(1.,
1.),(1.,1.),(1.,1.),(1.,1.),(1.,1.),(1.,1.),(1.,1.),(1.,1.),(1.,1.),(1.,
1.),(1.,1.),(1.,1.),(1.,1.),(1.,1.),(1.,1.),(1.,1.),(1.,1.),(1.,1.),(1.,
1.),(1.,1.),(1.,1.),(1.,1.),(1.,1.),(1.,1.),(1.,1.),(1.,1.),(1.,1.),(1.,
1.),(1.,1.),(1.,1.),(1.,1.),(1.,1.),(1.,1.),(1.,1.),(1.,1.),(1.,1.),(1.,
1.),(1.,1.),(1.,1.),(1.,1.),(1.,1.),(1.,1.),(1.,1.),(1.,1.),(1.,1.),(1.,
1.),(1.,1.)))
REPRESENTATION_ITEM('')
SURFACE()
);
#54=(
BOUNDED_SURFACE()
B_SPLINE_SURFACE(5,1,((#45288,#45289),(#45290,#45291),(#45292,#45293),(#45294,
#45295),(#45296,#45297),(#45298,#45299),(#45300,#45301),(#45302,#45303),
(#45304,#45305),(#45306,#45307),(#45308,#45309),(#45310,#45311),(#45312,
#45313),(#45314,#45315),(#45316,#45317),(#45318,#45319),(#45320,#45321),
(#45322,#45323),(#45324,#45325),(#45326,#45327),(#45328,#45329),(#45330,
#45331),(#45332,#45333),(#45334,#45335),(#45336,#45337),(#45338,#45339),
(#45340,#45341),(#45342,#45343),(#45344,#45345),(#45346,#45347),(#45348,
#45349),(#45350,#45351),(#45352,#45353),(#45354,#45355),(#45356,#45357),
(#45358,#45359),(#45360,#45361),(#45362,#45363),(#45364,#45365),(#45366,
#45367),(#45368,#45369),(#45370,#45371),(#45372,#45373),(#45374,#45375),
(#45376,#45377),(#45378,#45379),(#45380,#45381),(#45382,#45383),(#45384,
#45385),(#45386,#45387),(#45388,#45389),(#45390,#45391),(#45392,#45393),
(#45394,#45395),(#45396,#45397),(#45398,#45399),(#45400,#45401),(#45402,
#45403),(#45404,#45405),(#45406,#45407),(#45408,#45409),(#45410,#45411),
(#45412,#45413),(#45414,#45415),(#45416,#45417),(#45418,#45419),(#45420,
#45421),(#45422,#45423),(#45424,#45425),(#45426,#45427)),.UNSPECIFIED.,
 .F.,.F.,.F.)
B_SPLINE_SURFACE_WITH_KNOTS((6,1,1,1,1,1,1,1,1,1,1,1,1,1,1,1,1,1,1,1,1,
1,1,1,1,1,1,1,1,1,1,1,1,1,1,1,1,1,1,1,1,1,1,1,1,1,1,1,1,1,1,1,1,1,1,1,1,
1,1,1,1,1,1,1,1,6),(2,2),(-1.,-0.984615384615383,-0.969230769230768,-0.953846153846152,
-0.938461538461537,-0.923076923076922,-0.907692307692306,-0.892307692307691,
-0.876923076923076,-0.86153846153846,-0.846153846153845,-0.83076923076923,
-0.815384615384614,-0.799999999999999,-0.784615384615384,-0.769230769230768,
-0.753846153846153,-0.738461538461538,-0.723076923076922,-0.707692307692307,
-0.692307692307692,-0.676923076923076,-0.661538461538461,-0.646153846153846,
-0.63076923076923,-0.615384615384615,-0.6,-0.584615384615384,-0.569230769230769,
-0.553846153846154,-0.538461538461538,-0.523076923076923,-0.507692307692308,
-0.492307692307692,-0.476923076923077,-0.461538461538462,-0.446153846153846,
-0.430769230769231,-0.415384615384615,-0.4,-0.384615384615385,-0.369230769230769,
-0.353846153846154,-0.338461538461538,-0.323076923076923,-0.307692307692308,
-0.292307692307692,-0.276923076923077,-0.261538461538462,-0.246153846153846,
-0.230769230769231,-0.215384615384615,-0.2,-0.184615384615385,-0.169230769230769,
-0.153846153846154,-0.138461538461538,-0.123076923076923,-0.107692307692308,
-0.0923076923076923,-0.0769230769230769,-0.0615384615384615,-0.0461538461538462,
-0.0307692307692308,-0.0153846153846154,0.),(-1.,1.),.UNSPECIFIED.)
GEOMETRIC_REPRESENTATION_ITEM()
RATIONAL_B_SPLINE_SURFACE(((1.,1.),(1.,1.),(1.,1.),(1.,1.),(1.,1.),(1.,
1.),(1.,1.),(1.,1.),(1.,1.),(1.,1.),(1.,1.),(1.,1.),(1.,1.),(1.,1.),(1.,
1.),(1.,1.),(1.,1.),(1.,1.),(1.,1.),(1.,1.),(1.,1.),(1.,1.),(1.,1.),(1.,
1.),(1.,1.),(1.,1.),(1.,1.),(1.,1.),(1.,1.),(1.,1.),(1.,1.),(1.,1.),(1.,
1.),(1.,1.),(1.,1.),(1.,1.),(1.,1.),(1.,1.),(1.,1.),(1.,1.),(1.,1.),(1.,
1.),(1.,1.),(1.,1.),(1.,1.),(1.,1.),(1.,1.),(1.,1.),(1.,1.),(1.,1.),(1.,
1.),(1.,1.),(1.,1.),(1.,1.),(1.,1.),(1.,1.),(1.,1.),(1.,1.),(1.,1.),(1.,
1.),(1.,1.),(1.,1.),(1.,1.),(1.,1.),(1.,1.),(1.,1.),(1.,1.),(1.,1.),(1.,
1.),(1.,1.)))
REPRESENTATION_ITEM('')
SURFACE()
);
#55=(
BOUNDED_SURFACE()
B_SPLINE_SURFACE(5,1,((#45518,#45519),(#45520,#45521),(#45522,#45523),(#45524,
#45525),(#45526,#45527),(#45528,#45529),(#45530,#45531),(#45532,#45533),
(#45534,#45535),(#45536,#45537),(#45538,#45539),(#45540,#45541),(#45542,
#45543),(#45544,#45545),(#45546,#45547),(#45548,#45549),(#45550,#45551),
(#45552,#45553),(#45554,#45555),(#45556,#45557),(#45558,#45559),(#45560,
#45561),(#45562,#45563),(#45564,#45565),(#45566,#45567),(#45568,#45569),
(#45570,#45571),(#45572,#45573),(#45574,#45575),(#45576,#45577),(#45578,
#45579),(#45580,#45581),(#45582,#45583),(#45584,#45585),(#45586,#45587),
(#45588,#45589),(#45590,#45591),(#45592,#45593),(#45594,#45595),(#45596,
#45597),(#45598,#45599),(#45600,#45601),(#45602,#45603),(#45604,#45605),
(#45606,#45607),(#45608,#45609),(#45610,#45611),(#45612,#45613),(#45614,
#45615),(#45616,#45617),(#45618,#45619),(#45620,#45621),(#45622,#45623),
(#45624,#45625),(#45626,#45627),(#45628,#45629),(#45630,#45631),(#45632,
#45633),(#45634,#45635),(#45636,#45637),(#45638,#45639),(#45640,#45641),
(#45642,#45643),(#45644,#45645),(#45646,#45647),(#45648,#45649),(#45650,
#45651),(#45652,#45653),(#45654,#45655),(#45656,#45657)),.UNSPECIFIED.,
 .F.,.F.,.F.)
B_SPLINE_SURFACE_WITH_KNOTS((6,1,1,1,1,1,1,1,1,1,1,1,1,1,1,1,1,1,1,1,1,
1,1,1,1,1,1,1,1,1,1,1,1,1,1,1,1,1,1,1,1,1,1,1,1,1,1,1,1,1,1,1,1,1,1,1,1,
1,1,1,1,1,1,1,1,6),(2,2),(-1.,-0.984615384615383,-0.969230769230768,-0.953846153846152,
-0.938461538461537,-0.923076923076922,-0.907692307692306,-0.892307692307691,
-0.876923076923076,-0.86153846153846,-0.846153846153845,-0.83076923076923,
-0.815384615384614,-0.799999999999999,-0.784615384615384,-0.769230769230768,
-0.753846153846153,-0.738461538461538,-0.723076923076922,-0.707692307692307,
-0.692307692307692,-0.676923076923076,-0.661538461538461,-0.646153846153846,
-0.63076923076923,-0.615384615384615,-0.6,-0.584615384615384,-0.569230769230769,
-0.553846153846154,-0.538461538461538,-0.523076923076923,-0.507692307692308,
-0.492307692307692,-0.476923076923077,-0.461538461538462,-0.446153846153846,
-0.430769230769231,-0.415384615384615,-0.4,-0.384615384615385,-0.369230769230769,
-0.353846153846154,-0.338461538461538,-0.323076923076923,-0.307692307692308,
-0.292307692307692,-0.276923076923077,-0.261538461538462,-0.246153846153846,
-0.230769230769231,-0.215384615384615,-0.2,-0.184615384615385,-0.169230769230769,
-0.153846153846154,-0.138461538461538,-0.123076923076923,-0.107692307692308,
-0.0923076923076923,-0.0769230769230769,-0.0615384615384615,-0.0461538461538462,
-0.0307692307692308,-0.0153846153846154,0.),(-1.,1.),.UNSPECIFIED.)
GEOMETRIC_REPRESENTATION_ITEM()
RATIONAL_B_SPLINE_SURFACE(((1.,1.),(1.,1.),(1.,1.),(1.,1.),(1.,1.),(1.,
1.),(1.,1.),(1.,1.),(1.,1.),(1.,1.),(1.,1.),(1.,1.),(1.,1.),(1.,1.),(1.,
1.),(1.,1.),(1.,1.),(1.,1.),(1.,1.),(1.,1.),(1.,1.),(1.,1.),(1.,1.),(1.,
1.),(1.,1.),(1.,1.),(1.,1.),(1.,1.),(1.,1.),(1.,1.),(1.,1.),(1.,1.),(1.,
1.),(1.,1.),(1.,1.),(1.,1.),(1.,1.),(1.,1.),(1.,1.),(1.,1.),(1.,1.),(1.,
1.),(1.,1.),(1.,1.),(1.,1.),(1.,1.),(1.,1.),(1.,1.),(1.,1.),(1.,1.),(1.,
1.),(1.,1.),(1.,1.),(1.,1.),(1.,1.),(1.,1.),(1.,1.),(1.,1.),(1.,1.),(1.,
1.),(1.,1.),(1.,1.),(1.,1.),(1.,1.),(1.,1.),(1.,1.),(1.,1.),(1.,1.),(1.,
1.),(1.,1.)))
REPRESENTATION_ITEM('')
SURFACE()
);
#56=(
BOUNDED_SURFACE()
B_SPLINE_SURFACE(5,1,((#45730,#45731),(#45732,#45733),(#45734,#45735),(#45736,
#45737),(#45738,#45739),(#45740,#45741),(#45742,#45743),(#45744,#45745),
(#45746,#45747),(#45748,#45749),(#45750,#45751),(#45752,#45753),(#45754,
#45755),(#45756,#45757),(#45758,#45759),(#45760,#45761),(#45762,#45763),
(#45764,#45765),(#45766,#45767),(#45768,#45769),(#45770,#45771),(#45772,
#45773),(#45774,#45775),(#45776,#45777),(#45778,#45779),(#45780,#45781),
(#45782,#45783),(#45784,#45785),(#45786,#45787),(#45788,#45789),(#45790,
#45791),(#45792,#45793),(#45794,#45795),(#45796,#45797),(#45798,#45799),
(#45800,#45801),(#45802,#45803),(#45804,#45805),(#45806,#45807),(#45808,
#45809),(#45810,#45811),(#45812,#45813),(#45814,#45815),(#45816,#45817),
(#45818,#45819),(#45820,#45821),(#45822,#45823),(#45824,#45825),(#45826,
#45827),(#45828,#45829),(#45830,#45831),(#45832,#45833),(#45834,#45835),
(#45836,#45837),(#45838,#45839),(#45840,#45841),(#45842,#45843),(#45844,
#45845),(#45846,#45847),(#45848,#45849),(#45850,#45851),(#45852,#45853),
(#45854,#45855),(#45856,#45857),(#45858,#45859),(#45860,#45861),(#45862,
#45863),(#45864,#45865),(#45866,#45867),(#45868,#45869)),.UNSPECIFIED.,
 .F.,.F.,.F.)
B_SPLINE_SURFACE_WITH_KNOTS((6,1,1,1,1,1,1,1,1,1,1,1,1,1,1,1,1,1,1,1,1,
1,1,1,1,1,1,1,1,1,1,1,1,1,1,1,1,1,1,1,1,1,1,1,1,1,1,1,1,1,1,1,1,1,1,1,1,
1,1,1,1,1,1,1,1,6),(2,2),(-1.,-0.984615384615383,-0.969230769230768,-0.953846153846152,
-0.938461538461537,-0.923076923076922,-0.907692307692306,-0.892307692307691,
-0.876923076923076,-0.86153846153846,-0.846153846153845,-0.83076923076923,
-0.815384615384614,-0.799999999999999,-0.784615384615384,-0.769230769230768,
-0.753846153846153,-0.738461538461538,-0.723076923076922,-0.707692307692307,
-0.692307692307692,-0.676923076923076,-0.661538461538461,-0.646153846153846,
-0.63076923076923,-0.615384615384615,-0.6,-0.584615384615384,-0.569230769230769,
-0.553846153846154,-0.538461538461538,-0.523076923076923,-0.507692307692308,
-0.492307692307692,-0.476923076923077,-0.461538461538462,-0.446153846153846,
-0.430769230769231,-0.415384615384615,-0.4,-0.384615384615385,-0.369230769230769,
-0.353846153846154,-0.338461538461538,-0.323076923076923,-0.307692307692308,
-0.292307692307692,-0.276923076923077,-0.261538461538462,-0.246153846153846,
-0.230769230769231,-0.215384615384615,-0.2,-0.184615384615385,-0.169230769230769,
-0.153846153846154,-0.138461538461538,-0.123076923076923,-0.107692307692308,
-0.0923076923076923,-0.0769230769230769,-0.0615384615384615,-0.0461538461538462,
-0.0307692307692308,-0.0153846153846154,0.),(-1.,1.),.UNSPECIFIED.)
GEOMETRIC_REPRESENTATION_ITEM()
RATIONAL_B_SPLINE_SURFACE(((1.,1.),(1.,1.),(1.,1.),(1.,1.),(1.,1.),(1.,
1.),(1.,1.),(1.,1.),(1.,1.),(1.,1.),(1.,1.),(1.,1.),(1.,1.),(1.,1.),(1.,
1.),(1.,1.),(1.,1.),(1.,1.),(1.,1.),(1.,1.),(1.,1.),(1.,1.),(1.,1.),(1.,
1.),(1.,1.),(1.,1.),(1.,1.),(1.,1.),(1.,1.),(1.,1.),(1.,1.),(1.,1.),(1.,
1.),(1.,1.),(1.,1.),(1.,1.),(1.,1.),(1.,1.),(1.,1.),(1.,1.),(1.,1.),(1.,
1.),(1.,1.),(1.,1.),(1.,1.),(1.,1.),(1.,1.),(1.,1.),(1.,1.),(1.,1.),(1.,
1.),(1.,1.),(1.,1.),(1.,1.),(1.,1.),(1.,1.),(1.,1.),(1.,1.),(1.,1.),(1.,
1.),(1.,1.),(1.,1.),(1.,1.),(1.,1.),(1.,1.),(1.,1.),(1.,1.),(1.,1.),(1.,
1.),(1.,1.)))
REPRESENTATION_ITEM('')
SURFACE()
);
#57=(
BOUNDED_SURFACE()
B_SPLINE_SURFACE(5,1,((#45960,#45961),(#45962,#45963),(#45964,#45965),(#45966,
#45967),(#45968,#45969),(#45970,#45971),(#45972,#45973),(#45974,#45975),
(#45976,#45977),(#45978,#45979),(#45980,#45981),(#45982,#45983),(#45984,
#45985),(#45986,#45987),(#45988,#45989),(#45990,#45991),(#45992,#45993),
(#45994,#45995),(#45996,#45997),(#45998,#45999),(#46000,#46001),(#46002,
#46003),(#46004,#46005),(#46006,#46007),(#46008,#46009),(#46010,#46011),
(#46012,#46013),(#46014,#46015),(#46016,#46017),(#46018,#46019),(#46020,
#46021),(#46022,#46023),(#46024,#46025),(#46026,#46027),(#46028,#46029),
(#46030,#46031),(#46032,#46033),(#46034,#46035),(#46036,#46037),(#46038,
#46039),(#46040,#46041),(#46042,#46043),(#46044,#46045),(#46046,#46047),
(#46048,#46049),(#46050,#46051),(#46052,#46053),(#46054,#46055),(#46056,
#46057),(#46058,#46059),(#46060,#46061),(#46062,#46063),(#46064,#46065),
(#46066,#46067),(#46068,#46069),(#46070,#46071),(#46072,#46073),(#46074,
#46075),(#46076,#46077),(#46078,#46079),(#46080,#46081),(#46082,#46083),
(#46084,#46085),(#46086,#46087),(#46088,#46089),(#46090,#46091),(#46092,
#46093),(#46094,#46095),(#46096,#46097),(#46098,#46099)),.UNSPECIFIED.,
 .F.,.F.,.F.)
B_SPLINE_SURFACE_WITH_KNOTS((6,1,1,1,1,1,1,1,1,1,1,1,1,1,1,1,1,1,1,1,1,
1,1,1,1,1,1,1,1,1,1,1,1,1,1,1,1,1,1,1,1,1,1,1,1,1,1,1,1,1,1,1,1,1,1,1,1,
1,1,1,1,1,1,1,1,6),(2,2),(-1.,-0.984615384615383,-0.969230769230768,-0.953846153846152,
-0.938461538461537,-0.923076923076922,-0.907692307692306,-0.892307692307691,
-0.876923076923076,-0.86153846153846,-0.846153846153845,-0.83076923076923,
-0.815384615384614,-0.799999999999999,-0.784615384615384,-0.769230769230768,
-0.753846153846153,-0.738461538461538,-0.723076923076922,-0.707692307692307,
-0.692307692307692,-0.676923076923076,-0.661538461538461,-0.646153846153846,
-0.63076923076923,-0.615384615384615,-0.6,-0.584615384615384,-0.569230769230769,
-0.553846153846154,-0.538461538461538,-0.523076923076923,-0.507692307692308,
-0.492307692307692,-0.476923076923077,-0.461538461538462,-0.446153846153846,
-0.430769230769231,-0.415384615384615,-0.4,-0.384615384615385,-0.369230769230769,
-0.353846153846154,-0.338461538461538,-0.323076923076923,-0.307692307692308,
-0.292307692307692,-0.276923076923077,-0.261538461538462,-0.246153846153846,
-0.230769230769231,-0.215384615384615,-0.2,-0.184615384615385,-0.169230769230769,
-0.153846153846154,-0.138461538461538,-0.123076923076923,-0.107692307692308,
-0.0923076923076923,-0.0769230769230769,-0.0615384615384615,-0.0461538461538462,
-0.0307692307692308,-0.0153846153846154,0.),(-1.,1.),.UNSPECIFIED.)
GEOMETRIC_REPRESENTATION_ITEM()
RATIONAL_B_SPLINE_SURFACE(((1.,1.),(1.,1.),(1.,1.),(1.,1.),(1.,1.),(1.,
1.),(1.,1.),(1.,1.),(1.,1.),(1.,1.),(1.,1.),(1.,1.),(1.,1.),(1.,1.),(1.,
1.),(1.,1.),(1.,1.),(1.,1.),(1.,1.),(1.,1.),(1.,1.),(1.,1.),(1.,1.),(1.,
1.),(1.,1.),(1.,1.),(1.,1.),(1.,1.),(1.,1.),(1.,1.),(1.,1.),(1.,1.),(1.,
1.),(1.,1.),(1.,1.),(1.,1.),(1.,1.),(1.,1.),(1.,1.),(1.,1.),(1.,1.),(1.,
1.),(1.,1.),(1.,1.),(1.,1.),(1.,1.),(1.,1.),(1.,1.),(1.,1.),(1.,1.),(1.,
1.),(1.,1.),(1.,1.),(1.,1.),(1.,1.),(1.,1.),(1.,1.),(1.,1.),(1.,1.),(1.,
1.),(1.,1.),(1.,1.),(1.,1.),(1.,1.),(1.,1.),(1.,1.),(1.,1.),(1.,1.),(1.,
1.),(1.,1.)))
REPRESENTATION_ITEM('')
SURFACE()
);
#58=(
BOUNDED_SURFACE()
B_SPLINE_SURFACE(5,1,((#46172,#46173),(#46174,#46175),(#46176,#46177),(#46178,
#46179),(#46180,#46181),(#46182,#46183),(#46184,#46185),(#46186,#46187),
(#46188,#46189),(#46190,#46191),(#46192,#46193),(#46194,#46195),(#46196,
#46197),(#46198,#46199),(#46200,#46201),(#46202,#46203),(#46204,#46205),
(#46206,#46207),(#46208,#46209),(#46210,#46211),(#46212,#46213),(#46214,
#46215),(#46216,#46217),(#46218,#46219),(#46220,#46221),(#46222,#46223),
(#46224,#46225),(#46226,#46227),(#46228,#46229),(#46230,#46231),(#46232,
#46233),(#46234,#46235),(#46236,#46237),(#46238,#46239),(#46240,#46241),
(#46242,#46243),(#46244,#46245),(#46246,#46247),(#46248,#46249),(#46250,
#46251),(#46252,#46253),(#46254,#46255),(#46256,#46257),(#46258,#46259),
(#46260,#46261),(#46262,#46263),(#46264,#46265),(#46266,#46267),(#46268,
#46269),(#46270,#46271),(#46272,#46273),(#46274,#46275),(#46276,#46277),
(#46278,#46279),(#46280,#46281),(#46282,#46283),(#46284,#46285),(#46286,
#46287),(#46288,#46289),(#46290,#46291),(#46292,#46293),(#46294,#46295),
(#46296,#46297),(#46298,#46299),(#46300,#46301),(#46302,#46303),(#46304,
#46305),(#46306,#46307),(#46308,#46309),(#46310,#46311)),.UNSPECIFIED.,
 .F.,.F.,.F.)
B_SPLINE_SURFACE_WITH_KNOTS((6,1,1,1,1,1,1,1,1,1,1,1,1,1,1,1,1,1,1,1,1,
1,1,1,1,1,1,1,1,1,1,1,1,1,1,1,1,1,1,1,1,1,1,1,1,1,1,1,1,1,1,1,1,1,1,1,1,
1,1,1,1,1,1,1,1,6),(2,2),(-1.,-0.984615384615383,-0.969230769230768,-0.953846153846152,
-0.938461538461537,-0.923076923076922,-0.907692307692306,-0.892307692307691,
-0.876923076923076,-0.86153846153846,-0.846153846153845,-0.83076923076923,
-0.815384615384614,-0.799999999999999,-0.784615384615384,-0.769230769230768,
-0.753846153846153,-0.738461538461538,-0.723076923076922,-0.707692307692307,
-0.692307692307692,-0.676923076923076,-0.661538461538461,-0.646153846153846,
-0.63076923076923,-0.615384615384615,-0.6,-0.584615384615384,-0.569230769230769,
-0.553846153846154,-0.538461538461538,-0.523076923076923,-0.507692307692308,
-0.492307692307692,-0.476923076923077,-0.461538461538462,-0.446153846153846,
-0.430769230769231,-0.415384615384615,-0.4,-0.384615384615385,-0.369230769230769,
-0.353846153846154,-0.338461538461538,-0.323076923076923,-0.307692307692308,
-0.292307692307692,-0.276923076923077,-0.261538461538462,-0.246153846153846,
-0.230769230769231,-0.215384615384615,-0.2,-0.184615384615385,-0.169230769230769,
-0.153846153846154,-0.138461538461538,-0.123076923076923,-0.107692307692308,
-0.0923076923076923,-0.0769230769230769,-0.0615384615384615,-0.0461538461538462,
-0.0307692307692308,-0.0153846153846154,0.),(-1.,1.),.UNSPECIFIED.)
GEOMETRIC_REPRESENTATION_ITEM()
RATIONAL_B_SPLINE_SURFACE(((1.,1.),(1.,1.),(1.,1.),(1.,1.),(1.,1.),(1.,
1.),(1.,1.),(1.,1.),(1.,1.),(1.,1.),(1.,1.),(1.,1.),(1.,1.),(1.,1.),(1.,
1.),(1.,1.),(1.,1.),(1.,1.),(1.,1.),(1.,1.),(1.,1.),(1.,1.),(1.,1.),(1.,
1.),(1.,1.),(1.,1.),(1.,1.),(1.,1.),(1.,1.),(1.,1.),(1.,1.),(1.,1.),(1.,
1.),(1.,1.),(1.,1.),(1.,1.),(1.,1.),(1.,1.),(1.,1.),(1.,1.),(1.,1.),(1.,
1.),(1.,1.),(1.,1.),(1.,1.),(1.,1.),(1.,1.),(1.,1.),(1.,1.),(1.,1.),(1.,
1.),(1.,1.),(1.,1.),(1.,1.),(1.,1.),(1.,1.),(1.,1.),(1.,1.),(1.,1.),(1.,
1.),(1.,1.),(1.,1.),(1.,1.),(1.,1.),(1.,1.),(1.,1.),(1.,1.),(1.,1.),(1.,
1.),(1.,1.)))
REPRESENTATION_ITEM('')
SURFACE()
);
#59=(
BOUNDED_SURFACE()
B_SPLINE_SURFACE(5,1,((#46402,#46403),(#46404,#46405),(#46406,#46407),(#46408,
#46409),(#46410,#46411),(#46412,#46413),(#46414,#46415),(#46416,#46417),
(#46418,#46419),(#46420,#46421),(#46422,#46423),(#46424,#46425),(#46426,
#46427),(#46428,#46429),(#46430,#46431),(#46432,#46433),(#46434,#46435),
(#46436,#46437),(#46438,#46439),(#46440,#46441),(#46442,#46443),(#46444,
#46445),(#46446,#46447),(#46448,#46449),(#46450,#46451),(#46452,#46453),
(#46454,#46455),(#46456,#46457),(#46458,#46459),(#46460,#46461),(#46462,
#46463),(#46464,#46465),(#46466,#46467),(#46468,#46469),(#46470,#46471),
(#46472,#46473),(#46474,#46475),(#46476,#46477),(#46478,#46479),(#46480,
#46481),(#46482,#46483),(#46484,#46485),(#46486,#46487),(#46488,#46489),
(#46490,#46491),(#46492,#46493),(#46494,#46495),(#46496,#46497),(#46498,
#46499),(#46500,#46501),(#46502,#46503),(#46504,#46505),(#46506,#46507),
(#46508,#46509),(#46510,#46511),(#46512,#46513),(#46514,#46515),(#46516,
#46517),(#46518,#46519),(#46520,#46521),(#46522,#46523),(#46524,#46525),
(#46526,#46527),(#46528,#46529),(#46530,#46531),(#46532,#46533),(#46534,
#46535),(#46536,#46537),(#46538,#46539),(#46540,#46541)),.UNSPECIFIED.,
 .F.,.F.,.F.)
B_SPLINE_SURFACE_WITH_KNOTS((6,1,1,1,1,1,1,1,1,1,1,1,1,1,1,1,1,1,1,1,1,
1,1,1,1,1,1,1,1,1,1,1,1,1,1,1,1,1,1,1,1,1,1,1,1,1,1,1,1,1,1,1,1,1,1,1,1,
1,1,1,1,1,1,1,1,6),(2,2),(-1.,-0.984615384615383,-0.969230769230768,-0.953846153846152,
-0.938461538461537,-0.923076923076922,-0.907692307692306,-0.892307692307691,
-0.876923076923076,-0.86153846153846,-0.846153846153845,-0.83076923076923,
-0.815384615384614,-0.799999999999999,-0.784615384615384,-0.769230769230768,
-0.753846153846153,-0.738461538461538,-0.723076923076922,-0.707692307692307,
-0.692307692307692,-0.676923076923076,-0.661538461538461,-0.646153846153846,
-0.63076923076923,-0.615384615384615,-0.6,-0.584615384615384,-0.569230769230769,
-0.553846153846154,-0.538461538461538,-0.523076923076923,-0.507692307692308,
-0.492307692307692,-0.476923076923077,-0.461538461538462,-0.446153846153846,
-0.430769230769231,-0.415384615384615,-0.4,-0.384615384615385,-0.369230769230769,
-0.353846153846154,-0.338461538461538,-0.323076923076923,-0.307692307692308,
-0.292307692307692,-0.276923076923077,-0.261538461538462,-0.246153846153846,
-0.230769230769231,-0.215384615384615,-0.2,-0.184615384615385,-0.169230769230769,
-0.153846153846154,-0.138461538461538,-0.123076923076923,-0.107692307692308,
-0.0923076923076923,-0.0769230769230769,-0.0615384615384615,-0.0461538461538462,
-0.0307692307692308,-0.0153846153846154,0.),(-1.,1.),.UNSPECIFIED.)
GEOMETRIC_REPRESENTATION_ITEM()
RATIONAL_B_SPLINE_SURFACE(((1.,1.),(1.,1.),(1.,1.),(1.,1.),(1.,1.),(1.,
1.),(1.,1.),(1.,1.),(1.,1.),(1.,1.),(1.,1.),(1.,1.),(1.,1.),(1.,1.),(1.,
1.),(1.,1.),(1.,1.),(1.,1.),(1.,1.),(1.,1.),(1.,1.),(1.,1.),(1.,1.),(1.,
1.),(1.,1.),(1.,1.),(1.,1.),(1.,1.),(1.,1.),(1.,1.),(1.,1.),(1.,1.),(1.,
1.),(1.,1.),(1.,1.),(1.,1.),(1.,1.),(1.,1.),(1.,1.),(1.,1.),(1.,1.),(1.,
1.),(1.,1.),(1.,1.),(1.,1.),(1.,1.),(1.,1.),(1.,1.),(1.,1.),(1.,1.),(1.,
1.),(1.,1.),(1.,1.),(1.,1.),(1.,1.),(1.,1.),(1.,1.),(1.,1.),(1.,1.),(1.,
1.),(1.,1.),(1.,1.),(1.,1.),(1.,1.),(1.,1.),(1.,1.),(1.,1.),(1.,1.),(1.,
1.),(1.,1.)))
REPRESENTATION_ITEM('')
SURFACE()
);
#60=(
BOUNDED_SURFACE()
B_SPLINE_SURFACE(5,1,((#46614,#46615),(#46616,#46617),(#46618,#46619),(#46620,
#46621),(#46622,#46623),(#46624,#46625),(#46626,#46627),(#46628,#46629),
(#46630,#46631),(#46632,#46633),(#46634,#46635),(#46636,#46637),(#46638,
#46639),(#46640,#46641),(#46642,#46643),(#46644,#46645),(#46646,#46647),
(#46648,#46649),(#46650,#46651),(#46652,#46653),(#46654,#46655),(#46656,
#46657),(#46658,#46659),(#46660,#46661),(#46662,#46663),(#46664,#46665),
(#46666,#46667),(#46668,#46669),(#46670,#46671),(#46672,#46673),(#46674,
#46675),(#46676,#46677),(#46678,#46679),(#46680,#46681),(#46682,#46683),
(#46684,#46685),(#46686,#46687),(#46688,#46689),(#46690,#46691),(#46692,
#46693),(#46694,#46695),(#46696,#46697),(#46698,#46699),(#46700,#46701),
(#46702,#46703),(#46704,#46705),(#46706,#46707),(#46708,#46709),(#46710,
#46711),(#46712,#46713),(#46714,#46715),(#46716,#46717),(#46718,#46719),
(#46720,#46721),(#46722,#46723),(#46724,#46725),(#46726,#46727),(#46728,
#46729),(#46730,#46731),(#46732,#46733),(#46734,#46735),(#46736,#46737),
(#46738,#46739),(#46740,#46741),(#46742,#46743),(#46744,#46745),(#46746,
#46747),(#46748,#46749),(#46750,#46751),(#46752,#46753)),.UNSPECIFIED.,
 .F.,.F.,.F.)
B_SPLINE_SURFACE_WITH_KNOTS((6,1,1,1,1,1,1,1,1,1,1,1,1,1,1,1,1,1,1,1,1,
1,1,1,1,1,1,1,1,1,1,1,1,1,1,1,1,1,1,1,1,1,1,1,1,1,1,1,1,1,1,1,1,1,1,1,1,
1,1,1,1,1,1,1,1,6),(2,2),(-1.,-0.984615384615383,-0.969230769230768,-0.953846153846152,
-0.938461538461537,-0.923076923076922,-0.907692307692306,-0.892307692307691,
-0.876923076923076,-0.86153846153846,-0.846153846153845,-0.83076923076923,
-0.815384615384614,-0.799999999999999,-0.784615384615384,-0.769230769230768,
-0.753846153846153,-0.738461538461538,-0.723076923076922,-0.707692307692307,
-0.692307692307692,-0.676923076923076,-0.661538461538461,-0.646153846153846,
-0.63076923076923,-0.615384615384615,-0.6,-0.584615384615384,-0.569230769230769,
-0.553846153846154,-0.538461538461538,-0.523076923076923,-0.507692307692308,
-0.492307692307692,-0.476923076923077,-0.461538461538462,-0.446153846153846,
-0.430769230769231,-0.415384615384615,-0.4,-0.384615384615385,-0.369230769230769,
-0.353846153846154,-0.338461538461538,-0.323076923076923,-0.307692307692308,
-0.292307692307692,-0.276923076923077,-0.261538461538462,-0.246153846153846,
-0.230769230769231,-0.215384615384615,-0.2,-0.184615384615385,-0.169230769230769,
-0.153846153846154,-0.138461538461538,-0.123076923076923,-0.107692307692308,
-0.0923076923076923,-0.0769230769230769,-0.0615384615384615,-0.0461538461538462,
-0.0307692307692308,-0.0153846153846154,0.),(-1.,1.),.UNSPECIFIED.)
GEOMETRIC_REPRESENTATION_ITEM()
RATIONAL_B_SPLINE_SURFACE(((1.,1.),(1.,1.),(1.,1.),(1.,1.),(1.,1.),(1.,
1.),(1.,1.),(1.,1.),(1.,1.),(1.,1.),(1.,1.),(1.,1.),(1.,1.),(1.,1.),(1.,
1.),(1.,1.),(1.,1.),(1.,1.),(1.,1.),(1.,1.),(1.,1.),(1.,1.),(1.,1.),(1.,
1.),(1.,1.),(1.,1.),(1.,1.),(1.,1.),(1.,1.),(1.,1.),(1.,1.),(1.,1.),(1.,
1.),(1.,1.),(1.,1.),(1.,1.),(1.,1.),(1.,1.),(1.,1.),(1.,1.),(1.,1.),(1.,
1.),(1.,1.),(1.,1.),(1.,1.),(1.,1.),(1.,1.),(1.,1.),(1.,1.),(1.,1.),(1.,
1.),(1.,1.),(1.,1.),(1.,1.),(1.,1.),(1.,1.),(1.,1.),(1.,1.),(1.,1.),(1.,
1.),(1.,1.),(1.,1.),(1.,1.),(1.,1.),(1.,1.),(1.,1.),(1.,1.),(1.,1.),(1.,
1.),(1.,1.)))
REPRESENTATION_ITEM('')
SURFACE()
);
#61=(
BOUNDED_SURFACE()
B_SPLINE_SURFACE(5,1,((#46844,#46845),(#46846,#46847),(#46848,#46849),(#46850,
#46851),(#46852,#46853),(#46854,#46855),(#46856,#46857),(#46858,#46859),
(#46860,#46861),(#46862,#46863),(#46864,#46865),(#46866,#46867),(#46868,
#46869),(#46870,#46871),(#46872,#46873),(#46874,#46875),(#46876,#46877),
(#46878,#46879),(#46880,#46881),(#46882,#46883),(#46884,#46885),(#46886,
#46887),(#46888,#46889),(#46890,#46891),(#46892,#46893),(#46894,#46895),
(#46896,#46897),(#46898,#46899),(#46900,#46901),(#46902,#46903),(#46904,
#46905),(#46906,#46907),(#46908,#46909),(#46910,#46911),(#46912,#46913),
(#46914,#46915),(#46916,#46917),(#46918,#46919),(#46920,#46921),(#46922,
#46923),(#46924,#46925),(#46926,#46927),(#46928,#46929),(#46930,#46931),
(#46932,#46933),(#46934,#46935),(#46936,#46937),(#46938,#46939),(#46940,
#46941),(#46942,#46943),(#46944,#46945),(#46946,#46947),(#46948,#46949),
(#46950,#46951),(#46952,#46953),(#46954,#46955),(#46956,#46957),(#46958,
#46959),(#46960,#46961),(#46962,#46963),(#46964,#46965),(#46966,#46967),
(#46968,#46969),(#46970,#46971),(#46972,#46973),(#46974,#46975),(#46976,
#46977),(#46978,#46979),(#46980,#46981),(#46982,#46983)),.UNSPECIFIED.,
 .F.,.F.,.F.)
B_SPLINE_SURFACE_WITH_KNOTS((6,1,1,1,1,1,1,1,1,1,1,1,1,1,1,1,1,1,1,1,1,
1,1,1,1,1,1,1,1,1,1,1,1,1,1,1,1,1,1,1,1,1,1,1,1,1,1,1,1,1,1,1,1,1,1,1,1,
1,1,1,1,1,1,1,1,6),(2,2),(-1.,-0.984615384615383,-0.969230769230768,-0.953846153846152,
-0.938461538461537,-0.923076923076922,-0.907692307692306,-0.892307692307691,
-0.876923076923076,-0.86153846153846,-0.846153846153845,-0.83076923076923,
-0.815384615384614,-0.799999999999999,-0.784615384615384,-0.769230769230768,
-0.753846153846153,-0.738461538461538,-0.723076923076922,-0.707692307692307,
-0.692307692307692,-0.676923076923076,-0.661538461538461,-0.646153846153846,
-0.63076923076923,-0.615384615384615,-0.6,-0.584615384615384,-0.569230769230769,
-0.553846153846154,-0.538461538461538,-0.523076923076923,-0.507692307692308,
-0.492307692307692,-0.476923076923077,-0.461538461538462,-0.446153846153846,
-0.430769230769231,-0.415384615384615,-0.4,-0.384615384615385,-0.369230769230769,
-0.353846153846154,-0.338461538461538,-0.323076923076923,-0.307692307692308,
-0.292307692307692,-0.276923076923077,-0.261538461538462,-0.246153846153846,
-0.230769230769231,-0.215384615384615,-0.2,-0.184615384615385,-0.169230769230769,
-0.153846153846154,-0.138461538461538,-0.123076923076923,-0.107692307692308,
-0.0923076923076923,-0.0769230769230769,-0.0615384615384615,-0.0461538461538462,
-0.0307692307692308,-0.0153846153846154,0.),(-1.,1.),.UNSPECIFIED.)
GEOMETRIC_REPRESENTATION_ITEM()
RATIONAL_B_SPLINE_SURFACE(((1.,1.),(1.,1.),(1.,1.),(1.,1.),(1.,1.),(1.,
1.),(1.,1.),(1.,1.),(1.,1.),(1.,1.),(1.,1.),(1.,1.),(1.,1.),(1.,1.),(1.,
1.),(1.,1.),(1.,1.),(1.,1.),(1.,1.),(1.,1.),(1.,1.),(1.,1.),(1.,1.),(1.,
1.),(1.,1.),(1.,1.),(1.,1.),(1.,1.),(1.,1.),(1.,1.),(1.,1.),(1.,1.),(1.,
1.),(1.,1.),(1.,1.),(1.,1.),(1.,1.),(1.,1.),(1.,1.),(1.,1.),(1.,1.),(1.,
1.),(1.,1.),(1.,1.),(1.,1.),(1.,1.),(1.,1.),(1.,1.),(1.,1.),(1.,1.),(1.,
1.),(1.,1.),(1.,1.),(1.,1.),(1.,1.),(1.,1.),(1.,1.),(1.,1.),(1.,1.),(1.,
1.),(1.,1.),(1.,1.),(1.,1.),(1.,1.),(1.,1.),(1.,1.),(1.,1.),(1.,1.),(1.,
1.),(1.,1.)))
REPRESENTATION_ITEM('')
SURFACE()
);
#62=(
BOUNDED_SURFACE()
B_SPLINE_SURFACE(5,1,((#47056,#47057),(#47058,#47059),(#47060,#47061),(#47062,
#47063),(#47064,#47065),(#47066,#47067),(#47068,#47069),(#47070,#47071),
(#47072,#47073),(#47074,#47075),(#47076,#47077),(#47078,#47079),(#47080,
#47081),(#47082,#47083),(#47084,#47085),(#47086,#47087),(#47088,#47089),
(#47090,#47091),(#47092,#47093),(#47094,#47095),(#47096,#47097),(#47098,
#47099),(#47100,#47101),(#47102,#47103),(#47104,#47105),(#47106,#47107),
(#47108,#47109),(#47110,#47111),(#47112,#47113),(#47114,#47115),(#47116,
#47117),(#47118,#47119),(#47120,#47121),(#47122,#47123),(#47124,#47125),
(#47126,#47127),(#47128,#47129),(#47130,#47131),(#47132,#47133),(#47134,
#47135),(#47136,#47137),(#47138,#47139),(#47140,#47141),(#47142,#47143),
(#47144,#47145),(#47146,#47147),(#47148,#47149),(#47150,#47151),(#47152,
#47153),(#47154,#47155),(#47156,#47157),(#47158,#47159),(#47160,#47161),
(#47162,#47163),(#47164,#47165),(#47166,#47167),(#47168,#47169),(#47170,
#47171),(#47172,#47173),(#47174,#47175),(#47176,#47177),(#47178,#47179),
(#47180,#47181),(#47182,#47183),(#47184,#47185),(#47186,#47187),(#47188,
#47189),(#47190,#47191),(#47192,#47193),(#47194,#47195)),.UNSPECIFIED.,
 .F.,.F.,.F.)
B_SPLINE_SURFACE_WITH_KNOTS((6,1,1,1,1,1,1,1,1,1,1,1,1,1,1,1,1,1,1,1,1,
1,1,1,1,1,1,1,1,1,1,1,1,1,1,1,1,1,1,1,1,1,1,1,1,1,1,1,1,1,1,1,1,1,1,1,1,
1,1,1,1,1,1,1,1,6),(2,2),(-1.,-0.984615384615383,-0.969230769230768,-0.953846153846152,
-0.938461538461537,-0.923076923076922,-0.907692307692306,-0.892307692307691,
-0.876923076923076,-0.86153846153846,-0.846153846153845,-0.83076923076923,
-0.815384615384614,-0.799999999999999,-0.784615384615384,-0.769230769230768,
-0.753846153846153,-0.738461538461538,-0.723076923076922,-0.707692307692307,
-0.692307692307692,-0.676923076923076,-0.661538461538461,-0.646153846153846,
-0.63076923076923,-0.615384615384615,-0.6,-0.584615384615384,-0.569230769230769,
-0.553846153846154,-0.538461538461538,-0.523076923076923,-0.507692307692308,
-0.492307692307692,-0.476923076923077,-0.461538461538462,-0.446153846153846,
-0.430769230769231,-0.415384615384615,-0.4,-0.384615384615385,-0.369230769230769,
-0.353846153846154,-0.338461538461538,-0.323076923076923,-0.307692307692308,
-0.292307692307692,-0.276923076923077,-0.261538461538462,-0.246153846153846,
-0.230769230769231,-0.215384615384615,-0.2,-0.184615384615385,-0.169230769230769,
-0.153846153846154,-0.138461538461538,-0.123076923076923,-0.107692307692308,
-0.0923076923076923,-0.0769230769230769,-0.0615384615384615,-0.0461538461538462,
-0.0307692307692308,-0.0153846153846154,0.),(-1.,1.),.UNSPECIFIED.)
GEOMETRIC_REPRESENTATION_ITEM()
RATIONAL_B_SPLINE_SURFACE(((1.,1.),(1.,1.),(1.,1.),(1.,1.),(1.,1.),(1.,
1.),(1.,1.),(1.,1.),(1.,1.),(1.,1.),(1.,1.),(1.,1.),(1.,1.),(1.,1.),(1.,
1.),(1.,1.),(1.,1.),(1.,1.),(1.,1.),(1.,1.),(1.,1.),(1.,1.),(1.,1.),(1.,
1.),(1.,1.),(1.,1.),(1.,1.),(1.,1.),(1.,1.),(1.,1.),(1.,1.),(1.,1.),(1.,
1.),(1.,1.),(1.,1.),(1.,1.),(1.,1.),(1.,1.),(1.,1.),(1.,1.),(1.,1.),(1.,
1.),(1.,1.),(1.,1.),(1.,1.),(1.,1.),(1.,1.),(1.,1.),(1.,1.),(1.,1.),(1.,
1.),(1.,1.),(1.,1.),(1.,1.),(1.,1.),(1.,1.),(1.,1.),(1.,1.),(1.,1.),(1.,
1.),(1.,1.),(1.,1.),(1.,1.),(1.,1.),(1.,1.),(1.,1.),(1.,1.),(1.,1.),(1.,
1.),(1.,1.)))
REPRESENTATION_ITEM('')
SURFACE()
);
#63=(
BOUNDED_SURFACE()
B_SPLINE_SURFACE(5,1,((#47286,#47287),(#47288,#47289),(#47290,#47291),(#47292,
#47293),(#47294,#47295),(#47296,#47297),(#47298,#47299),(#47300,#47301),
(#47302,#47303),(#47304,#47305),(#47306,#47307),(#47308,#47309),(#47310,
#47311),(#47312,#47313),(#47314,#47315),(#47316,#47317),(#47318,#47319),
(#47320,#47321),(#47322,#47323),(#47324,#47325),(#47326,#47327),(#47328,
#47329),(#47330,#47331),(#47332,#47333),(#47334,#47335),(#47336,#47337),
(#47338,#47339),(#47340,#47341),(#47342,#47343),(#47344,#47345),(#47346,
#47347),(#47348,#47349),(#47350,#47351),(#47352,#47353),(#47354,#47355),
(#47356,#47357),(#47358,#47359),(#47360,#47361),(#47362,#47363),(#47364,
#47365),(#47366,#47367),(#47368,#47369),(#47370,#47371),(#47372,#47373),
(#47374,#47375),(#47376,#47377),(#47378,#47379),(#47380,#47381),(#47382,
#47383),(#47384,#47385),(#47386,#47387),(#47388,#47389),(#47390,#47391),
(#47392,#47393),(#47394,#47395),(#47396,#47397),(#47398,#47399),(#47400,
#47401),(#47402,#47403),(#47404,#47405),(#47406,#47407),(#47408,#47409),
(#47410,#47411),(#47412,#47413),(#47414,#47415),(#47416,#47417),(#47418,
#47419),(#47420,#47421),(#47422,#47423),(#47424,#47425)),.UNSPECIFIED.,
 .F.,.F.,.F.)
B_SPLINE_SURFACE_WITH_KNOTS((6,1,1,1,1,1,1,1,1,1,1,1,1,1,1,1,1,1,1,1,1,
1,1,1,1,1,1,1,1,1,1,1,1,1,1,1,1,1,1,1,1,1,1,1,1,1,1,1,1,1,1,1,1,1,1,1,1,
1,1,1,1,1,1,1,1,6),(2,2),(-1.,-0.984615384615383,-0.969230769230768,-0.953846153846152,
-0.938461538461537,-0.923076923076922,-0.907692307692306,-0.892307692307691,
-0.876923076923076,-0.86153846153846,-0.846153846153845,-0.83076923076923,
-0.815384615384614,-0.799999999999999,-0.784615384615384,-0.769230769230768,
-0.753846153846153,-0.738461538461538,-0.723076923076922,-0.707692307692307,
-0.692307692307692,-0.676923076923076,-0.661538461538461,-0.646153846153846,
-0.63076923076923,-0.615384615384615,-0.6,-0.584615384615384,-0.569230769230769,
-0.553846153846154,-0.538461538461538,-0.523076923076923,-0.507692307692308,
-0.492307692307692,-0.476923076923077,-0.461538461538462,-0.446153846153846,
-0.430769230769231,-0.415384615384615,-0.4,-0.384615384615385,-0.369230769230769,
-0.353846153846154,-0.338461538461538,-0.323076923076923,-0.307692307692308,
-0.292307692307692,-0.276923076923077,-0.261538461538462,-0.246153846153846,
-0.230769230769231,-0.215384615384615,-0.2,-0.184615384615385,-0.169230769230769,
-0.153846153846154,-0.138461538461538,-0.123076923076923,-0.107692307692308,
-0.0923076923076923,-0.0769230769230769,-0.0615384615384615,-0.0461538461538462,
-0.0307692307692308,-0.0153846153846154,0.),(-1.,1.),.UNSPECIFIED.)
GEOMETRIC_REPRESENTATION_ITEM()
RATIONAL_B_SPLINE_SURFACE(((1.,1.),(1.,1.),(1.,1.),(1.,1.),(1.,1.),(1.,
1.),(1.,1.),(1.,1.),(1.,1.),(1.,1.),(1.,1.),(1.,1.),(1.,1.),(1.,1.),(1.,
1.),(1.,1.),(1.,1.),(1.,1.),(1.,1.),(1.,1.),(1.,1.),(1.,1.),(1.,1.),(1.,
1.),(1.,1.),(1.,1.),(1.,1.),(1.,1.),(1.,1.),(1.,1.),(1.,1.),(1.,1.),(1.,
1.),(1.,1.),(1.,1.),(1.,1.),(1.,1.),(1.,1.),(1.,1.),(1.,1.),(1.,1.),(1.,
1.),(1.,1.),(1.,1.),(1.,1.),(1.,1.),(1.,1.),(1.,1.),(1.,1.),(1.,1.),(1.,
1.),(1.,1.),(1.,1.),(1.,1.),(1.,1.),(1.,1.),(1.,1.),(1.,1.),(1.,1.),(1.,
1.),(1.,1.),(1.,1.),(1.,1.),(1.,1.),(1.,1.),(1.,1.),(1.,1.),(1.,1.),(1.,
1.),(1.,1.)))
REPRESENTATION_ITEM('')
SURFACE()
);
#64=(
BOUNDED_SURFACE()
B_SPLINE_SURFACE(5,1,((#47498,#47499),(#47500,#47501),(#47502,#47503),(#47504,
#47505),(#47506,#47507),(#47508,#47509),(#47510,#47511),(#47512,#47513),
(#47514,#47515),(#47516,#47517),(#47518,#47519),(#47520,#47521),(#47522,
#47523),(#47524,#47525),(#47526,#47527),(#47528,#47529),(#47530,#47531),
(#47532,#47533),(#47534,#47535),(#47536,#47537),(#47538,#47539),(#47540,
#47541),(#47542,#47543),(#47544,#47545),(#47546,#47547),(#47548,#47549),
(#47550,#47551),(#47552,#47553),(#47554,#47555),(#47556,#47557),(#47558,
#47559),(#47560,#47561),(#47562,#47563),(#47564,#47565),(#47566,#47567),
(#47568,#47569),(#47570,#47571),(#47572,#47573),(#47574,#47575),(#47576,
#47577),(#47578,#47579),(#47580,#47581),(#47582,#47583),(#47584,#47585),
(#47586,#47587),(#47588,#47589),(#47590,#47591),(#47592,#47593),(#47594,
#47595),(#47596,#47597),(#47598,#47599),(#47600,#47601),(#47602,#47603),
(#47604,#47605),(#47606,#47607),(#47608,#47609),(#47610,#47611),(#47612,
#47613),(#47614,#47615),(#47616,#47617),(#47618,#47619),(#47620,#47621),
(#47622,#47623),(#47624,#47625),(#47626,#47627),(#47628,#47629),(#47630,
#47631),(#47632,#47633),(#47634,#47635),(#47636,#47637)),.UNSPECIFIED.,
 .F.,.F.,.F.)
B_SPLINE_SURFACE_WITH_KNOTS((6,1,1,1,1,1,1,1,1,1,1,1,1,1,1,1,1,1,1,1,1,
1,1,1,1,1,1,1,1,1,1,1,1,1,1,1,1,1,1,1,1,1,1,1,1,1,1,1,1,1,1,1,1,1,1,1,1,
1,1,1,1,1,1,1,1,6),(2,2),(-1.,-0.984615384615383,-0.969230769230768,-0.953846153846152,
-0.938461538461537,-0.923076923076922,-0.907692307692306,-0.892307692307691,
-0.876923076923076,-0.86153846153846,-0.846153846153845,-0.83076923076923,
-0.815384615384614,-0.799999999999999,-0.784615384615384,-0.769230769230768,
-0.753846153846153,-0.738461538461538,-0.723076923076922,-0.707692307692307,
-0.692307692307692,-0.676923076923076,-0.661538461538461,-0.646153846153846,
-0.63076923076923,-0.615384615384615,-0.6,-0.584615384615384,-0.569230769230769,
-0.553846153846154,-0.538461538461538,-0.523076923076923,-0.507692307692308,
-0.492307692307692,-0.476923076923077,-0.461538461538462,-0.446153846153846,
-0.430769230769231,-0.415384615384615,-0.4,-0.384615384615385,-0.369230769230769,
-0.353846153846154,-0.338461538461538,-0.323076923076923,-0.307692307692308,
-0.292307692307692,-0.276923076923077,-0.261538461538462,-0.246153846153846,
-0.230769230769231,-0.215384615384615,-0.2,-0.184615384615385,-0.169230769230769,
-0.153846153846154,-0.138461538461538,-0.123076923076923,-0.107692307692308,
-0.0923076923076923,-0.0769230769230769,-0.0615384615384615,-0.0461538461538462,
-0.0307692307692308,-0.0153846153846154,0.),(-1.,1.),.UNSPECIFIED.)
GEOMETRIC_REPRESENTATION_ITEM()
RATIONAL_B_SPLINE_SURFACE(((1.,1.),(1.,1.),(1.,1.),(1.,1.),(1.,1.),(1.,
1.),(1.,1.),(1.,1.),(1.,1.),(1.,1.),(1.,1.),(1.,1.),(1.,1.),(1.,1.),(1.,
1.),(1.,1.),(1.,1.),(1.,1.),(1.,1.),(1.,1.),(1.,1.),(1.,1.),(1.,1.),(1.,
1.),(1.,1.),(1.,1.),(1.,1.),(1.,1.),(1.,1.),(1.,1.),(1.,1.),(1.,1.),(1.,
1.),(1.,1.),(1.,1.),(1.,1.),(1.,1.),(1.,1.),(1.,1.),(1.,1.),(1.,1.),(1.,
1.),(1.,1.),(1.,1.),(1.,1.),(1.,1.),(1.,1.),(1.,1.),(1.,1.),(1.,1.),(1.,
1.),(1.,1.),(1.,1.),(1.,1.),(1.,1.),(1.,1.),(1.,1.),(1.,1.),(1.,1.),(1.,
1.),(1.,1.),(1.,1.),(1.,1.),(1.,1.),(1.,1.),(1.,1.),(1.,1.),(1.,1.),(1.,
1.),(1.,1.)))
REPRESENTATION_ITEM('')
SURFACE()
);
#65=(
BOUNDED_SURFACE()
B_SPLINE_SURFACE(5,1,((#47728,#47729),(#47730,#47731),(#47732,#47733),(#47734,
#47735),(#47736,#47737),(#47738,#47739),(#47740,#47741),(#47742,#47743),
(#47744,#47745),(#47746,#47747),(#47748,#47749),(#47750,#47751),(#47752,
#47753),(#47754,#47755),(#47756,#47757),(#47758,#47759),(#47760,#47761),
(#47762,#47763),(#47764,#47765),(#47766,#47767),(#47768,#47769),(#47770,
#47771),(#47772,#47773),(#47774,#47775),(#47776,#47777),(#47778,#47779),
(#47780,#47781),(#47782,#47783),(#47784,#47785),(#47786,#47787),(#47788,
#47789),(#47790,#47791),(#47792,#47793),(#47794,#47795),(#47796,#47797),
(#47798,#47799),(#47800,#47801),(#47802,#47803),(#47804,#47805),(#47806,
#47807),(#47808,#47809),(#47810,#47811),(#47812,#47813),(#47814,#47815),
(#47816,#47817),(#47818,#47819),(#47820,#47821),(#47822,#47823),(#47824,
#47825),(#47826,#47827),(#47828,#47829),(#47830,#47831),(#47832,#47833),
(#47834,#47835),(#47836,#47837),(#47838,#47839),(#47840,#47841),(#47842,
#47843),(#47844,#47845),(#47846,#47847),(#47848,#47849),(#47850,#47851),
(#47852,#47853),(#47854,#47855),(#47856,#47857),(#47858,#47859),(#47860,
#47861),(#47862,#47863),(#47864,#47865),(#47866,#47867)),.UNSPECIFIED.,
 .F.,.F.,.F.)
B_SPLINE_SURFACE_WITH_KNOTS((6,1,1,1,1,1,1,1,1,1,1,1,1,1,1,1,1,1,1,1,1,
1,1,1,1,1,1,1,1,1,1,1,1,1,1,1,1,1,1,1,1,1,1,1,1,1,1,1,1,1,1,1,1,1,1,1,1,
1,1,1,1,1,1,1,1,6),(2,2),(-1.,-0.984615384615383,-0.969230769230768,-0.953846153846152,
-0.938461538461537,-0.923076923076922,-0.907692307692306,-0.892307692307691,
-0.876923076923076,-0.86153846153846,-0.846153846153845,-0.83076923076923,
-0.815384615384614,-0.799999999999999,-0.784615384615384,-0.769230769230768,
-0.753846153846153,-0.738461538461538,-0.723076923076922,-0.707692307692307,
-0.692307692307692,-0.676923076923076,-0.661538461538461,-0.646153846153846,
-0.63076923076923,-0.615384615384615,-0.6,-0.584615384615384,-0.569230769230769,
-0.553846153846154,-0.538461538461538,-0.523076923076923,-0.507692307692308,
-0.492307692307692,-0.476923076923077,-0.461538461538462,-0.446153846153846,
-0.430769230769231,-0.415384615384615,-0.4,-0.384615384615385,-0.369230769230769,
-0.353846153846154,-0.338461538461538,-0.323076923076923,-0.307692307692308,
-0.292307692307692,-0.276923076923077,-0.261538461538462,-0.246153846153846,
-0.230769230769231,-0.215384615384615,-0.2,-0.184615384615385,-0.169230769230769,
-0.153846153846154,-0.138461538461538,-0.123076923076923,-0.107692307692308,
-0.0923076923076923,-0.0769230769230769,-0.0615384615384615,-0.0461538461538462,
-0.0307692307692308,-0.0153846153846154,0.),(-1.,1.),.UNSPECIFIED.)
GEOMETRIC_REPRESENTATION_ITEM()
RATIONAL_B_SPLINE_SURFACE(((1.,1.),(1.,1.),(1.,1.),(1.,1.),(1.,1.),(1.,
1.),(1.,1.),(1.,1.),(1.,1.),(1.,1.),(1.,1.),(1.,1.),(1.,1.),(1.,1.),(1.,
1.),(1.,1.),(1.,1.),(1.,1.),(1.,1.),(1.,1.),(1.,1.),(1.,1.),(1.,1.),(1.,
1.),(1.,1.),(1.,1.),(1.,1.),(1.,1.),(1.,1.),(1.,1.),(1.,1.),(1.,1.),(1.,
1.),(1.,1.),(1.,1.),(1.,1.),(1.,1.),(1.,1.),(1.,1.),(1.,1.),(1.,1.),(1.,
1.),(1.,1.),(1.,1.),(1.,1.),(1.,1.),(1.,1.),(1.,1.),(1.,1.),(1.,1.),(1.,
1.),(1.,1.),(1.,1.),(1.,1.),(1.,1.),(1.,1.),(1.,1.),(1.,1.),(1.,1.),(1.,
1.),(1.,1.),(1.,1.),(1.,1.),(1.,1.),(1.,1.),(1.,1.),(1.,1.),(1.,1.),(1.,
1.),(1.,1.)))
REPRESENTATION_ITEM('')
SURFACE()
);
#66=(
BOUNDED_SURFACE()
B_SPLINE_SURFACE(5,1,((#47940,#47941),(#47942,#47943),(#47944,#47945),(#47946,
#47947),(#47948,#47949),(#47950,#47951),(#47952,#47953),(#47954,#47955),
(#47956,#47957),(#47958,#47959),(#47960,#47961),(#47962,#47963),(#47964,
#47965),(#47966,#47967),(#47968,#47969),(#47970,#47971),(#47972,#47973),
(#47974,#47975),(#47976,#47977),(#47978,#47979),(#47980,#47981),(#47982,
#47983),(#47984,#47985),(#47986,#47987),(#47988,#47989),(#47990,#47991),
(#47992,#47993),(#47994,#47995),(#47996,#47997),(#47998,#47999),(#48000,
#48001),(#48002,#48003),(#48004,#48005),(#48006,#48007),(#48008,#48009),
(#48010,#48011),(#48012,#48013),(#48014,#48015),(#48016,#48017),(#48018,
#48019),(#48020,#48021),(#48022,#48023),(#48024,#48025),(#48026,#48027),
(#48028,#48029),(#48030,#48031),(#48032,#48033),(#48034,#48035),(#48036,
#48037),(#48038,#48039),(#48040,#48041),(#48042,#48043),(#48044,#48045),
(#48046,#48047),(#48048,#48049),(#48050,#48051),(#48052,#48053),(#48054,
#48055),(#48056,#48057),(#48058,#48059),(#48060,#48061),(#48062,#48063),
(#48064,#48065),(#48066,#48067),(#48068,#48069),(#48070,#48071),(#48072,
#48073),(#48074,#48075),(#48076,#48077),(#48078,#48079)),.UNSPECIFIED.,
 .F.,.F.,.F.)
B_SPLINE_SURFACE_WITH_KNOTS((6,1,1,1,1,1,1,1,1,1,1,1,1,1,1,1,1,1,1,1,1,
1,1,1,1,1,1,1,1,1,1,1,1,1,1,1,1,1,1,1,1,1,1,1,1,1,1,1,1,1,1,1,1,1,1,1,1,
1,1,1,1,1,1,1,1,6),(2,2),(-1.,-0.984615384615383,-0.969230769230768,-0.953846153846152,
-0.938461538461537,-0.923076923076922,-0.907692307692306,-0.892307692307691,
-0.876923076923076,-0.86153846153846,-0.846153846153845,-0.83076923076923,
-0.815384615384614,-0.799999999999999,-0.784615384615384,-0.769230769230768,
-0.753846153846153,-0.738461538461538,-0.723076923076922,-0.707692307692307,
-0.692307692307692,-0.676923076923076,-0.661538461538461,-0.646153846153846,
-0.63076923076923,-0.615384615384615,-0.6,-0.584615384615384,-0.569230769230769,
-0.553846153846154,-0.538461538461538,-0.523076923076923,-0.507692307692308,
-0.492307692307692,-0.476923076923077,-0.461538461538462,-0.446153846153846,
-0.430769230769231,-0.415384615384615,-0.4,-0.384615384615385,-0.369230769230769,
-0.353846153846154,-0.338461538461538,-0.323076923076923,-0.307692307692308,
-0.292307692307692,-0.276923076923077,-0.261538461538462,-0.246153846153846,
-0.230769230769231,-0.215384615384615,-0.2,-0.184615384615385,-0.169230769230769,
-0.153846153846154,-0.138461538461538,-0.123076923076923,-0.107692307692308,
-0.0923076923076923,-0.0769230769230769,-0.0615384615384615,-0.0461538461538462,
-0.0307692307692308,-0.0153846153846154,0.),(-1.,1.),.UNSPECIFIED.)
GEOMETRIC_REPRESENTATION_ITEM()
RATIONAL_B_SPLINE_SURFACE(((1.,1.),(1.,1.),(1.,1.),(1.,1.),(1.,1.),(1.,
1.),(1.,1.),(1.,1.),(1.,1.),(1.,1.),(1.,1.),(1.,1.),(1.,1.),(1.,1.),(1.,
1.),(1.,1.),(1.,1.),(1.,1.),(1.,1.),(1.,1.),(1.,1.),(1.,1.),(1.,1.),(1.,
1.),(1.,1.),(1.,1.),(1.,1.),(1.,1.),(1.,1.),(1.,1.),(1.,1.),(1.,1.),(1.,
1.),(1.,1.),(1.,1.),(1.,1.),(1.,1.),(1.,1.),(1.,1.),(1.,1.),(1.,1.),(1.,
1.),(1.,1.),(1.,1.),(1.,1.),(1.,1.),(1.,1.),(1.,1.),(1.,1.),(1.,1.),(1.,
1.),(1.,1.),(1.,1.),(1.,1.),(1.,1.),(1.,1.),(1.,1.),(1.,1.),(1.,1.),(1.,
1.),(1.,1.),(1.,1.),(1.,1.),(1.,1.),(1.,1.),(1.,1.),(1.,1.),(1.,1.),(1.,
1.),(1.,1.)))
REPRESENTATION_ITEM('')
SURFACE()
);
#67=(
BOUNDED_SURFACE()
B_SPLINE_SURFACE(5,1,((#48170,#48171),(#48172,#48173),(#48174,#48175),(#48176,
#48177),(#48178,#48179),(#48180,#48181),(#48182,#48183),(#48184,#48185),
(#48186,#48187),(#48188,#48189),(#48190,#48191),(#48192,#48193),(#48194,
#48195),(#48196,#48197),(#48198,#48199),(#48200,#48201),(#48202,#48203),
(#48204,#48205),(#48206,#48207),(#48208,#48209),(#48210,#48211),(#48212,
#48213),(#48214,#48215),(#48216,#48217),(#48218,#48219),(#48220,#48221),
(#48222,#48223),(#48224,#48225),(#48226,#48227),(#48228,#48229),(#48230,
#48231),(#48232,#48233),(#48234,#48235),(#48236,#48237),(#48238,#48239),
(#48240,#48241),(#48242,#48243),(#48244,#48245),(#48246,#48247),(#48248,
#48249),(#48250,#48251),(#48252,#48253),(#48254,#48255),(#48256,#48257),
(#48258,#48259),(#48260,#48261),(#48262,#48263),(#48264,#48265),(#48266,
#48267),(#48268,#48269),(#48270,#48271),(#48272,#48273),(#48274,#48275),
(#48276,#48277),(#48278,#48279),(#48280,#48281),(#48282,#48283),(#48284,
#48285),(#48286,#48287),(#48288,#48289),(#48290,#48291),(#48292,#48293),
(#48294,#48295),(#48296,#48297),(#48298,#48299),(#48300,#48301),(#48302,
#48303),(#48304,#48305),(#48306,#48307),(#48308,#48309)),.UNSPECIFIED.,
 .F.,.F.,.F.)
B_SPLINE_SURFACE_WITH_KNOTS((6,1,1,1,1,1,1,1,1,1,1,1,1,1,1,1,1,1,1,1,1,
1,1,1,1,1,1,1,1,1,1,1,1,1,1,1,1,1,1,1,1,1,1,1,1,1,1,1,1,1,1,1,1,1,1,1,1,
1,1,1,1,1,1,1,1,6),(2,2),(-1.,-0.984615384615383,-0.969230769230768,-0.953846153846152,
-0.938461538461537,-0.923076923076922,-0.907692307692306,-0.892307692307691,
-0.876923076923076,-0.86153846153846,-0.846153846153845,-0.83076923076923,
-0.815384615384614,-0.799999999999999,-0.784615384615384,-0.769230769230768,
-0.753846153846153,-0.738461538461538,-0.723076923076922,-0.707692307692307,
-0.692307692307692,-0.676923076923076,-0.661538461538461,-0.646153846153846,
-0.63076923076923,-0.615384615384615,-0.6,-0.584615384615384,-0.569230769230769,
-0.553846153846154,-0.538461538461538,-0.523076923076923,-0.507692307692308,
-0.492307692307692,-0.476923076923077,-0.461538461538462,-0.446153846153846,
-0.430769230769231,-0.415384615384615,-0.4,-0.384615384615385,-0.369230769230769,
-0.353846153846154,-0.338461538461538,-0.323076923076923,-0.307692307692308,
-0.292307692307692,-0.276923076923077,-0.261538461538462,-0.246153846153846,
-0.230769230769231,-0.215384615384615,-0.2,-0.184615384615385,-0.169230769230769,
-0.153846153846154,-0.138461538461538,-0.123076923076923,-0.107692307692308,
-0.0923076923076923,-0.0769230769230769,-0.0615384615384615,-0.0461538461538462,
-0.0307692307692308,-0.0153846153846154,0.),(-1.,1.),.UNSPECIFIED.)
GEOMETRIC_REPRESENTATION_ITEM()
RATIONAL_B_SPLINE_SURFACE(((1.,1.),(1.,1.),(1.,1.),(1.,1.),(1.,1.),(1.,
1.),(1.,1.),(1.,1.),(1.,1.),(1.,1.),(1.,1.),(1.,1.),(1.,1.),(1.,1.),(1.,
1.),(1.,1.),(1.,1.),(1.,1.),(1.,1.),(1.,1.),(1.,1.),(1.,1.),(1.,1.),(1.,
1.),(1.,1.),(1.,1.),(1.,1.),(1.,1.),(1.,1.),(1.,1.),(1.,1.),(1.,1.),(1.,
1.),(1.,1.),(1.,1.),(1.,1.),(1.,1.),(1.,1.),(1.,1.),(1.,1.),(1.,1.),(1.,
1.),(1.,1.),(1.,1.),(1.,1.),(1.,1.),(1.,1.),(1.,1.),(1.,1.),(1.,1.),(1.,
1.),(1.,1.),(1.,1.),(1.,1.),(1.,1.),(1.,1.),(1.,1.),(1.,1.),(1.,1.),(1.,
1.),(1.,1.),(1.,1.),(1.,1.),(1.,1.),(1.,1.),(1.,1.),(1.,1.),(1.,1.),(1.,
1.),(1.,1.)))
REPRESENTATION_ITEM('')
SURFACE()
);
#68=(
BOUNDED_SURFACE()
B_SPLINE_SURFACE(5,1,((#48382,#48383),(#48384,#48385),(#48386,#48387),(#48388,
#48389),(#48390,#48391),(#48392,#48393),(#48394,#48395),(#48396,#48397),
(#48398,#48399),(#48400,#48401),(#48402,#48403),(#48404,#48405),(#48406,
#48407),(#48408,#48409),(#48410,#48411),(#48412,#48413),(#48414,#48415),
(#48416,#48417),(#48418,#48419),(#48420,#48421),(#48422,#48423),(#48424,
#48425),(#48426,#48427),(#48428,#48429),(#48430,#48431),(#48432,#48433),
(#48434,#48435),(#48436,#48437),(#48438,#48439),(#48440,#48441),(#48442,
#48443),(#48444,#48445),(#48446,#48447),(#48448,#48449),(#48450,#48451),
(#48452,#48453),(#48454,#48455),(#48456,#48457),(#48458,#48459),(#48460,
#48461),(#48462,#48463),(#48464,#48465),(#48466,#48467),(#48468,#48469),
(#48470,#48471),(#48472,#48473),(#48474,#48475),(#48476,#48477),(#48478,
#48479),(#48480,#48481),(#48482,#48483),(#48484,#48485),(#48486,#48487),
(#48488,#48489),(#48490,#48491),(#48492,#48493),(#48494,#48495),(#48496,
#48497),(#48498,#48499),(#48500,#48501),(#48502,#48503),(#48504,#48505),
(#48506,#48507),(#48508,#48509),(#48510,#48511),(#48512,#48513),(#48514,
#48515),(#48516,#48517),(#48518,#48519),(#48520,#48521)),.UNSPECIFIED.,
 .F.,.F.,.F.)
B_SPLINE_SURFACE_WITH_KNOTS((6,1,1,1,1,1,1,1,1,1,1,1,1,1,1,1,1,1,1,1,1,
1,1,1,1,1,1,1,1,1,1,1,1,1,1,1,1,1,1,1,1,1,1,1,1,1,1,1,1,1,1,1,1,1,1,1,1,
1,1,1,1,1,1,1,1,6),(2,2),(-1.,-0.984615384615383,-0.969230769230768,-0.953846153846152,
-0.938461538461537,-0.923076923076922,-0.907692307692306,-0.892307692307691,
-0.876923076923076,-0.86153846153846,-0.846153846153845,-0.83076923076923,
-0.815384615384614,-0.799999999999999,-0.784615384615384,-0.769230769230768,
-0.753846153846153,-0.738461538461538,-0.723076923076922,-0.707692307692307,
-0.692307692307692,-0.676923076923076,-0.661538461538461,-0.646153846153846,
-0.63076923076923,-0.615384615384615,-0.6,-0.584615384615384,-0.569230769230769,
-0.553846153846154,-0.538461538461538,-0.523076923076923,-0.507692307692308,
-0.492307692307692,-0.476923076923077,-0.461538461538462,-0.446153846153846,
-0.430769230769231,-0.415384615384615,-0.4,-0.384615384615385,-0.369230769230769,
-0.353846153846154,-0.338461538461538,-0.323076923076923,-0.307692307692308,
-0.292307692307692,-0.276923076923077,-0.261538461538462,-0.246153846153846,
-0.230769230769231,-0.215384615384615,-0.2,-0.184615384615385,-0.169230769230769,
-0.153846153846154,-0.138461538461538,-0.123076923076923,-0.107692307692308,
-0.0923076923076923,-0.0769230769230769,-0.0615384615384615,-0.0461538461538462,
-0.0307692307692308,-0.0153846153846154,0.),(-1.,1.),.UNSPECIFIED.)
GEOMETRIC_REPRESENTATION_ITEM()
RATIONAL_B_SPLINE_SURFACE(((1.,1.),(1.,1.),(1.,1.),(1.,1.),(1.,1.),(1.,
1.),(1.,1.),(1.,1.),(1.,1.),(1.,1.),(1.,1.),(1.,1.),(1.,1.),(1.,1.),(1.,
1.),(1.,1.),(1.,1.),(1.,1.),(1.,1.),(1.,1.),(1.,1.),(1.,1.),(1.,1.),(1.,
1.),(1.,1.),(1.,1.),(1.,1.),(1.,1.),(1.,1.),(1.,1.),(1.,1.),(1.,1.),(1.,
1.),(1.,1.),(1.,1.),(1.,1.),(1.,1.),(1.,1.),(1.,1.),(1.,1.),(1.,1.),(1.,
1.),(1.,1.),(1.,1.),(1.,1.),(1.,1.),(1.,1.),(1.,1.),(1.,1.),(1.,1.),(1.,
1.),(1.,1.),(1.,1.),(1.,1.),(1.,1.),(1.,1.),(1.,1.),(1.,1.),(1.,1.),(1.,
1.),(1.,1.),(1.,1.),(1.,1.),(1.,1.),(1.,1.),(1.,1.),(1.,1.),(1.,1.),(1.,
1.),(1.,1.)))
REPRESENTATION_ITEM('')
SURFACE()
);
#69=(
BOUNDED_SURFACE()
B_SPLINE_SURFACE(5,1,((#48612,#48613),(#48614,#48615),(#48616,#48617),(#48618,
#48619),(#48620,#48621),(#48622,#48623),(#48624,#48625),(#48626,#48627),
(#48628,#48629),(#48630,#48631),(#48632,#48633),(#48634,#48635),(#48636,
#48637),(#48638,#48639),(#48640,#48641),(#48642,#48643),(#48644,#48645),
(#48646,#48647),(#48648,#48649),(#48650,#48651),(#48652,#48653),(#48654,
#48655),(#48656,#48657),(#48658,#48659),(#48660,#48661),(#48662,#48663),
(#48664,#48665),(#48666,#48667),(#48668,#48669),(#48670,#48671),(#48672,
#48673),(#48674,#48675),(#48676,#48677),(#48678,#48679),(#48680,#48681),
(#48682,#48683),(#48684,#48685),(#48686,#48687),(#48688,#48689),(#48690,
#48691),(#48692,#48693),(#48694,#48695),(#48696,#48697),(#48698,#48699),
(#48700,#48701),(#48702,#48703),(#48704,#48705),(#48706,#48707),(#48708,
#48709),(#48710,#48711),(#48712,#48713),(#48714,#48715),(#48716,#48717),
(#48718,#48719),(#48720,#48721),(#48722,#48723),(#48724,#48725),(#48726,
#48727),(#48728,#48729),(#48730,#48731),(#48732,#48733),(#48734,#48735),
(#48736,#48737),(#48738,#48739),(#48740,#48741),(#48742,#48743),(#48744,
#48745),(#48746,#48747),(#48748,#48749),(#48750,#48751)),.UNSPECIFIED.,
 .F.,.F.,.F.)
B_SPLINE_SURFACE_WITH_KNOTS((6,1,1,1,1,1,1,1,1,1,1,1,1,1,1,1,1,1,1,1,1,
1,1,1,1,1,1,1,1,1,1,1,1,1,1,1,1,1,1,1,1,1,1,1,1,1,1,1,1,1,1,1,1,1,1,1,1,
1,1,1,1,1,1,1,1,6),(2,2),(-1.,-0.984615384615383,-0.969230769230768,-0.953846153846152,
-0.938461538461537,-0.923076923076922,-0.907692307692306,-0.892307692307691,
-0.876923076923076,-0.86153846153846,-0.846153846153845,-0.83076923076923,
-0.815384615384614,-0.799999999999999,-0.784615384615384,-0.769230769230768,
-0.753846153846153,-0.738461538461538,-0.723076923076922,-0.707692307692307,
-0.692307692307692,-0.676923076923076,-0.661538461538461,-0.646153846153846,
-0.63076923076923,-0.615384615384615,-0.6,-0.584615384615384,-0.569230769230769,
-0.553846153846154,-0.538461538461538,-0.523076923076923,-0.507692307692308,
-0.492307692307692,-0.476923076923077,-0.461538461538462,-0.446153846153846,
-0.430769230769231,-0.415384615384615,-0.4,-0.384615384615385,-0.369230769230769,
-0.353846153846154,-0.338461538461538,-0.323076923076923,-0.307692307692308,
-0.292307692307692,-0.276923076923077,-0.261538461538462,-0.246153846153846,
-0.230769230769231,-0.215384615384615,-0.2,-0.184615384615385,-0.169230769230769,
-0.153846153846154,-0.138461538461538,-0.123076923076923,-0.107692307692308,
-0.0923076923076923,-0.0769230769230769,-0.0615384615384615,-0.0461538461538462,
-0.0307692307692308,-0.0153846153846154,0.),(-1.,1.),.UNSPECIFIED.)
GEOMETRIC_REPRESENTATION_ITEM()
RATIONAL_B_SPLINE_SURFACE(((1.,1.),(1.,1.),(1.,1.),(1.,1.),(1.,1.),(1.,
1.),(1.,1.),(1.,1.),(1.,1.),(1.,1.),(1.,1.),(1.,1.),(1.,1.),(1.,1.),(1.,
1.),(1.,1.),(1.,1.),(1.,1.),(1.,1.),(1.,1.),(1.,1.),(1.,1.),(1.,1.),(1.,
1.),(1.,1.),(1.,1.),(1.,1.),(1.,1.),(1.,1.),(1.,1.),(1.,1.),(1.,1.),(1.,
1.),(1.,1.),(1.,1.),(1.,1.),(1.,1.),(1.,1.),(1.,1.),(1.,1.),(1.,1.),(1.,
1.),(1.,1.),(1.,1.),(1.,1.),(1.,1.),(1.,1.),(1.,1.),(1.,1.),(1.,1.),(1.,
1.),(1.,1.),(1.,1.),(1.,1.),(1.,1.),(1.,1.),(1.,1.),(1.,1.),(1.,1.),(1.,
1.),(1.,1.),(1.,1.),(1.,1.),(1.,1.),(1.,1.),(1.,1.),(1.,1.),(1.,1.),(1.,
1.),(1.,1.)))
REPRESENTATION_ITEM('')
SURFACE()
);
#70=(
BOUNDED_SURFACE()
B_SPLINE_SURFACE(5,1,((#48824,#48825),(#48826,#48827),(#48828,#48829),(#48830,
#48831),(#48832,#48833),(#48834,#48835),(#48836,#48837),(#48838,#48839),
(#48840,#48841),(#48842,#48843),(#48844,#48845),(#48846,#48847),(#48848,
#48849),(#48850,#48851),(#48852,#48853),(#48854,#48855),(#48856,#48857),
(#48858,#48859),(#48860,#48861),(#48862,#48863),(#48864,#48865),(#48866,
#48867),(#48868,#48869),(#48870,#48871),(#48872,#48873),(#48874,#48875),
(#48876,#48877),(#48878,#48879),(#48880,#48881),(#48882,#48883),(#48884,
#48885),(#48886,#48887),(#48888,#48889),(#48890,#48891),(#48892,#48893),
(#48894,#48895),(#48896,#48897),(#48898,#48899),(#48900,#48901),(#48902,
#48903),(#48904,#48905),(#48906,#48907),(#48908,#48909),(#48910,#48911),
(#48912,#48913),(#48914,#48915),(#48916,#48917),(#48918,#48919),(#48920,
#48921),(#48922,#48923),(#48924,#48925),(#48926,#48927),(#48928,#48929),
(#48930,#48931),(#48932,#48933),(#48934,#48935),(#48936,#48937),(#48938,
#48939),(#48940,#48941),(#48942,#48943),(#48944,#48945),(#48946,#48947),
(#48948,#48949),(#48950,#48951),(#48952,#48953),(#48954,#48955),(#48956,
#48957),(#48958,#48959),(#48960,#48961),(#48962,#48963)),.UNSPECIFIED.,
 .F.,.F.,.F.)
B_SPLINE_SURFACE_WITH_KNOTS((6,1,1,1,1,1,1,1,1,1,1,1,1,1,1,1,1,1,1,1,1,
1,1,1,1,1,1,1,1,1,1,1,1,1,1,1,1,1,1,1,1,1,1,1,1,1,1,1,1,1,1,1,1,1,1,1,1,
1,1,1,1,1,1,1,1,6),(2,2),(-1.,-0.984615384615383,-0.969230769230768,-0.953846153846152,
-0.938461538461537,-0.923076923076922,-0.907692307692306,-0.892307692307691,
-0.876923076923076,-0.86153846153846,-0.846153846153845,-0.83076923076923,
-0.815384615384614,-0.799999999999999,-0.784615384615384,-0.769230769230768,
-0.753846153846153,-0.738461538461538,-0.723076923076922,-0.707692307692307,
-0.692307692307692,-0.676923076923076,-0.661538461538461,-0.646153846153846,
-0.63076923076923,-0.615384615384615,-0.6,-0.584615384615384,-0.569230769230769,
-0.553846153846154,-0.538461538461538,-0.523076923076923,-0.507692307692308,
-0.492307692307692,-0.476923076923077,-0.461538461538462,-0.446153846153846,
-0.430769230769231,-0.415384615384615,-0.4,-0.384615384615385,-0.369230769230769,
-0.353846153846154,-0.338461538461538,-0.323076923076923,-0.307692307692308,
-0.292307692307692,-0.276923076923077,-0.261538461538462,-0.246153846153846,
-0.230769230769231,-0.215384615384615,-0.2,-0.184615384615385,-0.169230769230769,
-0.153846153846154,-0.138461538461538,-0.123076923076923,-0.107692307692308,
-0.0923076923076923,-0.0769230769230769,-0.0615384615384615,-0.0461538461538462,
-0.0307692307692308,-0.0153846153846154,0.),(-1.,1.),.UNSPECIFIED.)
GEOMETRIC_REPRESENTATION_ITEM()
RATIONAL_B_SPLINE_SURFACE(((1.,1.),(1.,1.),(1.,1.),(1.,1.),(1.,1.),(1.,
1.),(1.,1.),(1.,1.),(1.,1.),(1.,1.),(1.,1.),(1.,1.),(1.,1.),(1.,1.),(1.,
1.),(1.,1.),(1.,1.),(1.,1.),(1.,1.),(1.,1.),(1.,1.),(1.,1.),(1.,1.),(1.,
1.),(1.,1.),(1.,1.),(1.,1.),(1.,1.),(1.,1.),(1.,1.),(1.,1.),(1.,1.),(1.,
1.),(1.,1.),(1.,1.),(1.,1.),(1.,1.),(1.,1.),(1.,1.),(1.,1.),(1.,1.),(1.,
1.),(1.,1.),(1.,1.),(1.,1.),(1.,1.),(1.,1.),(1.,1.),(1.,1.),(1.,1.),(1.,
1.),(1.,1.),(1.,1.),(1.,1.),(1.,1.),(1.,1.),(1.,1.),(1.,1.),(1.,1.),(1.,
1.),(1.,1.),(1.,1.),(1.,1.),(1.,1.),(1.,1.),(1.,1.),(1.,1.),(1.,1.),(1.,
1.),(1.,1.)))
REPRESENTATION_ITEM('')
SURFACE()
);
#71=(
BOUNDED_SURFACE()
B_SPLINE_SURFACE(5,1,((#49054,#49055),(#49056,#49057),(#49058,#49059),(#49060,
#49061),(#49062,#49063),(#49064,#49065),(#49066,#49067),(#49068,#49069),
(#49070,#49071),(#49072,#49073),(#49074,#49075),(#49076,#49077),(#49078,
#49079),(#49080,#49081),(#49082,#49083),(#49084,#49085),(#49086,#49087),
(#49088,#49089),(#49090,#49091),(#49092,#49093),(#49094,#49095),(#49096,
#49097),(#49098,#49099),(#49100,#49101),(#49102,#49103),(#49104,#49105),
(#49106,#49107),(#49108,#49109),(#49110,#49111),(#49112,#49113),(#49114,
#49115),(#49116,#49117),(#49118,#49119),(#49120,#49121),(#49122,#49123),
(#49124,#49125),(#49126,#49127),(#49128,#49129),(#49130,#49131),(#49132,
#49133),(#49134,#49135),(#49136,#49137),(#49138,#49139),(#49140,#49141),
(#49142,#49143),(#49144,#49145),(#49146,#49147),(#49148,#49149),(#49150,
#49151),(#49152,#49153),(#49154,#49155),(#49156,#49157),(#49158,#49159),
(#49160,#49161),(#49162,#49163),(#49164,#49165),(#49166,#49167),(#49168,
#49169),(#49170,#49171),(#49172,#49173),(#49174,#49175),(#49176,#49177),
(#49178,#49179),(#49180,#49181),(#49182,#49183),(#49184,#49185),(#49186,
#49187),(#49188,#49189),(#49190,#49191),(#49192,#49193)),.UNSPECIFIED.,
 .F.,.F.,.F.)
B_SPLINE_SURFACE_WITH_KNOTS((6,1,1,1,1,1,1,1,1,1,1,1,1,1,1,1,1,1,1,1,1,
1,1,1,1,1,1,1,1,1,1,1,1,1,1,1,1,1,1,1,1,1,1,1,1,1,1,1,1,1,1,1,1,1,1,1,1,
1,1,1,1,1,1,1,1,6),(2,2),(-1.,-0.984615384615383,-0.969230769230768,-0.953846153846152,
-0.938461538461537,-0.923076923076922,-0.907692307692306,-0.892307692307691,
-0.876923076923076,-0.86153846153846,-0.846153846153845,-0.83076923076923,
-0.815384615384614,-0.799999999999999,-0.784615384615384,-0.769230769230768,
-0.753846153846153,-0.738461538461538,-0.723076923076922,-0.707692307692307,
-0.692307692307692,-0.676923076923076,-0.661538461538461,-0.646153846153846,
-0.63076923076923,-0.615384615384615,-0.6,-0.584615384615384,-0.569230769230769,
-0.553846153846154,-0.538461538461538,-0.523076923076923,-0.507692307692308,
-0.492307692307692,-0.476923076923077,-0.461538461538462,-0.446153846153846,
-0.430769230769231,-0.415384615384615,-0.4,-0.384615384615385,-0.369230769230769,
-0.353846153846154,-0.338461538461538,-0.323076923076923,-0.307692307692308,
-0.292307692307692,-0.276923076923077,-0.261538461538462,-0.246153846153846,
-0.230769230769231,-0.215384615384615,-0.2,-0.184615384615385,-0.169230769230769,
-0.153846153846154,-0.138461538461538,-0.123076923076923,-0.107692307692308,
-0.0923076923076923,-0.0769230769230769,-0.0615384615384615,-0.0461538461538462,
-0.0307692307692308,-0.0153846153846154,0.),(-1.,1.),.UNSPECIFIED.)
GEOMETRIC_REPRESENTATION_ITEM()
RATIONAL_B_SPLINE_SURFACE(((1.,1.),(1.,1.),(1.,1.),(1.,1.),(1.,1.),(1.,
1.),(1.,1.),(1.,1.),(1.,1.),(1.,1.),(1.,1.),(1.,1.),(1.,1.),(1.,1.),(1.,
1.),(1.,1.),(1.,1.),(1.,1.),(1.,1.),(1.,1.),(1.,1.),(1.,1.),(1.,1.),(1.,
1.),(1.,1.),(1.,1.),(1.,1.),(1.,1.),(1.,1.),(1.,1.),(1.,1.),(1.,1.),(1.,
1.),(1.,1.),(1.,1.),(1.,1.),(1.,1.),(1.,1.),(1.,1.),(1.,1.),(1.,1.),(1.,
1.),(1.,1.),(1.,1.),(1.,1.),(1.,1.),(1.,1.),(1.,1.),(1.,1.),(1.,1.),(1.,
1.),(1.,1.),(1.,1.),(1.,1.),(1.,1.),(1.,1.),(1.,1.),(1.,1.),(1.,1.),(1.,
1.),(1.,1.),(1.,1.),(1.,1.),(1.,1.),(1.,1.),(1.,1.),(1.,1.),(1.,1.),(1.,
1.),(1.,1.)))
REPRESENTATION_ITEM('')
SURFACE()
);
#72=(
BOUNDED_SURFACE()
B_SPLINE_SURFACE(5,1,((#49266,#49267),(#49268,#49269),(#49270,#49271),(#49272,
#49273),(#49274,#49275),(#49276,#49277),(#49278,#49279),(#49280,#49281),
(#49282,#49283),(#49284,#49285),(#49286,#49287),(#49288,#49289),(#49290,
#49291),(#49292,#49293),(#49294,#49295),(#49296,#49297),(#49298,#49299),
(#49300,#49301),(#49302,#49303),(#49304,#49305),(#49306,#49307),(#49308,
#49309),(#49310,#49311),(#49312,#49313),(#49314,#49315),(#49316,#49317),
(#49318,#49319),(#49320,#49321),(#49322,#49323),(#49324,#49325),(#49326,
#49327),(#49328,#49329),(#49330,#49331),(#49332,#49333),(#49334,#49335),
(#49336,#49337),(#49338,#49339),(#49340,#49341),(#49342,#49343),(#49344,
#49345),(#49346,#49347),(#49348,#49349),(#49350,#49351),(#49352,#49353),
(#49354,#49355),(#49356,#49357),(#49358,#49359),(#49360,#49361),(#49362,
#49363),(#49364,#49365),(#49366,#49367),(#49368,#49369),(#49370,#49371),
(#49372,#49373),(#49374,#49375),(#49376,#49377),(#49378,#49379),(#49380,
#49381),(#49382,#49383),(#49384,#49385),(#49386,#49387),(#49388,#49389),
(#49390,#49391),(#49392,#49393),(#49394,#49395),(#49396,#49397),(#49398,
#49399),(#49400,#49401),(#49402,#49403),(#49404,#49405)),.UNSPECIFIED.,
 .F.,.F.,.F.)
B_SPLINE_SURFACE_WITH_KNOTS((6,1,1,1,1,1,1,1,1,1,1,1,1,1,1,1,1,1,1,1,1,
1,1,1,1,1,1,1,1,1,1,1,1,1,1,1,1,1,1,1,1,1,1,1,1,1,1,1,1,1,1,1,1,1,1,1,1,
1,1,1,1,1,1,1,1,6),(2,2),(-1.,-0.984615384615383,-0.969230769230768,-0.953846153846152,
-0.938461538461537,-0.923076923076922,-0.907692307692306,-0.892307692307691,
-0.876923076923076,-0.86153846153846,-0.846153846153845,-0.83076923076923,
-0.815384615384614,-0.799999999999999,-0.784615384615384,-0.769230769230768,
-0.753846153846153,-0.738461538461538,-0.723076923076922,-0.707692307692307,
-0.692307692307692,-0.676923076923076,-0.661538461538461,-0.646153846153846,
-0.63076923076923,-0.615384615384615,-0.6,-0.584615384615384,-0.569230769230769,
-0.553846153846154,-0.538461538461538,-0.523076923076923,-0.507692307692308,
-0.492307692307692,-0.476923076923077,-0.461538461538462,-0.446153846153846,
-0.430769230769231,-0.415384615384615,-0.4,-0.384615384615385,-0.369230769230769,
-0.353846153846154,-0.338461538461538,-0.323076923076923,-0.307692307692308,
-0.292307692307692,-0.276923076923077,-0.261538461538462,-0.246153846153846,
-0.230769230769231,-0.215384615384615,-0.2,-0.184615384615385,-0.169230769230769,
-0.153846153846154,-0.138461538461538,-0.123076923076923,-0.107692307692308,
-0.0923076923076923,-0.0769230769230769,-0.0615384615384615,-0.0461538461538462,
-0.0307692307692308,-0.0153846153846154,0.),(-1.,1.),.UNSPECIFIED.)
GEOMETRIC_REPRESENTATION_ITEM()
RATIONAL_B_SPLINE_SURFACE(((1.,1.),(1.,1.),(1.,1.),(1.,1.),(1.,1.),(1.,
1.),(1.,1.),(1.,1.),(1.,1.),(1.,1.),(1.,1.),(1.,1.),(1.,1.),(1.,1.),(1.,
1.),(1.,1.),(1.,1.),(1.,1.),(1.,1.),(1.,1.),(1.,1.),(1.,1.),(1.,1.),(1.,
1.),(1.,1.),(1.,1.),(1.,1.),(1.,1.),(1.,1.),(1.,1.),(1.,1.),(1.,1.),(1.,
1.),(1.,1.),(1.,1.),(1.,1.),(1.,1.),(1.,1.),(1.,1.),(1.,1.),(1.,1.),(1.,
1.),(1.,1.),(1.,1.),(1.,1.),(1.,1.),(1.,1.),(1.,1.),(1.,1.),(1.,1.),(1.,
1.),(1.,1.),(1.,1.),(1.,1.),(1.,1.),(1.,1.),(1.,1.),(1.,1.),(1.,1.),(1.,
1.),(1.,1.),(1.,1.),(1.,1.),(1.,1.),(1.,1.),(1.,1.),(1.,1.),(1.,1.),(1.,
1.),(1.,1.)))
REPRESENTATION_ITEM('')
SURFACE()
);
#73=(
BOUNDED_SURFACE()
B_SPLINE_SURFACE(5,1,((#49496,#49497),(#49498,#49499),(#49500,#49501),(#49502,
#49503),(#49504,#49505),(#49506,#49507),(#49508,#49509),(#49510,#49511),
(#49512,#49513),(#49514,#49515),(#49516,#49517),(#49518,#49519),(#49520,
#49521),(#49522,#49523),(#49524,#49525),(#49526,#49527),(#49528,#49529),
(#49530,#49531),(#49532,#49533),(#49534,#49535),(#49536,#49537),(#49538,
#49539),(#49540,#49541),(#49542,#49543),(#49544,#49545),(#49546,#49547),
(#49548,#49549),(#49550,#49551),(#49552,#49553),(#49554,#49555),(#49556,
#49557),(#49558,#49559),(#49560,#49561),(#49562,#49563),(#49564,#49565),
(#49566,#49567),(#49568,#49569),(#49570,#49571),(#49572,#49573),(#49574,
#49575),(#49576,#49577),(#49578,#49579),(#49580,#49581),(#49582,#49583),
(#49584,#49585),(#49586,#49587),(#49588,#49589),(#49590,#49591),(#49592,
#49593),(#49594,#49595),(#49596,#49597),(#49598,#49599),(#49600,#49601),
(#49602,#49603),(#49604,#49605),(#49606,#49607),(#49608,#49609),(#49610,
#49611),(#49612,#49613),(#49614,#49615),(#49616,#49617),(#49618,#49619),
(#49620,#49621),(#49622,#49623),(#49624,#49625),(#49626,#49627),(#49628,
#49629),(#49630,#49631),(#49632,#49633),(#49634,#49635)),.UNSPECIFIED.,
 .F.,.F.,.F.)
B_SPLINE_SURFACE_WITH_KNOTS((6,1,1,1,1,1,1,1,1,1,1,1,1,1,1,1,1,1,1,1,1,
1,1,1,1,1,1,1,1,1,1,1,1,1,1,1,1,1,1,1,1,1,1,1,1,1,1,1,1,1,1,1,1,1,1,1,1,
1,1,1,1,1,1,1,1,6),(2,2),(-1.,-0.984615384615383,-0.969230769230768,-0.953846153846152,
-0.938461538461537,-0.923076923076922,-0.907692307692306,-0.892307692307691,
-0.876923076923076,-0.86153846153846,-0.846153846153845,-0.83076923076923,
-0.815384615384614,-0.799999999999999,-0.784615384615384,-0.769230769230768,
-0.753846153846153,-0.738461538461538,-0.723076923076922,-0.707692307692307,
-0.692307692307692,-0.676923076923076,-0.661538461538461,-0.646153846153846,
-0.63076923076923,-0.615384615384615,-0.6,-0.584615384615384,-0.569230769230769,
-0.553846153846154,-0.538461538461538,-0.523076923076923,-0.507692307692308,
-0.492307692307692,-0.476923076923077,-0.461538461538462,-0.446153846153846,
-0.430769230769231,-0.415384615384615,-0.4,-0.384615384615385,-0.369230769230769,
-0.353846153846154,-0.338461538461538,-0.323076923076923,-0.307692307692308,
-0.292307692307692,-0.276923076923077,-0.261538461538462,-0.246153846153846,
-0.230769230769231,-0.215384615384615,-0.2,-0.184615384615385,-0.169230769230769,
-0.153846153846154,-0.138461538461538,-0.123076923076923,-0.107692307692308,
-0.0923076923076923,-0.0769230769230769,-0.0615384615384615,-0.0461538461538462,
-0.0307692307692308,-0.0153846153846154,0.),(-1.,1.),.UNSPECIFIED.)
GEOMETRIC_REPRESENTATION_ITEM()
RATIONAL_B_SPLINE_SURFACE(((1.,1.),(1.,1.),(1.,1.),(1.,1.),(1.,1.),(1.,
1.),(1.,1.),(1.,1.),(1.,1.),(1.,1.),(1.,1.),(1.,1.),(1.,1.),(1.,1.),(1.,
1.),(1.,1.),(1.,1.),(1.,1.),(1.,1.),(1.,1.),(1.,1.),(1.,1.),(1.,1.),(1.,
1.),(1.,1.),(1.,1.),(1.,1.),(1.,1.),(1.,1.),(1.,1.),(1.,1.),(1.,1.),(1.,
1.),(1.,1.),(1.,1.),(1.,1.),(1.,1.),(1.,1.),(1.,1.),(1.,1.),(1.,1.),(1.,
1.),(1.,1.),(1.,1.),(1.,1.),(1.,1.),(1.,1.),(1.,1.),(1.,1.),(1.,1.),(1.,
1.),(1.,1.),(1.,1.),(1.,1.),(1.,1.),(1.,1.),(1.,1.),(1.,1.),(1.,1.),(1.,
1.),(1.,1.),(1.,1.),(1.,1.),(1.,1.),(1.,1.),(1.,1.),(1.,1.),(1.,1.),(1.,
1.),(1.,1.)))
REPRESENTATION_ITEM('')
SURFACE()
);
#74=(
BOUNDED_SURFACE()
B_SPLINE_SURFACE(5,1,((#49708,#49709),(#49710,#49711),(#49712,#49713),(#49714,
#49715),(#49716,#49717),(#49718,#49719),(#49720,#49721),(#49722,#49723),
(#49724,#49725),(#49726,#49727),(#49728,#49729),(#49730,#49731),(#49732,
#49733),(#49734,#49735),(#49736,#49737),(#49738,#49739),(#49740,#49741),
(#49742,#49743),(#49744,#49745),(#49746,#49747),(#49748,#49749),(#49750,
#49751),(#49752,#49753),(#49754,#49755),(#49756,#49757),(#49758,#49759),
(#49760,#49761),(#49762,#49763),(#49764,#49765),(#49766,#49767),(#49768,
#49769),(#49770,#49771),(#49772,#49773),(#49774,#49775),(#49776,#49777),
(#49778,#49779),(#49780,#49781),(#49782,#49783),(#49784,#49785),(#49786,
#49787),(#49788,#49789),(#49790,#49791),(#49792,#49793),(#49794,#49795),
(#49796,#49797),(#49798,#49799),(#49800,#49801),(#49802,#49803),(#49804,
#49805),(#49806,#49807),(#49808,#49809),(#49810,#49811),(#49812,#49813),
(#49814,#49815),(#49816,#49817),(#49818,#49819),(#49820,#49821),(#49822,
#49823),(#49824,#49825),(#49826,#49827),(#49828,#49829),(#49830,#49831),
(#49832,#49833),(#49834,#49835),(#49836,#49837),(#49838,#49839),(#49840,
#49841),(#49842,#49843),(#49844,#49845),(#49846,#49847)),.UNSPECIFIED.,
 .F.,.F.,.F.)
B_SPLINE_SURFACE_WITH_KNOTS((6,1,1,1,1,1,1,1,1,1,1,1,1,1,1,1,1,1,1,1,1,
1,1,1,1,1,1,1,1,1,1,1,1,1,1,1,1,1,1,1,1,1,1,1,1,1,1,1,1,1,1,1,1,1,1,1,1,
1,1,1,1,1,1,1,1,6),(2,2),(-1.,-0.984615384615383,-0.969230769230768,-0.953846153846152,
-0.938461538461537,-0.923076923076922,-0.907692307692306,-0.892307692307691,
-0.876923076923076,-0.86153846153846,-0.846153846153845,-0.83076923076923,
-0.815384615384614,-0.799999999999999,-0.784615384615384,-0.769230769230768,
-0.753846153846153,-0.738461538461538,-0.723076923076922,-0.707692307692307,
-0.692307692307692,-0.676923076923076,-0.661538461538461,-0.646153846153846,
-0.63076923076923,-0.615384615384615,-0.6,-0.584615384615384,-0.569230769230769,
-0.553846153846154,-0.538461538461538,-0.523076923076923,-0.507692307692308,
-0.492307692307692,-0.476923076923077,-0.461538461538462,-0.446153846153846,
-0.430769230769231,-0.415384615384615,-0.4,-0.384615384615385,-0.369230769230769,
-0.353846153846154,-0.338461538461538,-0.323076923076923,-0.307692307692308,
-0.292307692307692,-0.276923076923077,-0.261538461538462,-0.246153846153846,
-0.230769230769231,-0.215384615384615,-0.2,-0.184615384615385,-0.169230769230769,
-0.153846153846154,-0.138461538461538,-0.123076923076923,-0.107692307692308,
-0.0923076923076923,-0.0769230769230769,-0.0615384615384615,-0.0461538461538462,
-0.0307692307692308,-0.0153846153846154,0.),(-1.,1.),.UNSPECIFIED.)
GEOMETRIC_REPRESENTATION_ITEM()
RATIONAL_B_SPLINE_SURFACE(((1.,1.),(1.,1.),(1.,1.),(1.,1.),(1.,1.),(1.,
1.),(1.,1.),(1.,1.),(1.,1.),(1.,1.),(1.,1.),(1.,1.),(1.,1.),(1.,1.),(1.,
1.),(1.,1.),(1.,1.),(1.,1.),(1.,1.),(1.,1.),(1.,1.),(1.,1.),(1.,1.),(1.,
1.),(1.,1.),(1.,1.),(1.,1.),(1.,1.),(1.,1.),(1.,1.),(1.,1.),(1.,1.),(1.,
1.),(1.,1.),(1.,1.),(1.,1.),(1.,1.),(1.,1.),(1.,1.),(1.,1.),(1.,1.),(1.,
1.),(1.,1.),(1.,1.),(1.,1.),(1.,1.),(1.,1.),(1.,1.),(1.,1.),(1.,1.),(1.,
1.),(1.,1.),(1.,1.),(1.,1.),(1.,1.),(1.,1.),(1.,1.),(1.,1.),(1.,1.),(1.,
1.),(1.,1.),(1.,1.),(1.,1.),(1.,1.),(1.,1.),(1.,1.),(1.,1.),(1.,1.),(1.,
1.),(1.,1.)))
REPRESENTATION_ITEM('')
SURFACE()
);
#75=(
BOUNDED_SURFACE()
B_SPLINE_SURFACE(5,1,((#49938,#49939),(#49940,#49941),(#49942,#49943),(#49944,
#49945),(#49946,#49947),(#49948,#49949),(#49950,#49951),(#49952,#49953),
(#49954,#49955),(#49956,#49957),(#49958,#49959),(#49960,#49961),(#49962,
#49963),(#49964,#49965),(#49966,#49967),(#49968,#49969),(#49970,#49971),
(#49972,#49973),(#49974,#49975),(#49976,#49977),(#49978,#49979),(#49980,
#49981),(#49982,#49983),(#49984,#49985),(#49986,#49987),(#49988,#49989),
(#49990,#49991),(#49992,#49993),(#49994,#49995),(#49996,#49997),(#49998,
#49999),(#50000,#50001),(#50002,#50003),(#50004,#50005),(#50006,#50007),
(#50008,#50009),(#50010,#50011),(#50012,#50013),(#50014,#50015),(#50016,
#50017),(#50018,#50019),(#50020,#50021),(#50022,#50023),(#50024,#50025),
(#50026,#50027),(#50028,#50029),(#50030,#50031),(#50032,#50033),(#50034,
#50035),(#50036,#50037),(#50038,#50039),(#50040,#50041),(#50042,#50043),
(#50044,#50045),(#50046,#50047),(#50048,#50049),(#50050,#50051),(#50052,
#50053),(#50054,#50055),(#50056,#50057),(#50058,#50059),(#50060,#50061),
(#50062,#50063),(#50064,#50065),(#50066,#50067),(#50068,#50069),(#50070,
#50071),(#50072,#50073),(#50074,#50075),(#50076,#50077)),.UNSPECIFIED.,
 .F.,.F.,.F.)
B_SPLINE_SURFACE_WITH_KNOTS((6,1,1,1,1,1,1,1,1,1,1,1,1,1,1,1,1,1,1,1,1,
1,1,1,1,1,1,1,1,1,1,1,1,1,1,1,1,1,1,1,1,1,1,1,1,1,1,1,1,1,1,1,1,1,1,1,1,
1,1,1,1,1,1,1,1,6),(2,2),(-1.,-0.984615384615383,-0.969230769230768,-0.953846153846152,
-0.938461538461537,-0.923076923076922,-0.907692307692306,-0.892307692307691,
-0.876923076923076,-0.86153846153846,-0.846153846153845,-0.83076923076923,
-0.815384615384614,-0.799999999999999,-0.784615384615384,-0.769230769230768,
-0.753846153846153,-0.738461538461538,-0.723076923076922,-0.707692307692307,
-0.692307692307692,-0.676923076923076,-0.661538461538461,-0.646153846153846,
-0.63076923076923,-0.615384615384615,-0.6,-0.584615384615384,-0.569230769230769,
-0.553846153846154,-0.538461538461538,-0.523076923076923,-0.507692307692308,
-0.492307692307692,-0.476923076923077,-0.461538461538462,-0.446153846153846,
-0.430769230769231,-0.415384615384615,-0.4,-0.384615384615385,-0.369230769230769,
-0.353846153846154,-0.338461538461538,-0.323076923076923,-0.307692307692308,
-0.292307692307692,-0.276923076923077,-0.261538461538462,-0.246153846153846,
-0.230769230769231,-0.215384615384615,-0.2,-0.184615384615385,-0.169230769230769,
-0.153846153846154,-0.138461538461538,-0.123076923076923,-0.107692307692308,
-0.0923076923076923,-0.0769230769230769,-0.0615384615384615,-0.0461538461538462,
-0.0307692307692308,-0.0153846153846154,0.),(-1.,1.),.UNSPECIFIED.)
GEOMETRIC_REPRESENTATION_ITEM()
RATIONAL_B_SPLINE_SURFACE(((1.,1.),(1.,1.),(1.,1.),(1.,1.),(1.,1.),(1.,
1.),(1.,1.),(1.,1.),(1.,1.),(1.,1.),(1.,1.),(1.,1.),(1.,1.),(1.,1.),(1.,
1.),(1.,1.),(1.,1.),(1.,1.),(1.,1.),(1.,1.),(1.,1.),(1.,1.),(1.,1.),(1.,
1.),(1.,1.),(1.,1.),(1.,1.),(1.,1.),(1.,1.),(1.,1.),(1.,1.),(1.,1.),(1.,
1.),(1.,1.),(1.,1.),(1.,1.),(1.,1.),(1.,1.),(1.,1.),(1.,1.),(1.,1.),(1.,
1.),(1.,1.),(1.,1.),(1.,1.),(1.,1.),(1.,1.),(1.,1.),(1.,1.),(1.,1.),(1.,
1.),(1.,1.),(1.,1.),(1.,1.),(1.,1.),(1.,1.),(1.,1.),(1.,1.),(1.,1.),(1.,
1.),(1.,1.),(1.,1.),(1.,1.),(1.,1.),(1.,1.),(1.,1.),(1.,1.),(1.,1.),(1.,
1.),(1.,1.)))
REPRESENTATION_ITEM('')
SURFACE()
);
#76=(
BOUNDED_SURFACE()
B_SPLINE_SURFACE(5,1,((#50150,#50151),(#50152,#50153),(#50154,#50155),(#50156,
#50157),(#50158,#50159),(#50160,#50161),(#50162,#50163),(#50164,#50165),
(#50166,#50167),(#50168,#50169),(#50170,#50171),(#50172,#50173),(#50174,
#50175),(#50176,#50177),(#50178,#50179),(#50180,#50181),(#50182,#50183),
(#50184,#50185),(#50186,#50187),(#50188,#50189),(#50190,#50191),(#50192,
#50193),(#50194,#50195),(#50196,#50197),(#50198,#50199),(#50200,#50201),
(#50202,#50203),(#50204,#50205),(#50206,#50207),(#50208,#50209),(#50210,
#50211),(#50212,#50213),(#50214,#50215),(#50216,#50217),(#50218,#50219),
(#50220,#50221),(#50222,#50223),(#50224,#50225),(#50226,#50227),(#50228,
#50229),(#50230,#50231),(#50232,#50233),(#50234,#50235),(#50236,#50237),
(#50238,#50239),(#50240,#50241),(#50242,#50243),(#50244,#50245),(#50246,
#50247),(#50248,#50249),(#50250,#50251),(#50252,#50253),(#50254,#50255),
(#50256,#50257),(#50258,#50259),(#50260,#50261),(#50262,#50263),(#50264,
#50265),(#50266,#50267),(#50268,#50269),(#50270,#50271),(#50272,#50273),
(#50274,#50275),(#50276,#50277),(#50278,#50279),(#50280,#50281),(#50282,
#50283),(#50284,#50285),(#50286,#50287),(#50288,#50289)),.UNSPECIFIED.,
 .F.,.F.,.F.)
B_SPLINE_SURFACE_WITH_KNOTS((6,1,1,1,1,1,1,1,1,1,1,1,1,1,1,1,1,1,1,1,1,
1,1,1,1,1,1,1,1,1,1,1,1,1,1,1,1,1,1,1,1,1,1,1,1,1,1,1,1,1,1,1,1,1,1,1,1,
1,1,1,1,1,1,1,1,6),(2,2),(-1.,-0.984615384615383,-0.969230769230768,-0.953846153846152,
-0.938461538461537,-0.923076923076922,-0.907692307692306,-0.892307692307691,
-0.876923076923076,-0.86153846153846,-0.846153846153845,-0.83076923076923,
-0.815384615384614,-0.799999999999999,-0.784615384615384,-0.769230769230768,
-0.753846153846153,-0.738461538461538,-0.723076923076922,-0.707692307692307,
-0.692307692307692,-0.676923076923076,-0.661538461538461,-0.646153846153846,
-0.63076923076923,-0.615384615384615,-0.6,-0.584615384615384,-0.569230769230769,
-0.553846153846154,-0.538461538461538,-0.523076923076923,-0.507692307692308,
-0.492307692307692,-0.476923076923077,-0.461538461538462,-0.446153846153846,
-0.430769230769231,-0.415384615384615,-0.4,-0.384615384615385,-0.369230769230769,
-0.353846153846154,-0.338461538461538,-0.323076923076923,-0.307692307692308,
-0.292307692307692,-0.276923076923077,-0.261538461538462,-0.246153846153846,
-0.230769230769231,-0.215384615384615,-0.2,-0.184615384615385,-0.169230769230769,
-0.153846153846154,-0.138461538461538,-0.123076923076923,-0.107692307692308,
-0.0923076923076923,-0.0769230769230769,-0.0615384615384615,-0.0461538461538462,
-0.0307692307692308,-0.0153846153846154,0.),(-1.,1.),.UNSPECIFIED.)
GEOMETRIC_REPRESENTATION_ITEM()
RATIONAL_B_SPLINE_SURFACE(((1.,1.),(1.,1.),(1.,1.),(1.,1.),(1.,1.),(1.,
1.),(1.,1.),(1.,1.),(1.,1.),(1.,1.),(1.,1.),(1.,1.),(1.,1.),(1.,1.),(1.,
1.),(1.,1.),(1.,1.),(1.,1.),(1.,1.),(1.,1.),(1.,1.),(1.,1.),(1.,1.),(1.,
1.),(1.,1.),(1.,1.),(1.,1.),(1.,1.),(1.,1.),(1.,1.),(1.,1.),(1.,1.),(1.,
1.),(1.,1.),(1.,1.),(1.,1.),(1.,1.),(1.,1.),(1.,1.),(1.,1.),(1.,1.),(1.,
1.),(1.,1.),(1.,1.),(1.,1.),(1.,1.),(1.,1.),(1.,1.),(1.,1.),(1.,1.),(1.,
1.),(1.,1.),(1.,1.),(1.,1.),(1.,1.),(1.,1.),(1.,1.),(1.,1.),(1.,1.),(1.,
1.),(1.,1.),(1.,1.),(1.,1.),(1.,1.),(1.,1.),(1.,1.),(1.,1.),(1.,1.),(1.,
1.),(1.,1.)))
REPRESENTATION_ITEM('')
SURFACE()
);
#77=(
BOUNDED_SURFACE()
B_SPLINE_SURFACE(5,1,((#50380,#50381),(#50382,#50383),(#50384,#50385),(#50386,
#50387),(#50388,#50389),(#50390,#50391),(#50392,#50393),(#50394,#50395),
(#50396,#50397),(#50398,#50399),(#50400,#50401),(#50402,#50403),(#50404,
#50405),(#50406,#50407),(#50408,#50409),(#50410,#50411),(#50412,#50413),
(#50414,#50415),(#50416,#50417),(#50418,#50419),(#50420,#50421),(#50422,
#50423),(#50424,#50425),(#50426,#50427),(#50428,#50429),(#50430,#50431),
(#50432,#50433),(#50434,#50435),(#50436,#50437),(#50438,#50439),(#50440,
#50441),(#50442,#50443),(#50444,#50445),(#50446,#50447),(#50448,#50449),
(#50450,#50451),(#50452,#50453),(#50454,#50455),(#50456,#50457),(#50458,
#50459),(#50460,#50461),(#50462,#50463),(#50464,#50465),(#50466,#50467),
(#50468,#50469),(#50470,#50471),(#50472,#50473),(#50474,#50475),(#50476,
#50477),(#50478,#50479),(#50480,#50481),(#50482,#50483),(#50484,#50485),
(#50486,#50487),(#50488,#50489),(#50490,#50491),(#50492,#50493),(#50494,
#50495),(#50496,#50497),(#50498,#50499),(#50500,#50501),(#50502,#50503),
(#50504,#50505),(#50506,#50507),(#50508,#50509),(#50510,#50511),(#50512,
#50513),(#50514,#50515),(#50516,#50517),(#50518,#50519)),.UNSPECIFIED.,
 .F.,.F.,.F.)
B_SPLINE_SURFACE_WITH_KNOTS((6,1,1,1,1,1,1,1,1,1,1,1,1,1,1,1,1,1,1,1,1,
1,1,1,1,1,1,1,1,1,1,1,1,1,1,1,1,1,1,1,1,1,1,1,1,1,1,1,1,1,1,1,1,1,1,1,1,
1,1,1,1,1,1,1,1,6),(2,2),(-1.,-0.984615384615383,-0.969230769230768,-0.953846153846152,
-0.938461538461537,-0.923076923076922,-0.907692307692306,-0.892307692307691,
-0.876923076923076,-0.86153846153846,-0.846153846153845,-0.83076923076923,
-0.815384615384614,-0.799999999999999,-0.784615384615384,-0.769230769230768,
-0.753846153846153,-0.738461538461538,-0.723076923076922,-0.707692307692307,
-0.692307692307692,-0.676923076923076,-0.661538461538461,-0.646153846153846,
-0.63076923076923,-0.615384615384615,-0.6,-0.584615384615384,-0.569230769230769,
-0.553846153846154,-0.538461538461538,-0.523076923076923,-0.507692307692308,
-0.492307692307692,-0.476923076923077,-0.461538461538462,-0.446153846153846,
-0.430769230769231,-0.415384615384615,-0.4,-0.384615384615385,-0.369230769230769,
-0.353846153846154,-0.338461538461538,-0.323076923076923,-0.307692307692308,
-0.292307692307692,-0.276923076923077,-0.261538461538462,-0.246153846153846,
-0.230769230769231,-0.215384615384615,-0.2,-0.184615384615385,-0.169230769230769,
-0.153846153846154,-0.138461538461538,-0.123076923076923,-0.107692307692308,
-0.0923076923076923,-0.0769230769230769,-0.0615384615384615,-0.0461538461538462,
-0.0307692307692308,-0.0153846153846154,0.),(-1.,1.),.UNSPECIFIED.)
GEOMETRIC_REPRESENTATION_ITEM()
RATIONAL_B_SPLINE_SURFACE(((1.,1.),(1.,1.),(1.,1.),(1.,1.),(1.,1.),(1.,
1.),(1.,1.),(1.,1.),(1.,1.),(1.,1.),(1.,1.),(1.,1.),(1.,1.),(1.,1.),(1.,
1.),(1.,1.),(1.,1.),(1.,1.),(1.,1.),(1.,1.),(1.,1.),(1.,1.),(1.,1.),(1.,
1.),(1.,1.),(1.,1.),(1.,1.),(1.,1.),(1.,1.),(1.,1.),(1.,1.),(1.,1.),(1.,
1.),(1.,1.),(1.,1.),(1.,1.),(1.,1.),(1.,1.),(1.,1.),(1.,1.),(1.,1.),(1.,
1.),(1.,1.),(1.,1.),(1.,1.),(1.,1.),(1.,1.),(1.,1.),(1.,1.),(1.,1.),(1.,
1.),(1.,1.),(1.,1.),(1.,1.),(1.,1.),(1.,1.),(1.,1.),(1.,1.),(1.,1.),(1.,
1.),(1.,1.),(1.,1.),(1.,1.),(1.,1.),(1.,1.),(1.,1.),(1.,1.),(1.,1.),(1.,
1.),(1.,1.)))
REPRESENTATION_ITEM('')
SURFACE()
);
#78=(
BOUNDED_SURFACE()
B_SPLINE_SURFACE(5,1,((#50592,#50593),(#50594,#50595),(#50596,#50597),(#50598,
#50599),(#50600,#50601),(#50602,#50603),(#50604,#50605),(#50606,#50607),
(#50608,#50609),(#50610,#50611),(#50612,#50613),(#50614,#50615),(#50616,
#50617),(#50618,#50619),(#50620,#50621),(#50622,#50623),(#50624,#50625),
(#50626,#50627),(#50628,#50629),(#50630,#50631),(#50632,#50633),(#50634,
#50635),(#50636,#50637),(#50638,#50639),(#50640,#50641),(#50642,#50643),
(#50644,#50645),(#50646,#50647),(#50648,#50649),(#50650,#50651),(#50652,
#50653),(#50654,#50655),(#50656,#50657),(#50658,#50659),(#50660,#50661),
(#50662,#50663),(#50664,#50665),(#50666,#50667),(#50668,#50669),(#50670,
#50671),(#50672,#50673),(#50674,#50675),(#50676,#50677),(#50678,#50679),
(#50680,#50681),(#50682,#50683),(#50684,#50685),(#50686,#50687),(#50688,
#50689),(#50690,#50691),(#50692,#50693),(#50694,#50695),(#50696,#50697),
(#50698,#50699),(#50700,#50701),(#50702,#50703),(#50704,#50705),(#50706,
#50707),(#50708,#50709),(#50710,#50711),(#50712,#50713),(#50714,#50715),
(#50716,#50717),(#50718,#50719),(#50720,#50721),(#50722,#50723),(#50724,
#50725),(#50726,#50727),(#50728,#50729),(#50730,#50731)),.UNSPECIFIED.,
 .F.,.F.,.F.)
B_SPLINE_SURFACE_WITH_KNOTS((6,1,1,1,1,1,1,1,1,1,1,1,1,1,1,1,1,1,1,1,1,
1,1,1,1,1,1,1,1,1,1,1,1,1,1,1,1,1,1,1,1,1,1,1,1,1,1,1,1,1,1,1,1,1,1,1,1,
1,1,1,1,1,1,1,1,6),(2,2),(-1.,-0.984615384615383,-0.969230769230768,-0.953846153846152,
-0.938461538461537,-0.923076923076922,-0.907692307692306,-0.892307692307691,
-0.876923076923076,-0.86153846153846,-0.846153846153845,-0.83076923076923,
-0.815384615384614,-0.799999999999999,-0.784615384615384,-0.769230769230768,
-0.753846153846153,-0.738461538461538,-0.723076923076922,-0.707692307692307,
-0.692307692307692,-0.676923076923076,-0.661538461538461,-0.646153846153846,
-0.63076923076923,-0.615384615384615,-0.6,-0.584615384615384,-0.569230769230769,
-0.553846153846154,-0.538461538461538,-0.523076923076923,-0.507692307692308,
-0.492307692307692,-0.476923076923077,-0.461538461538462,-0.446153846153846,
-0.430769230769231,-0.415384615384615,-0.4,-0.384615384615385,-0.369230769230769,
-0.353846153846154,-0.338461538461538,-0.323076923076923,-0.307692307692308,
-0.292307692307692,-0.276923076923077,-0.261538461538462,-0.246153846153846,
-0.230769230769231,-0.215384615384615,-0.2,-0.184615384615385,-0.169230769230769,
-0.153846153846154,-0.138461538461538,-0.123076923076923,-0.107692307692308,
-0.0923076923076923,-0.0769230769230769,-0.0615384615384615,-0.0461538461538462,
-0.0307692307692308,-0.0153846153846154,0.),(-1.,1.),.UNSPECIFIED.)
GEOMETRIC_REPRESENTATION_ITEM()
RATIONAL_B_SPLINE_SURFACE(((1.,1.),(1.,1.),(1.,1.),(1.,1.),(1.,1.),(1.,
1.),(1.,1.),(1.,1.),(1.,1.),(1.,1.),(1.,1.),(1.,1.),(1.,1.),(1.,1.),(1.,
1.),(1.,1.),(1.,1.),(1.,1.),(1.,1.),(1.,1.),(1.,1.),(1.,1.),(1.,1.),(1.,
1.),(1.,1.),(1.,1.),(1.,1.),(1.,1.),(1.,1.),(1.,1.),(1.,1.),(1.,1.),(1.,
1.),(1.,1.),(1.,1.),(1.,1.),(1.,1.),(1.,1.),(1.,1.),(1.,1.),(1.,1.),(1.,
1.),(1.,1.),(1.,1.),(1.,1.),(1.,1.),(1.,1.),(1.,1.),(1.,1.),(1.,1.),(1.,
1.),(1.,1.),(1.,1.),(1.,1.),(1.,1.),(1.,1.),(1.,1.),(1.,1.),(1.,1.),(1.,
1.),(1.,1.),(1.,1.),(1.,1.),(1.,1.),(1.,1.),(1.,1.),(1.,1.),(1.,1.),(1.,
1.),(1.,1.)))
REPRESENTATION_ITEM('')
SURFACE()
);
#79=(
BOUNDED_SURFACE()
B_SPLINE_SURFACE(5,1,((#50822,#50823),(#50824,#50825),(#50826,#50827),(#50828,
#50829),(#50830,#50831),(#50832,#50833),(#50834,#50835),(#50836,#50837),
(#50838,#50839),(#50840,#50841),(#50842,#50843),(#50844,#50845),(#50846,
#50847),(#50848,#50849),(#50850,#50851),(#50852,#50853),(#50854,#50855),
(#50856,#50857),(#50858,#50859),(#50860,#50861),(#50862,#50863),(#50864,
#50865),(#50866,#50867),(#50868,#50869),(#50870,#50871),(#50872,#50873),
(#50874,#50875),(#50876,#50877),(#50878,#50879),(#50880,#50881),(#50882,
#50883),(#50884,#50885),(#50886,#50887),(#50888,#50889),(#50890,#50891),
(#50892,#50893),(#50894,#50895),(#50896,#50897),(#50898,#50899),(#50900,
#50901),(#50902,#50903),(#50904,#50905),(#50906,#50907),(#50908,#50909),
(#50910,#50911),(#50912,#50913),(#50914,#50915),(#50916,#50917),(#50918,
#50919),(#50920,#50921),(#50922,#50923),(#50924,#50925),(#50926,#50927),
(#50928,#50929),(#50930,#50931),(#50932,#50933),(#50934,#50935),(#50936,
#50937),(#50938,#50939),(#50940,#50941),(#50942,#50943),(#50944,#50945),
(#50946,#50947),(#50948,#50949),(#50950,#50951),(#50952,#50953),(#50954,
#50955),(#50956,#50957),(#50958,#50959),(#50960,#50961)),.UNSPECIFIED.,
 .F.,.F.,.F.)
B_SPLINE_SURFACE_WITH_KNOTS((6,1,1,1,1,1,1,1,1,1,1,1,1,1,1,1,1,1,1,1,1,
1,1,1,1,1,1,1,1,1,1,1,1,1,1,1,1,1,1,1,1,1,1,1,1,1,1,1,1,1,1,1,1,1,1,1,1,
1,1,1,1,1,1,1,1,6),(2,2),(-1.,-0.984615384615383,-0.969230769230768,-0.953846153846152,
-0.938461538461537,-0.923076923076922,-0.907692307692306,-0.892307692307691,
-0.876923076923076,-0.86153846153846,-0.846153846153845,-0.83076923076923,
-0.815384615384614,-0.799999999999999,-0.784615384615384,-0.769230769230768,
-0.753846153846153,-0.738461538461538,-0.723076923076922,-0.707692307692307,
-0.692307692307692,-0.676923076923076,-0.661538461538461,-0.646153846153846,
-0.63076923076923,-0.615384615384615,-0.6,-0.584615384615384,-0.569230769230769,
-0.553846153846154,-0.538461538461538,-0.523076923076923,-0.507692307692308,
-0.492307692307692,-0.476923076923077,-0.461538461538462,-0.446153846153846,
-0.430769230769231,-0.415384615384615,-0.4,-0.384615384615385,-0.369230769230769,
-0.353846153846154,-0.338461538461538,-0.323076923076923,-0.307692307692308,
-0.292307692307692,-0.276923076923077,-0.261538461538462,-0.246153846153846,
-0.230769230769231,-0.215384615384615,-0.2,-0.184615384615385,-0.169230769230769,
-0.153846153846154,-0.138461538461538,-0.123076923076923,-0.107692307692308,
-0.0923076923076923,-0.0769230769230769,-0.0615384615384615,-0.0461538461538462,
-0.0307692307692308,-0.0153846153846154,0.),(-1.,1.),.UNSPECIFIED.)
GEOMETRIC_REPRESENTATION_ITEM()
RATIONAL_B_SPLINE_SURFACE(((1.,1.),(1.,1.),(1.,1.),(1.,1.),(1.,1.),(1.,
1.),(1.,1.),(1.,1.),(1.,1.),(1.,1.),(1.,1.),(1.,1.),(1.,1.),(1.,1.),(1.,
1.),(1.,1.),(1.,1.),(1.,1.),(1.,1.),(1.,1.),(1.,1.),(1.,1.),(1.,1.),(1.,
1.),(1.,1.),(1.,1.),(1.,1.),(1.,1.),(1.,1.),(1.,1.),(1.,1.),(1.,1.),(1.,
1.),(1.,1.),(1.,1.),(1.,1.),(1.,1.),(1.,1.),(1.,1.),(1.,1.),(1.,1.),(1.,
1.),(1.,1.),(1.,1.),(1.,1.),(1.,1.),(1.,1.),(1.,1.),(1.,1.),(1.,1.),(1.,
1.),(1.,1.),(1.,1.),(1.,1.),(1.,1.),(1.,1.),(1.,1.),(1.,1.),(1.,1.),(1.,
1.),(1.,1.),(1.,1.),(1.,1.),(1.,1.),(1.,1.),(1.,1.),(1.,1.),(1.,1.),(1.,
1.),(1.,1.)))
REPRESENTATION_ITEM('')
SURFACE()
);
#80=(
BOUNDED_SURFACE()
B_SPLINE_SURFACE(5,1,((#51034,#51035),(#51036,#51037),(#51038,#51039),(#51040,
#51041),(#51042,#51043),(#51044,#51045),(#51046,#51047),(#51048,#51049),
(#51050,#51051),(#51052,#51053),(#51054,#51055),(#51056,#51057),(#51058,
#51059),(#51060,#51061),(#51062,#51063),(#51064,#51065),(#51066,#51067),
(#51068,#51069),(#51070,#51071),(#51072,#51073),(#51074,#51075),(#51076,
#51077),(#51078,#51079),(#51080,#51081),(#51082,#51083),(#51084,#51085),
(#51086,#51087),(#51088,#51089),(#51090,#51091),(#51092,#51093),(#51094,
#51095),(#51096,#51097),(#51098,#51099),(#51100,#51101),(#51102,#51103),
(#51104,#51105),(#51106,#51107),(#51108,#51109),(#51110,#51111),(#51112,
#51113),(#51114,#51115),(#51116,#51117),(#51118,#51119),(#51120,#51121),
(#51122,#51123),(#51124,#51125),(#51126,#51127),(#51128,#51129),(#51130,
#51131),(#51132,#51133),(#51134,#51135),(#51136,#51137),(#51138,#51139),
(#51140,#51141),(#51142,#51143),(#51144,#51145),(#51146,#51147),(#51148,
#51149),(#51150,#51151),(#51152,#51153),(#51154,#51155),(#51156,#51157),
(#51158,#51159),(#51160,#51161),(#51162,#51163),(#51164,#51165),(#51166,
#51167),(#51168,#51169),(#51170,#51171),(#51172,#51173)),.UNSPECIFIED.,
 .F.,.F.,.F.)
B_SPLINE_SURFACE_WITH_KNOTS((6,1,1,1,1,1,1,1,1,1,1,1,1,1,1,1,1,1,1,1,1,
1,1,1,1,1,1,1,1,1,1,1,1,1,1,1,1,1,1,1,1,1,1,1,1,1,1,1,1,1,1,1,1,1,1,1,1,
1,1,1,1,1,1,1,1,6),(2,2),(-1.,-0.984615384615383,-0.969230769230768,-0.953846153846152,
-0.938461538461537,-0.923076923076922,-0.907692307692306,-0.892307692307691,
-0.876923076923076,-0.86153846153846,-0.846153846153845,-0.83076923076923,
-0.815384615384614,-0.799999999999999,-0.784615384615384,-0.769230769230768,
-0.753846153846153,-0.738461538461538,-0.723076923076922,-0.707692307692307,
-0.692307692307692,-0.676923076923076,-0.661538461538461,-0.646153846153846,
-0.63076923076923,-0.615384615384615,-0.6,-0.584615384615384,-0.569230769230769,
-0.553846153846154,-0.538461538461538,-0.523076923076923,-0.507692307692308,
-0.492307692307692,-0.476923076923077,-0.461538461538462,-0.446153846153846,
-0.430769230769231,-0.415384615384615,-0.4,-0.384615384615385,-0.369230769230769,
-0.353846153846154,-0.338461538461538,-0.323076923076923,-0.307692307692308,
-0.292307692307692,-0.276923076923077,-0.261538461538462,-0.246153846153846,
-0.230769230769231,-0.215384615384615,-0.2,-0.184615384615385,-0.169230769230769,
-0.153846153846154,-0.138461538461538,-0.123076923076923,-0.107692307692308,
-0.0923076923076923,-0.0769230769230769,-0.0615384615384615,-0.0461538461538462,
-0.0307692307692308,-0.0153846153846154,0.),(-1.,1.),.UNSPECIFIED.)
GEOMETRIC_REPRESENTATION_ITEM()
RATIONAL_B_SPLINE_SURFACE(((1.,1.),(1.,1.),(1.,1.),(1.,1.),(1.,1.),(1.,
1.),(1.,1.),(1.,1.),(1.,1.),(1.,1.),(1.,1.),(1.,1.),(1.,1.),(1.,1.),(1.,
1.),(1.,1.),(1.,1.),(1.,1.),(1.,1.),(1.,1.),(1.,1.),(1.,1.),(1.,1.),(1.,
1.),(1.,1.),(1.,1.),(1.,1.),(1.,1.),(1.,1.),(1.,1.),(1.,1.),(1.,1.),(1.,
1.),(1.,1.),(1.,1.),(1.,1.),(1.,1.),(1.,1.),(1.,1.),(1.,1.),(1.,1.),(1.,
1.),(1.,1.),(1.,1.),(1.,1.),(1.,1.),(1.,1.),(1.,1.),(1.,1.),(1.,1.),(1.,
1.),(1.,1.),(1.,1.),(1.,1.),(1.,1.),(1.,1.),(1.,1.),(1.,1.),(1.,1.),(1.,
1.),(1.,1.),(1.,1.),(1.,1.),(1.,1.),(1.,1.),(1.,1.),(1.,1.),(1.,1.),(1.,
1.),(1.,1.)))
REPRESENTATION_ITEM('')
SURFACE()
);
#81=(
BOUNDED_SURFACE()
B_SPLINE_SURFACE(5,1,((#51264,#51265),(#51266,#51267),(#51268,#51269),(#51270,
#51271),(#51272,#51273),(#51274,#51275),(#51276,#51277),(#51278,#51279),
(#51280,#51281),(#51282,#51283),(#51284,#51285),(#51286,#51287),(#51288,
#51289),(#51290,#51291),(#51292,#51293),(#51294,#51295),(#51296,#51297),
(#51298,#51299),(#51300,#51301),(#51302,#51303),(#51304,#51305),(#51306,
#51307),(#51308,#51309),(#51310,#51311),(#51312,#51313),(#51314,#51315),
(#51316,#51317),(#51318,#51319),(#51320,#51321),(#51322,#51323),(#51324,
#51325),(#51326,#51327),(#51328,#51329),(#51330,#51331),(#51332,#51333),
(#51334,#51335),(#51336,#51337),(#51338,#51339),(#51340,#51341),(#51342,
#51343),(#51344,#51345),(#51346,#51347),(#51348,#51349),(#51350,#51351),
(#51352,#51353),(#51354,#51355),(#51356,#51357),(#51358,#51359),(#51360,
#51361),(#51362,#51363),(#51364,#51365),(#51366,#51367),(#51368,#51369),
(#51370,#51371),(#51372,#51373),(#51374,#51375),(#51376,#51377),(#51378,
#51379),(#51380,#51381),(#51382,#51383),(#51384,#51385),(#51386,#51387),
(#51388,#51389),(#51390,#51391),(#51392,#51393),(#51394,#51395),(#51396,
#51397),(#51398,#51399),(#51400,#51401),(#51402,#51403)),.UNSPECIFIED.,
 .F.,.F.,.F.)
B_SPLINE_SURFACE_WITH_KNOTS((6,1,1,1,1,1,1,1,1,1,1,1,1,1,1,1,1,1,1,1,1,
1,1,1,1,1,1,1,1,1,1,1,1,1,1,1,1,1,1,1,1,1,1,1,1,1,1,1,1,1,1,1,1,1,1,1,1,
1,1,1,1,1,1,1,1,6),(2,2),(-1.,-0.984615384615383,-0.969230769230768,-0.953846153846152,
-0.938461538461537,-0.923076923076922,-0.907692307692306,-0.892307692307691,
-0.876923076923076,-0.86153846153846,-0.846153846153845,-0.83076923076923,
-0.815384615384614,-0.799999999999999,-0.784615384615384,-0.769230769230768,
-0.753846153846153,-0.738461538461538,-0.723076923076922,-0.707692307692307,
-0.692307692307692,-0.676923076923076,-0.661538461538461,-0.646153846153846,
-0.63076923076923,-0.615384615384615,-0.6,-0.584615384615384,-0.569230769230769,
-0.553846153846154,-0.538461538461538,-0.523076923076923,-0.507692307692308,
-0.492307692307692,-0.476923076923077,-0.461538461538462,-0.446153846153846,
-0.430769230769231,-0.415384615384615,-0.4,-0.384615384615385,-0.369230769230769,
-0.353846153846154,-0.338461538461538,-0.323076923076923,-0.307692307692308,
-0.292307692307692,-0.276923076923077,-0.261538461538462,-0.246153846153846,
-0.230769230769231,-0.215384615384615,-0.2,-0.184615384615385,-0.169230769230769,
-0.153846153846154,-0.138461538461538,-0.123076923076923,-0.107692307692308,
-0.0923076923076923,-0.0769230769230769,-0.0615384615384615,-0.0461538461538462,
-0.0307692307692308,-0.0153846153846154,0.),(-1.,1.),.UNSPECIFIED.)
GEOMETRIC_REPRESENTATION_ITEM()
RATIONAL_B_SPLINE_SURFACE(((1.,1.),(1.,1.),(1.,1.),(1.,1.),(1.,1.),(1.,
1.),(1.,1.),(1.,1.),(1.,1.),(1.,1.),(1.,1.),(1.,1.),(1.,1.),(1.,1.),(1.,
1.),(1.,1.),(1.,1.),(1.,1.),(1.,1.),(1.,1.),(1.,1.),(1.,1.),(1.,1.),(1.,
1.),(1.,1.),(1.,1.),(1.,1.),(1.,1.),(1.,1.),(1.,1.),(1.,1.),(1.,1.),(1.,
1.),(1.,1.),(1.,1.),(1.,1.),(1.,1.),(1.,1.),(1.,1.),(1.,1.),(1.,1.),(1.,
1.),(1.,1.),(1.,1.),(1.,1.),(1.,1.),(1.,1.),(1.,1.),(1.,1.),(1.,1.),(1.,
1.),(1.,1.),(1.,1.),(1.,1.),(1.,1.),(1.,1.),(1.,1.),(1.,1.),(1.,1.),(1.,
1.),(1.,1.),(1.,1.),(1.,1.),(1.,1.),(1.,1.),(1.,1.),(1.,1.),(1.,1.),(1.,
1.),(1.,1.)))
REPRESENTATION_ITEM('')
SURFACE()
);
#82=(
BOUNDED_SURFACE()
B_SPLINE_SURFACE(5,1,((#51476,#51477),(#51478,#51479),(#51480,#51481),(#51482,
#51483),(#51484,#51485),(#51486,#51487),(#51488,#51489),(#51490,#51491),
(#51492,#51493),(#51494,#51495),(#51496,#51497),(#51498,#51499),(#51500,
#51501),(#51502,#51503),(#51504,#51505),(#51506,#51507),(#51508,#51509),
(#51510,#51511),(#51512,#51513),(#51514,#51515),(#51516,#51517),(#51518,
#51519),(#51520,#51521),(#51522,#51523),(#51524,#51525),(#51526,#51527),
(#51528,#51529),(#51530,#51531),(#51532,#51533),(#51534,#51535),(#51536,
#51537),(#51538,#51539),(#51540,#51541),(#51542,#51543),(#51544,#51545),
(#51546,#51547),(#51548,#51549),(#51550,#51551),(#51552,#51553),(#51554,
#51555),(#51556,#51557),(#51558,#51559),(#51560,#51561),(#51562,#51563),
(#51564,#51565),(#51566,#51567),(#51568,#51569),(#51570,#51571),(#51572,
#51573),(#51574,#51575),(#51576,#51577),(#51578,#51579),(#51580,#51581),
(#51582,#51583),(#51584,#51585),(#51586,#51587),(#51588,#51589),(#51590,
#51591),(#51592,#51593),(#51594,#51595),(#51596,#51597),(#51598,#51599),
(#51600,#51601),(#51602,#51603),(#51604,#51605),(#51606,#51607),(#51608,
#51609),(#51610,#51611),(#51612,#51613),(#51614,#51615)),.UNSPECIFIED.,
 .F.,.F.,.F.)
B_SPLINE_SURFACE_WITH_KNOTS((6,1,1,1,1,1,1,1,1,1,1,1,1,1,1,1,1,1,1,1,1,
1,1,1,1,1,1,1,1,1,1,1,1,1,1,1,1,1,1,1,1,1,1,1,1,1,1,1,1,1,1,1,1,1,1,1,1,
1,1,1,1,1,1,1,1,6),(2,2),(-1.,-0.984615384615383,-0.969230769230768,-0.953846153846152,
-0.938461538461537,-0.923076923076922,-0.907692307692306,-0.892307692307691,
-0.876923076923076,-0.86153846153846,-0.846153846153845,-0.83076923076923,
-0.815384615384614,-0.799999999999999,-0.784615384615384,-0.769230769230768,
-0.753846153846153,-0.738461538461538,-0.723076923076922,-0.707692307692307,
-0.692307692307692,-0.676923076923076,-0.661538461538461,-0.646153846153846,
-0.63076923076923,-0.615384615384615,-0.6,-0.584615384615384,-0.569230769230769,
-0.553846153846154,-0.538461538461538,-0.523076923076923,-0.507692307692308,
-0.492307692307692,-0.476923076923077,-0.461538461538462,-0.446153846153846,
-0.430769230769231,-0.415384615384615,-0.4,-0.384615384615385,-0.369230769230769,
-0.353846153846154,-0.338461538461538,-0.323076923076923,-0.307692307692308,
-0.292307692307692,-0.276923076923077,-0.261538461538462,-0.246153846153846,
-0.230769230769231,-0.215384615384615,-0.2,-0.184615384615385,-0.169230769230769,
-0.153846153846154,-0.138461538461538,-0.123076923076923,-0.107692307692308,
-0.0923076923076923,-0.0769230769230769,-0.0615384615384615,-0.0461538461538462,
-0.0307692307692308,-0.0153846153846154,0.),(-1.,1.),.UNSPECIFIED.)
GEOMETRIC_REPRESENTATION_ITEM()
RATIONAL_B_SPLINE_SURFACE(((1.,1.),(1.,1.),(1.,1.),(1.,1.),(1.,1.),(1.,
1.),(1.,1.),(1.,1.),(1.,1.),(1.,1.),(1.,1.),(1.,1.),(1.,1.),(1.,1.),(1.,
1.),(1.,1.),(1.,1.),(1.,1.),(1.,1.),(1.,1.),(1.,1.),(1.,1.),(1.,1.),(1.,
1.),(1.,1.),(1.,1.),(1.,1.),(1.,1.),(1.,1.),(1.,1.),(1.,1.),(1.,1.),(1.,
1.),(1.,1.),(1.,1.),(1.,1.),(1.,1.),(1.,1.),(1.,1.),(1.,1.),(1.,1.),(1.,
1.),(1.,1.),(1.,1.),(1.,1.),(1.,1.),(1.,1.),(1.,1.),(1.,1.),(1.,1.),(1.,
1.),(1.,1.),(1.,1.),(1.,1.),(1.,1.),(1.,1.),(1.,1.),(1.,1.),(1.,1.),(1.,
1.),(1.,1.),(1.,1.),(1.,1.),(1.,1.),(1.,1.),(1.,1.),(1.,1.),(1.,1.),(1.,
1.),(1.,1.)))
REPRESENTATION_ITEM('')
SURFACE()
);
#83=(
BOUNDED_SURFACE()
B_SPLINE_SURFACE(5,1,((#51706,#51707),(#51708,#51709),(#51710,#51711),(#51712,
#51713),(#51714,#51715),(#51716,#51717),(#51718,#51719),(#51720,#51721),
(#51722,#51723),(#51724,#51725),(#51726,#51727),(#51728,#51729),(#51730,
#51731),(#51732,#51733),(#51734,#51735),(#51736,#51737),(#51738,#51739),
(#51740,#51741),(#51742,#51743),(#51744,#51745),(#51746,#51747),(#51748,
#51749),(#51750,#51751),(#51752,#51753),(#51754,#51755),(#51756,#51757),
(#51758,#51759),(#51760,#51761),(#51762,#51763),(#51764,#51765),(#51766,
#51767),(#51768,#51769),(#51770,#51771),(#51772,#51773),(#51774,#51775),
(#51776,#51777),(#51778,#51779),(#51780,#51781),(#51782,#51783),(#51784,
#51785),(#51786,#51787),(#51788,#51789),(#51790,#51791),(#51792,#51793),
(#51794,#51795),(#51796,#51797),(#51798,#51799),(#51800,#51801),(#51802,
#51803),(#51804,#51805),(#51806,#51807),(#51808,#51809),(#51810,#51811),
(#51812,#51813),(#51814,#51815),(#51816,#51817),(#51818,#51819),(#51820,
#51821),(#51822,#51823),(#51824,#51825),(#51826,#51827),(#51828,#51829),
(#51830,#51831),(#51832,#51833),(#51834,#51835),(#51836,#51837),(#51838,
#51839),(#51840,#51841),(#51842,#51843),(#51844,#51845)),.UNSPECIFIED.,
 .F.,.F.,.F.)
B_SPLINE_SURFACE_WITH_KNOTS((6,1,1,1,1,1,1,1,1,1,1,1,1,1,1,1,1,1,1,1,1,
1,1,1,1,1,1,1,1,1,1,1,1,1,1,1,1,1,1,1,1,1,1,1,1,1,1,1,1,1,1,1,1,1,1,1,1,
1,1,1,1,1,1,1,1,6),(2,2),(-1.,-0.984615384615383,-0.969230769230768,-0.953846153846152,
-0.938461538461537,-0.923076923076922,-0.907692307692306,-0.892307692307691,
-0.876923076923076,-0.86153846153846,-0.846153846153845,-0.83076923076923,
-0.815384615384614,-0.799999999999999,-0.784615384615384,-0.769230769230768,
-0.753846153846153,-0.738461538461538,-0.723076923076922,-0.707692307692307,
-0.692307692307692,-0.676923076923076,-0.661538461538461,-0.646153846153846,
-0.63076923076923,-0.615384615384615,-0.6,-0.584615384615384,-0.569230769230769,
-0.553846153846154,-0.538461538461538,-0.523076923076923,-0.507692307692308,
-0.492307692307692,-0.476923076923077,-0.461538461538462,-0.446153846153846,
-0.430769230769231,-0.415384615384615,-0.4,-0.384615384615385,-0.369230769230769,
-0.353846153846154,-0.338461538461538,-0.323076923076923,-0.307692307692308,
-0.292307692307692,-0.276923076923077,-0.261538461538462,-0.246153846153846,
-0.230769230769231,-0.215384615384615,-0.2,-0.184615384615385,-0.169230769230769,
-0.153846153846154,-0.138461538461538,-0.123076923076923,-0.107692307692308,
-0.0923076923076923,-0.0769230769230769,-0.0615384615384615,-0.0461538461538462,
-0.0307692307692308,-0.0153846153846154,0.),(-1.,1.),.UNSPECIFIED.)
GEOMETRIC_REPRESENTATION_ITEM()
RATIONAL_B_SPLINE_SURFACE(((1.,1.),(1.,1.),(1.,1.),(1.,1.),(1.,1.),(1.,
1.),(1.,1.),(1.,1.),(1.,1.),(1.,1.),(1.,1.),(1.,1.),(1.,1.),(1.,1.),(1.,
1.),(1.,1.),(1.,1.),(1.,1.),(1.,1.),(1.,1.),(1.,1.),(1.,1.),(1.,1.),(1.,
1.),(1.,1.),(1.,1.),(1.,1.),(1.,1.),(1.,1.),(1.,1.),(1.,1.),(1.,1.),(1.,
1.),(1.,1.),(1.,1.),(1.,1.),(1.,1.),(1.,1.),(1.,1.),(1.,1.),(1.,1.),(1.,
1.),(1.,1.),(1.,1.),(1.,1.),(1.,1.),(1.,1.),(1.,1.),(1.,1.),(1.,1.),(1.,
1.),(1.,1.),(1.,1.),(1.,1.),(1.,1.),(1.,1.),(1.,1.),(1.,1.),(1.,1.),(1.,
1.),(1.,1.),(1.,1.),(1.,1.),(1.,1.),(1.,1.),(1.,1.),(1.,1.),(1.,1.),(1.,
1.),(1.,1.)))
REPRESENTATION_ITEM('')
SURFACE()
);
#84=(
BOUNDED_SURFACE()
B_SPLINE_SURFACE(5,1,((#51918,#51919),(#51920,#51921),(#51922,#51923),(#51924,
#51925),(#51926,#51927),(#51928,#51929),(#51930,#51931),(#51932,#51933),
(#51934,#51935),(#51936,#51937),(#51938,#51939),(#51940,#51941),(#51942,
#51943),(#51944,#51945),(#51946,#51947),(#51948,#51949),(#51950,#51951),
(#51952,#51953),(#51954,#51955),(#51956,#51957),(#51958,#51959),(#51960,
#51961),(#51962,#51963),(#51964,#51965),(#51966,#51967),(#51968,#51969),
(#51970,#51971),(#51972,#51973),(#51974,#51975),(#51976,#51977),(#51978,
#51979),(#51980,#51981),(#51982,#51983),(#51984,#51985),(#51986,#51987),
(#51988,#51989),(#51990,#51991),(#51992,#51993),(#51994,#51995),(#51996,
#51997),(#51998,#51999),(#52000,#52001),(#52002,#52003),(#52004,#52005),
(#52006,#52007),(#52008,#52009),(#52010,#52011),(#52012,#52013),(#52014,
#52015),(#52016,#52017),(#52018,#52019),(#52020,#52021),(#52022,#52023),
(#52024,#52025),(#52026,#52027),(#52028,#52029),(#52030,#52031),(#52032,
#52033),(#52034,#52035),(#52036,#52037),(#52038,#52039),(#52040,#52041),
(#52042,#52043),(#52044,#52045),(#52046,#52047),(#52048,#52049),(#52050,
#52051),(#52052,#52053),(#52054,#52055),(#52056,#52057)),.UNSPECIFIED.,
 .F.,.F.,.F.)
B_SPLINE_SURFACE_WITH_KNOTS((6,1,1,1,1,1,1,1,1,1,1,1,1,1,1,1,1,1,1,1,1,
1,1,1,1,1,1,1,1,1,1,1,1,1,1,1,1,1,1,1,1,1,1,1,1,1,1,1,1,1,1,1,1,1,1,1,1,
1,1,1,1,1,1,1,1,6),(2,2),(-1.,-0.984615384615383,-0.969230769230768,-0.953846153846152,
-0.938461538461537,-0.923076923076922,-0.907692307692306,-0.892307692307691,
-0.876923076923076,-0.86153846153846,-0.846153846153845,-0.83076923076923,
-0.815384615384614,-0.799999999999999,-0.784615384615384,-0.769230769230768,
-0.753846153846153,-0.738461538461538,-0.723076923076922,-0.707692307692307,
-0.692307692307692,-0.676923076923076,-0.661538461538461,-0.646153846153846,
-0.63076923076923,-0.615384615384615,-0.6,-0.584615384615384,-0.569230769230769,
-0.553846153846154,-0.538461538461538,-0.523076923076923,-0.507692307692308,
-0.492307692307692,-0.476923076923077,-0.461538461538462,-0.446153846153846,
-0.430769230769231,-0.415384615384615,-0.4,-0.384615384615385,-0.369230769230769,
-0.353846153846154,-0.338461538461538,-0.323076923076923,-0.307692307692308,
-0.292307692307692,-0.276923076923077,-0.261538461538462,-0.246153846153846,
-0.230769230769231,-0.215384615384615,-0.2,-0.184615384615385,-0.169230769230769,
-0.153846153846154,-0.138461538461538,-0.123076923076923,-0.107692307692308,
-0.0923076923076923,-0.0769230769230769,-0.0615384615384615,-0.0461538461538462,
-0.0307692307692308,-0.0153846153846154,0.),(-1.,1.),.UNSPECIFIED.)
GEOMETRIC_REPRESENTATION_ITEM()
RATIONAL_B_SPLINE_SURFACE(((1.,1.),(1.,1.),(1.,1.),(1.,1.),(1.,1.),(1.,
1.),(1.,1.),(1.,1.),(1.,1.),(1.,1.),(1.,1.),(1.,1.),(1.,1.),(1.,1.),(1.,
1.),(1.,1.),(1.,1.),(1.,1.),(1.,1.),(1.,1.),(1.,1.),(1.,1.),(1.,1.),(1.,
1.),(1.,1.),(1.,1.),(1.,1.),(1.,1.),(1.,1.),(1.,1.),(1.,1.),(1.,1.),(1.,
1.),(1.,1.),(1.,1.),(1.,1.),(1.,1.),(1.,1.),(1.,1.),(1.,1.),(1.,1.),(1.,
1.),(1.,1.),(1.,1.),(1.,1.),(1.,1.),(1.,1.),(1.,1.),(1.,1.),(1.,1.),(1.,
1.),(1.,1.),(1.,1.),(1.,1.),(1.,1.),(1.,1.),(1.,1.),(1.,1.),(1.,1.),(1.,
1.),(1.,1.),(1.,1.),(1.,1.),(1.,1.),(1.,1.),(1.,1.),(1.,1.),(1.,1.),(1.,
1.),(1.,1.)))
REPRESENTATION_ITEM('')
SURFACE()
);
#85=(
BOUNDED_SURFACE()
B_SPLINE_SURFACE(5,1,((#52148,#52149),(#52150,#52151),(#52152,#52153),(#52154,
#52155),(#52156,#52157),(#52158,#52159),(#52160,#52161),(#52162,#52163),
(#52164,#52165),(#52166,#52167),(#52168,#52169),(#52170,#52171),(#52172,
#52173),(#52174,#52175),(#52176,#52177),(#52178,#52179),(#52180,#52181),
(#52182,#52183),(#52184,#52185),(#52186,#52187),(#52188,#52189),(#52190,
#52191),(#52192,#52193),(#52194,#52195),(#52196,#52197),(#52198,#52199),
(#52200,#52201),(#52202,#52203),(#52204,#52205),(#52206,#52207),(#52208,
#52209),(#52210,#52211),(#52212,#52213),(#52214,#52215),(#52216,#52217),
(#52218,#52219),(#52220,#52221),(#52222,#52223),(#52224,#52225),(#52226,
#52227),(#52228,#52229),(#52230,#52231),(#52232,#52233),(#52234,#52235),
(#52236,#52237),(#52238,#52239),(#52240,#52241),(#52242,#52243),(#52244,
#52245),(#52246,#52247),(#52248,#52249),(#52250,#52251),(#52252,#52253),
(#52254,#52255),(#52256,#52257),(#52258,#52259),(#52260,#52261),(#52262,
#52263),(#52264,#52265),(#52266,#52267),(#52268,#52269),(#52270,#52271),
(#52272,#52273),(#52274,#52275),(#52276,#52277),(#52278,#52279),(#52280,
#52281),(#52282,#52283),(#52284,#52285),(#52286,#52287)),.UNSPECIFIED.,
 .F.,.F.,.F.)
B_SPLINE_SURFACE_WITH_KNOTS((6,1,1,1,1,1,1,1,1,1,1,1,1,1,1,1,1,1,1,1,1,
1,1,1,1,1,1,1,1,1,1,1,1,1,1,1,1,1,1,1,1,1,1,1,1,1,1,1,1,1,1,1,1,1,1,1,1,
1,1,1,1,1,1,1,1,6),(2,2),(-1.,-0.984615384615383,-0.969230769230768,-0.953846153846152,
-0.938461538461537,-0.923076923076922,-0.907692307692306,-0.892307692307691,
-0.876923076923076,-0.86153846153846,-0.846153846153845,-0.83076923076923,
-0.815384615384614,-0.799999999999999,-0.784615384615384,-0.769230769230768,
-0.753846153846153,-0.738461538461538,-0.723076923076922,-0.707692307692307,
-0.692307692307692,-0.676923076923076,-0.661538461538461,-0.646153846153846,
-0.63076923076923,-0.615384615384615,-0.6,-0.584615384615384,-0.569230769230769,
-0.553846153846154,-0.538461538461538,-0.523076923076923,-0.507692307692308,
-0.492307692307692,-0.476923076923077,-0.461538461538462,-0.446153846153846,
-0.430769230769231,-0.415384615384615,-0.4,-0.384615384615385,-0.369230769230769,
-0.353846153846154,-0.338461538461538,-0.323076923076923,-0.307692307692308,
-0.292307692307692,-0.276923076923077,-0.261538461538462,-0.246153846153846,
-0.230769230769231,-0.215384615384615,-0.2,-0.184615384615385,-0.169230769230769,
-0.153846153846154,-0.138461538461538,-0.123076923076923,-0.107692307692308,
-0.0923076923076923,-0.0769230769230769,-0.0615384615384615,-0.0461538461538462,
-0.0307692307692308,-0.0153846153846154,0.),(-1.,1.),.UNSPECIFIED.)
GEOMETRIC_REPRESENTATION_ITEM()
RATIONAL_B_SPLINE_SURFACE(((1.,1.),(1.,1.),(1.,1.),(1.,1.),(1.,1.),(1.,
1.),(1.,1.),(1.,1.),(1.,1.),(1.,1.),(1.,1.),(1.,1.),(1.,1.),(1.,1.),(1.,
1.),(1.,1.),(1.,1.),(1.,1.),(1.,1.),(1.,1.),(1.,1.),(1.,1.),(1.,1.),(1.,
1.),(1.,1.),(1.,1.),(1.,1.),(1.,1.),(1.,1.),(1.,1.),(1.,1.),(1.,1.),(1.,
1.),(1.,1.),(1.,1.),(1.,1.),(1.,1.),(1.,1.),(1.,1.),(1.,1.),(1.,1.),(1.,
1.),(1.,1.),(1.,1.),(1.,1.),(1.,1.),(1.,1.),(1.,1.),(1.,1.),(1.,1.),(1.,
1.),(1.,1.),(1.,1.),(1.,1.),(1.,1.),(1.,1.),(1.,1.),(1.,1.),(1.,1.),(1.,
1.),(1.,1.),(1.,1.),(1.,1.),(1.,1.),(1.,1.),(1.,1.),(1.,1.),(1.,1.),(1.,
1.),(1.,1.)))
REPRESENTATION_ITEM('')
SURFACE()
);
#86=(
BOUNDED_SURFACE()
B_SPLINE_SURFACE(5,1,((#52360,#52361),(#52362,#52363),(#52364,#52365),(#52366,
#52367),(#52368,#52369),(#52370,#52371),(#52372,#52373),(#52374,#52375),
(#52376,#52377),(#52378,#52379),(#52380,#52381),(#52382,#52383),(#52384,
#52385),(#52386,#52387),(#52388,#52389),(#52390,#52391),(#52392,#52393),
(#52394,#52395),(#52396,#52397),(#52398,#52399),(#52400,#52401),(#52402,
#52403),(#52404,#52405),(#52406,#52407),(#52408,#52409),(#52410,#52411),
(#52412,#52413),(#52414,#52415),(#52416,#52417),(#52418,#52419),(#52420,
#52421),(#52422,#52423),(#52424,#52425),(#52426,#52427),(#52428,#52429),
(#52430,#52431),(#52432,#52433),(#52434,#52435),(#52436,#52437),(#52438,
#52439),(#52440,#52441),(#52442,#52443),(#52444,#52445),(#52446,#52447),
(#52448,#52449),(#52450,#52451),(#52452,#52453),(#52454,#52455),(#52456,
#52457),(#52458,#52459),(#52460,#52461),(#52462,#52463),(#52464,#52465),
(#52466,#52467),(#52468,#52469),(#52470,#52471),(#52472,#52473),(#52474,
#52475),(#52476,#52477),(#52478,#52479),(#52480,#52481),(#52482,#52483),
(#52484,#52485),(#52486,#52487),(#52488,#52489),(#52490,#52491),(#52492,
#52493),(#52494,#52495),(#52496,#52497),(#52498,#52499)),.UNSPECIFIED.,
 .F.,.F.,.F.)
B_SPLINE_SURFACE_WITH_KNOTS((6,1,1,1,1,1,1,1,1,1,1,1,1,1,1,1,1,1,1,1,1,
1,1,1,1,1,1,1,1,1,1,1,1,1,1,1,1,1,1,1,1,1,1,1,1,1,1,1,1,1,1,1,1,1,1,1,1,
1,1,1,1,1,1,1,1,6),(2,2),(-1.,-0.984615384615383,-0.969230769230768,-0.953846153846152,
-0.938461538461537,-0.923076923076922,-0.907692307692306,-0.892307692307691,
-0.876923076923076,-0.86153846153846,-0.846153846153845,-0.83076923076923,
-0.815384615384614,-0.799999999999999,-0.784615384615384,-0.769230769230768,
-0.753846153846153,-0.738461538461538,-0.723076923076922,-0.707692307692307,
-0.692307692307692,-0.676923076923076,-0.661538461538461,-0.646153846153846,
-0.63076923076923,-0.615384615384615,-0.6,-0.584615384615384,-0.569230769230769,
-0.553846153846154,-0.538461538461538,-0.523076923076923,-0.507692307692308,
-0.492307692307692,-0.476923076923077,-0.461538461538462,-0.446153846153846,
-0.430769230769231,-0.415384615384615,-0.4,-0.384615384615385,-0.369230769230769,
-0.353846153846154,-0.338461538461538,-0.323076923076923,-0.307692307692308,
-0.292307692307692,-0.276923076923077,-0.261538461538462,-0.246153846153846,
-0.230769230769231,-0.215384615384615,-0.2,-0.184615384615385,-0.169230769230769,
-0.153846153846154,-0.138461538461538,-0.123076923076923,-0.107692307692308,
-0.0923076923076923,-0.0769230769230769,-0.0615384615384615,-0.0461538461538462,
-0.0307692307692308,-0.0153846153846154,0.),(-1.,1.),.UNSPECIFIED.)
GEOMETRIC_REPRESENTATION_ITEM()
RATIONAL_B_SPLINE_SURFACE(((1.,1.),(1.,1.),(1.,1.),(1.,1.),(1.,1.),(1.,
1.),(1.,1.),(1.,1.),(1.,1.),(1.,1.),(1.,1.),(1.,1.),(1.,1.),(1.,1.),(1.,
1.),(1.,1.),(1.,1.),(1.,1.),(1.,1.),(1.,1.),(1.,1.),(1.,1.),(1.,1.),(1.,
1.),(1.,1.),(1.,1.),(1.,1.),(1.,1.),(1.,1.),(1.,1.),(1.,1.),(1.,1.),(1.,
1.),(1.,1.),(1.,1.),(1.,1.),(1.,1.),(1.,1.),(1.,1.),(1.,1.),(1.,1.),(1.,
1.),(1.,1.),(1.,1.),(1.,1.),(1.,1.),(1.,1.),(1.,1.),(1.,1.),(1.,1.),(1.,
1.),(1.,1.),(1.,1.),(1.,1.),(1.,1.),(1.,1.),(1.,1.),(1.,1.),(1.,1.),(1.,
1.),(1.,1.),(1.,1.),(1.,1.),(1.,1.),(1.,1.),(1.,1.),(1.,1.),(1.,1.),(1.,
1.),(1.,1.)))
REPRESENTATION_ITEM('')
SURFACE()
);
#87=(
BOUNDED_SURFACE()
B_SPLINE_SURFACE(5,1,((#52590,#52591),(#52592,#52593),(#52594,#52595),(#52596,
#52597),(#52598,#52599),(#52600,#52601),(#52602,#52603),(#52604,#52605),
(#52606,#52607),(#52608,#52609),(#52610,#52611),(#52612,#52613),(#52614,
#52615),(#52616,#52617),(#52618,#52619),(#52620,#52621),(#52622,#52623),
(#52624,#52625),(#52626,#52627),(#52628,#52629),(#52630,#52631),(#52632,
#52633),(#52634,#52635),(#52636,#52637),(#52638,#52639),(#52640,#52641),
(#52642,#52643),(#52644,#52645),(#52646,#52647),(#52648,#52649),(#52650,
#52651),(#52652,#52653),(#52654,#52655),(#52656,#52657),(#52658,#52659),
(#52660,#52661),(#52662,#52663),(#52664,#52665),(#52666,#52667),(#52668,
#52669),(#52670,#52671),(#52672,#52673),(#52674,#52675),(#52676,#52677),
(#52678,#52679),(#52680,#52681),(#52682,#52683),(#52684,#52685),(#52686,
#52687),(#52688,#52689),(#52690,#52691),(#52692,#52693),(#52694,#52695),
(#52696,#52697),(#52698,#52699),(#52700,#52701),(#52702,#52703),(#52704,
#52705),(#52706,#52707),(#52708,#52709),(#52710,#52711),(#52712,#52713),
(#52714,#52715),(#52716,#52717),(#52718,#52719),(#52720,#52721),(#52722,
#52723),(#52724,#52725),(#52726,#52727),(#52728,#52729)),.UNSPECIFIED.,
 .F.,.F.,.F.)
B_SPLINE_SURFACE_WITH_KNOTS((6,1,1,1,1,1,1,1,1,1,1,1,1,1,1,1,1,1,1,1,1,
1,1,1,1,1,1,1,1,1,1,1,1,1,1,1,1,1,1,1,1,1,1,1,1,1,1,1,1,1,1,1,1,1,1,1,1,
1,1,1,1,1,1,1,1,6),(2,2),(-1.,-0.984615384615383,-0.969230769230768,-0.953846153846152,
-0.938461538461537,-0.923076923076922,-0.907692307692306,-0.892307692307691,
-0.876923076923076,-0.86153846153846,-0.846153846153845,-0.83076923076923,
-0.815384615384614,-0.799999999999999,-0.784615384615384,-0.769230769230768,
-0.753846153846153,-0.738461538461538,-0.723076923076922,-0.707692307692307,
-0.692307692307692,-0.676923076923076,-0.661538461538461,-0.646153846153846,
-0.63076923076923,-0.615384615384615,-0.6,-0.584615384615384,-0.569230769230769,
-0.553846153846154,-0.538461538461538,-0.523076923076923,-0.507692307692308,
-0.492307692307692,-0.476923076923077,-0.461538461538462,-0.446153846153846,
-0.430769230769231,-0.415384615384615,-0.4,-0.384615384615385,-0.369230769230769,
-0.353846153846154,-0.338461538461538,-0.323076923076923,-0.307692307692308,
-0.292307692307692,-0.276923076923077,-0.261538461538462,-0.246153846153846,
-0.230769230769231,-0.215384615384615,-0.2,-0.184615384615385,-0.169230769230769,
-0.153846153846154,-0.138461538461538,-0.123076923076923,-0.107692307692308,
-0.0923076923076923,-0.0769230769230769,-0.0615384615384615,-0.0461538461538462,
-0.0307692307692308,-0.0153846153846154,0.),(-1.,1.),.UNSPECIFIED.)
GEOMETRIC_REPRESENTATION_ITEM()
RATIONAL_B_SPLINE_SURFACE(((1.,1.),(1.,1.),(1.,1.),(1.,1.),(1.,1.),(1.,
1.),(1.,1.),(1.,1.),(1.,1.),(1.,1.),(1.,1.),(1.,1.),(1.,1.),(1.,1.),(1.,
1.),(1.,1.),(1.,1.),(1.,1.),(1.,1.),(1.,1.),(1.,1.),(1.,1.),(1.,1.),(1.,
1.),(1.,1.),(1.,1.),(1.,1.),(1.,1.),(1.,1.),(1.,1.),(1.,1.),(1.,1.),(1.,
1.),(1.,1.),(1.,1.),(1.,1.),(1.,1.),(1.,1.),(1.,1.),(1.,1.),(1.,1.),(1.,
1.),(1.,1.),(1.,1.),(1.,1.),(1.,1.),(1.,1.),(1.,1.),(1.,1.),(1.,1.),(1.,
1.),(1.,1.),(1.,1.),(1.,1.),(1.,1.),(1.,1.),(1.,1.),(1.,1.),(1.,1.),(1.,
1.),(1.,1.),(1.,1.),(1.,1.),(1.,1.),(1.,1.),(1.,1.),(1.,1.),(1.,1.),(1.,
1.),(1.,1.)))
REPRESENTATION_ITEM('')
SURFACE()
);
#88=(
BOUNDED_SURFACE()
B_SPLINE_SURFACE(5,1,((#52802,#52803),(#52804,#52805),(#52806,#52807),(#52808,
#52809),(#52810,#52811),(#52812,#52813),(#52814,#52815),(#52816,#52817),
(#52818,#52819),(#52820,#52821),(#52822,#52823),(#52824,#52825),(#52826,
#52827),(#52828,#52829),(#52830,#52831),(#52832,#52833),(#52834,#52835),
(#52836,#52837),(#52838,#52839),(#52840,#52841),(#52842,#52843),(#52844,
#52845),(#52846,#52847),(#52848,#52849),(#52850,#52851),(#52852,#52853),
(#52854,#52855),(#52856,#52857),(#52858,#52859),(#52860,#52861),(#52862,
#52863),(#52864,#52865),(#52866,#52867),(#52868,#52869),(#52870,#52871),
(#52872,#52873),(#52874,#52875),(#52876,#52877),(#52878,#52879),(#52880,
#52881),(#52882,#52883),(#52884,#52885),(#52886,#52887),(#52888,#52889),
(#52890,#52891),(#52892,#52893),(#52894,#52895),(#52896,#52897),(#52898,
#52899),(#52900,#52901),(#52902,#52903),(#52904,#52905),(#52906,#52907),
(#52908,#52909),(#52910,#52911),(#52912,#52913),(#52914,#52915),(#52916,
#52917),(#52918,#52919),(#52920,#52921),(#52922,#52923),(#52924,#52925),
(#52926,#52927),(#52928,#52929),(#52930,#52931),(#52932,#52933),(#52934,
#52935),(#52936,#52937),(#52938,#52939),(#52940,#52941)),.UNSPECIFIED.,
 .F.,.F.,.F.)
B_SPLINE_SURFACE_WITH_KNOTS((6,1,1,1,1,1,1,1,1,1,1,1,1,1,1,1,1,1,1,1,1,
1,1,1,1,1,1,1,1,1,1,1,1,1,1,1,1,1,1,1,1,1,1,1,1,1,1,1,1,1,1,1,1,1,1,1,1,
1,1,1,1,1,1,1,1,6),(2,2),(-1.,-0.984615384615383,-0.969230769230768,-0.953846153846152,
-0.938461538461537,-0.923076923076922,-0.907692307692306,-0.892307692307691,
-0.876923076923076,-0.86153846153846,-0.846153846153845,-0.83076923076923,
-0.815384615384614,-0.799999999999999,-0.784615384615384,-0.769230769230768,
-0.753846153846153,-0.738461538461538,-0.723076923076922,-0.707692307692307,
-0.692307692307692,-0.676923076923076,-0.661538461538461,-0.646153846153846,
-0.63076923076923,-0.615384615384615,-0.6,-0.584615384615384,-0.569230769230769,
-0.553846153846154,-0.538461538461538,-0.523076923076923,-0.507692307692308,
-0.492307692307692,-0.476923076923077,-0.461538461538462,-0.446153846153846,
-0.430769230769231,-0.415384615384615,-0.4,-0.384615384615385,-0.369230769230769,
-0.353846153846154,-0.338461538461538,-0.323076923076923,-0.307692307692308,
-0.292307692307692,-0.276923076923077,-0.261538461538462,-0.246153846153846,
-0.230769230769231,-0.215384615384615,-0.2,-0.184615384615385,-0.169230769230769,
-0.153846153846154,-0.138461538461538,-0.123076923076923,-0.107692307692308,
-0.0923076923076923,-0.0769230769230769,-0.0615384615384615,-0.0461538461538462,
-0.0307692307692308,-0.0153846153846154,0.),(-1.,1.),.UNSPECIFIED.)
GEOMETRIC_REPRESENTATION_ITEM()
RATIONAL_B_SPLINE_SURFACE(((1.,1.),(1.,1.),(1.,1.),(1.,1.),(1.,1.),(1.,
1.),(1.,1.),(1.,1.),(1.,1.),(1.,1.),(1.,1.),(1.,1.),(1.,1.),(1.,1.),(1.,
1.),(1.,1.),(1.,1.),(1.,1.),(1.,1.),(1.,1.),(1.,1.),(1.,1.),(1.,1.),(1.,
1.),(1.,1.),(1.,1.),(1.,1.),(1.,1.),(1.,1.),(1.,1.),(1.,1.),(1.,1.),(1.,
1.),(1.,1.),(1.,1.),(1.,1.),(1.,1.),(1.,1.),(1.,1.),(1.,1.),(1.,1.),(1.,
1.),(1.,1.),(1.,1.),(1.,1.),(1.,1.),(1.,1.),(1.,1.),(1.,1.),(1.,1.),(1.,
1.),(1.,1.),(1.,1.),(1.,1.),(1.,1.),(1.,1.),(1.,1.),(1.,1.),(1.,1.),(1.,
1.),(1.,1.),(1.,1.),(1.,1.),(1.,1.),(1.,1.),(1.,1.),(1.,1.),(1.,1.),(1.,
1.),(1.,1.)))
REPRESENTATION_ITEM('')
SURFACE()
);
#89=(
BOUNDED_SURFACE()
B_SPLINE_SURFACE(5,1,((#53032,#53033),(#53034,#53035),(#53036,#53037),(#53038,
#53039),(#53040,#53041),(#53042,#53043),(#53044,#53045),(#53046,#53047),
(#53048,#53049),(#53050,#53051),(#53052,#53053),(#53054,#53055),(#53056,
#53057),(#53058,#53059),(#53060,#53061),(#53062,#53063),(#53064,#53065),
(#53066,#53067),(#53068,#53069),(#53070,#53071),(#53072,#53073),(#53074,
#53075),(#53076,#53077),(#53078,#53079),(#53080,#53081),(#53082,#53083),
(#53084,#53085),(#53086,#53087),(#53088,#53089),(#53090,#53091),(#53092,
#53093),(#53094,#53095),(#53096,#53097),(#53098,#53099),(#53100,#53101),
(#53102,#53103),(#53104,#53105),(#53106,#53107),(#53108,#53109),(#53110,
#53111),(#53112,#53113),(#53114,#53115),(#53116,#53117),(#53118,#53119),
(#53120,#53121),(#53122,#53123),(#53124,#53125),(#53126,#53127),(#53128,
#53129),(#53130,#53131),(#53132,#53133),(#53134,#53135),(#53136,#53137),
(#53138,#53139),(#53140,#53141),(#53142,#53143),(#53144,#53145),(#53146,
#53147),(#53148,#53149),(#53150,#53151),(#53152,#53153),(#53154,#53155),
(#53156,#53157),(#53158,#53159),(#53160,#53161),(#53162,#53163),(#53164,
#53165),(#53166,#53167),(#53168,#53169),(#53170,#53171)),.UNSPECIFIED.,
 .F.,.F.,.F.)
B_SPLINE_SURFACE_WITH_KNOTS((6,1,1,1,1,1,1,1,1,1,1,1,1,1,1,1,1,1,1,1,1,
1,1,1,1,1,1,1,1,1,1,1,1,1,1,1,1,1,1,1,1,1,1,1,1,1,1,1,1,1,1,1,1,1,1,1,1,
1,1,1,1,1,1,1,1,6),(2,2),(-1.,-0.984615384615383,-0.969230769230768,-0.953846153846152,
-0.938461538461537,-0.923076923076922,-0.907692307692306,-0.892307692307691,
-0.876923076923076,-0.86153846153846,-0.846153846153845,-0.83076923076923,
-0.815384615384614,-0.799999999999999,-0.784615384615384,-0.769230769230768,
-0.753846153846153,-0.738461538461538,-0.723076923076922,-0.707692307692307,
-0.692307692307692,-0.676923076923076,-0.661538461538461,-0.646153846153846,
-0.63076923076923,-0.615384615384615,-0.6,-0.584615384615384,-0.569230769230769,
-0.553846153846154,-0.538461538461538,-0.523076923076923,-0.507692307692308,
-0.492307692307692,-0.476923076923077,-0.461538461538462,-0.446153846153846,
-0.430769230769231,-0.415384615384615,-0.4,-0.384615384615385,-0.369230769230769,
-0.353846153846154,-0.338461538461538,-0.323076923076923,-0.307692307692308,
-0.292307692307692,-0.276923076923077,-0.261538461538462,-0.246153846153846,
-0.230769230769231,-0.215384615384615,-0.2,-0.184615384615385,-0.169230769230769,
-0.153846153846154,-0.138461538461538,-0.123076923076923,-0.107692307692308,
-0.0923076923076923,-0.0769230769230769,-0.0615384615384615,-0.0461538461538462,
-0.0307692307692308,-0.0153846153846154,0.),(-1.,1.),.UNSPECIFIED.)
GEOMETRIC_REPRESENTATION_ITEM()
RATIONAL_B_SPLINE_SURFACE(((1.,1.),(1.,1.),(1.,1.),(1.,1.),(1.,1.),(1.,
1.),(1.,1.),(1.,1.),(1.,1.),(1.,1.),(1.,1.),(1.,1.),(1.,1.),(1.,1.),(1.,
1.),(1.,1.),(1.,1.),(1.,1.),(1.,1.),(1.,1.),(1.,1.),(1.,1.),(1.,1.),(1.,
1.),(1.,1.),(1.,1.),(1.,1.),(1.,1.),(1.,1.),(1.,1.),(1.,1.),(1.,1.),(1.,
1.),(1.,1.),(1.,1.),(1.,1.),(1.,1.),(1.,1.),(1.,1.),(1.,1.),(1.,1.),(1.,
1.),(1.,1.),(1.,1.),(1.,1.),(1.,1.),(1.,1.),(1.,1.),(1.,1.),(1.,1.),(1.,
1.),(1.,1.),(1.,1.),(1.,1.),(1.,1.),(1.,1.),(1.,1.),(1.,1.),(1.,1.),(1.,
1.),(1.,1.),(1.,1.),(1.,1.),(1.,1.),(1.,1.),(1.,1.),(1.,1.),(1.,1.),(1.,
1.),(1.,1.)))
REPRESENTATION_ITEM('')
SURFACE()
);
#90=(
BOUNDED_SURFACE()
B_SPLINE_SURFACE(5,1,((#53244,#53245),(#53246,#53247),(#53248,#53249),(#53250,
#53251),(#53252,#53253),(#53254,#53255),(#53256,#53257),(#53258,#53259),
(#53260,#53261),(#53262,#53263),(#53264,#53265),(#53266,#53267),(#53268,
#53269),(#53270,#53271),(#53272,#53273),(#53274,#53275),(#53276,#53277),
(#53278,#53279),(#53280,#53281),(#53282,#53283),(#53284,#53285),(#53286,
#53287),(#53288,#53289),(#53290,#53291),(#53292,#53293),(#53294,#53295),
(#53296,#53297),(#53298,#53299),(#53300,#53301),(#53302,#53303),(#53304,
#53305),(#53306,#53307),(#53308,#53309),(#53310,#53311),(#53312,#53313),
(#53314,#53315),(#53316,#53317),(#53318,#53319),(#53320,#53321),(#53322,
#53323),(#53324,#53325),(#53326,#53327),(#53328,#53329),(#53330,#53331),
(#53332,#53333),(#53334,#53335),(#53336,#53337),(#53338,#53339),(#53340,
#53341),(#53342,#53343),(#53344,#53345),(#53346,#53347),(#53348,#53349),
(#53350,#53351),(#53352,#53353),(#53354,#53355),(#53356,#53357),(#53358,
#53359),(#53360,#53361),(#53362,#53363),(#53364,#53365),(#53366,#53367),
(#53368,#53369),(#53370,#53371),(#53372,#53373),(#53374,#53375),(#53376,
#53377),(#53378,#53379),(#53380,#53381),(#53382,#53383)),.UNSPECIFIED.,
 .F.,.F.,.F.)
B_SPLINE_SURFACE_WITH_KNOTS((6,1,1,1,1,1,1,1,1,1,1,1,1,1,1,1,1,1,1,1,1,
1,1,1,1,1,1,1,1,1,1,1,1,1,1,1,1,1,1,1,1,1,1,1,1,1,1,1,1,1,1,1,1,1,1,1,1,
1,1,1,1,1,1,1,1,6),(2,2),(-1.,-0.984615384615383,-0.969230769230768,-0.953846153846152,
-0.938461538461537,-0.923076923076922,-0.907692307692306,-0.892307692307691,
-0.876923076923076,-0.86153846153846,-0.846153846153845,-0.83076923076923,
-0.815384615384614,-0.799999999999999,-0.784615384615384,-0.769230769230768,
-0.753846153846153,-0.738461538461538,-0.723076923076922,-0.707692307692307,
-0.692307692307692,-0.676923076923076,-0.661538461538461,-0.646153846153846,
-0.63076923076923,-0.615384615384615,-0.6,-0.584615384615384,-0.569230769230769,
-0.553846153846154,-0.538461538461538,-0.523076923076923,-0.507692307692308,
-0.492307692307692,-0.476923076923077,-0.461538461538462,-0.446153846153846,
-0.430769230769231,-0.415384615384615,-0.4,-0.384615384615385,-0.369230769230769,
-0.353846153846154,-0.338461538461538,-0.323076923076923,-0.307692307692308,
-0.292307692307692,-0.276923076923077,-0.261538461538462,-0.246153846153846,
-0.230769230769231,-0.215384615384615,-0.2,-0.184615384615385,-0.169230769230769,
-0.153846153846154,-0.138461538461538,-0.123076923076923,-0.107692307692308,
-0.0923076923076923,-0.0769230769230769,-0.0615384615384615,-0.0461538461538462,
-0.0307692307692308,-0.0153846153846154,0.),(-1.,1.),.UNSPECIFIED.)
GEOMETRIC_REPRESENTATION_ITEM()
RATIONAL_B_SPLINE_SURFACE(((1.,1.),(1.,1.),(1.,1.),(1.,1.),(1.,1.),(1.,
1.),(1.,1.),(1.,1.),(1.,1.),(1.,1.),(1.,1.),(1.,1.),(1.,1.),(1.,1.),(1.,
1.),(1.,1.),(1.,1.),(1.,1.),(1.,1.),(1.,1.),(1.,1.),(1.,1.),(1.,1.),(1.,
1.),(1.,1.),(1.,1.),(1.,1.),(1.,1.),(1.,1.),(1.,1.),(1.,1.),(1.,1.),(1.,
1.),(1.,1.),(1.,1.),(1.,1.),(1.,1.),(1.,1.),(1.,1.),(1.,1.),(1.,1.),(1.,
1.),(1.,1.),(1.,1.),(1.,1.),(1.,1.),(1.,1.),(1.,1.),(1.,1.),(1.,1.),(1.,
1.),(1.,1.),(1.,1.),(1.,1.),(1.,1.),(1.,1.),(1.,1.),(1.,1.),(1.,1.),(1.,
1.),(1.,1.),(1.,1.),(1.,1.),(1.,1.),(1.,1.),(1.,1.),(1.,1.),(1.,1.),(1.,
1.),(1.,1.)))
REPRESENTATION_ITEM('')
SURFACE()
);
#91=(
BOUNDED_SURFACE()
B_SPLINE_SURFACE(5,1,((#53474,#53475),(#53476,#53477),(#53478,#53479),(#53480,
#53481),(#53482,#53483),(#53484,#53485),(#53486,#53487),(#53488,#53489),
(#53490,#53491),(#53492,#53493),(#53494,#53495),(#53496,#53497),(#53498,
#53499),(#53500,#53501),(#53502,#53503),(#53504,#53505),(#53506,#53507),
(#53508,#53509),(#53510,#53511),(#53512,#53513),(#53514,#53515),(#53516,
#53517),(#53518,#53519),(#53520,#53521),(#53522,#53523),(#53524,#53525),
(#53526,#53527),(#53528,#53529),(#53530,#53531),(#53532,#53533),(#53534,
#53535),(#53536,#53537),(#53538,#53539),(#53540,#53541),(#53542,#53543),
(#53544,#53545),(#53546,#53547),(#53548,#53549),(#53550,#53551),(#53552,
#53553),(#53554,#53555),(#53556,#53557),(#53558,#53559),(#53560,#53561),
(#53562,#53563),(#53564,#53565),(#53566,#53567),(#53568,#53569),(#53570,
#53571),(#53572,#53573),(#53574,#53575),(#53576,#53577),(#53578,#53579),
(#53580,#53581),(#53582,#53583),(#53584,#53585),(#53586,#53587),(#53588,
#53589),(#53590,#53591),(#53592,#53593),(#53594,#53595),(#53596,#53597),
(#53598,#53599),(#53600,#53601),(#53602,#53603),(#53604,#53605),(#53606,
#53607),(#53608,#53609),(#53610,#53611),(#53612,#53613)),.UNSPECIFIED.,
 .F.,.F.,.F.)
B_SPLINE_SURFACE_WITH_KNOTS((6,1,1,1,1,1,1,1,1,1,1,1,1,1,1,1,1,1,1,1,1,
1,1,1,1,1,1,1,1,1,1,1,1,1,1,1,1,1,1,1,1,1,1,1,1,1,1,1,1,1,1,1,1,1,1,1,1,
1,1,1,1,1,1,1,1,6),(2,2),(-1.,-0.984615384615383,-0.969230769230768,-0.953846153846152,
-0.938461538461537,-0.923076923076922,-0.907692307692306,-0.892307692307691,
-0.876923076923076,-0.86153846153846,-0.846153846153845,-0.83076923076923,
-0.815384615384614,-0.799999999999999,-0.784615384615384,-0.769230769230768,
-0.753846153846153,-0.738461538461538,-0.723076923076922,-0.707692307692307,
-0.692307692307692,-0.676923076923076,-0.661538461538461,-0.646153846153846,
-0.63076923076923,-0.615384615384615,-0.6,-0.584615384615384,-0.569230769230769,
-0.553846153846154,-0.538461538461538,-0.523076923076923,-0.507692307692308,
-0.492307692307692,-0.476923076923077,-0.461538461538462,-0.446153846153846,
-0.430769230769231,-0.415384615384615,-0.4,-0.384615384615385,-0.369230769230769,
-0.353846153846154,-0.338461538461538,-0.323076923076923,-0.307692307692308,
-0.292307692307692,-0.276923076923077,-0.261538461538462,-0.246153846153846,
-0.230769230769231,-0.215384615384615,-0.2,-0.184615384615385,-0.169230769230769,
-0.153846153846154,-0.138461538461538,-0.123076923076923,-0.107692307692308,
-0.0923076923076923,-0.0769230769230769,-0.0615384615384615,-0.0461538461538462,
-0.0307692307692308,-0.0153846153846154,0.),(-1.,1.),.UNSPECIFIED.)
GEOMETRIC_REPRESENTATION_ITEM()
RATIONAL_B_SPLINE_SURFACE(((1.,1.),(1.,1.),(1.,1.),(1.,1.),(1.,1.),(1.,
1.),(1.,1.),(1.,1.),(1.,1.),(1.,1.),(1.,1.),(1.,1.),(1.,1.),(1.,1.),(1.,
1.),(1.,1.),(1.,1.),(1.,1.),(1.,1.),(1.,1.),(1.,1.),(1.,1.),(1.,1.),(1.,
1.),(1.,1.),(1.,1.),(1.,1.),(1.,1.),(1.,1.),(1.,1.),(1.,1.),(1.,1.),(1.,
1.),(1.,1.),(1.,1.),(1.,1.),(1.,1.),(1.,1.),(1.,1.),(1.,1.),(1.,1.),(1.,
1.),(1.,1.),(1.,1.),(1.,1.),(1.,1.),(1.,1.),(1.,1.),(1.,1.),(1.,1.),(1.,
1.),(1.,1.),(1.,1.),(1.,1.),(1.,1.),(1.,1.),(1.,1.),(1.,1.),(1.,1.),(1.,
1.),(1.,1.),(1.,1.),(1.,1.),(1.,1.),(1.,1.),(1.,1.),(1.,1.),(1.,1.),(1.,
1.),(1.,1.)))
REPRESENTATION_ITEM('')
SURFACE()
);
#92=(
BOUNDED_SURFACE()
B_SPLINE_SURFACE(5,1,((#53686,#53687),(#53688,#53689),(#53690,#53691),(#53692,
#53693),(#53694,#53695),(#53696,#53697),(#53698,#53699),(#53700,#53701),
(#53702,#53703),(#53704,#53705),(#53706,#53707),(#53708,#53709),(#53710,
#53711),(#53712,#53713),(#53714,#53715),(#53716,#53717),(#53718,#53719),
(#53720,#53721),(#53722,#53723),(#53724,#53725),(#53726,#53727),(#53728,
#53729),(#53730,#53731),(#53732,#53733),(#53734,#53735),(#53736,#53737),
(#53738,#53739),(#53740,#53741),(#53742,#53743),(#53744,#53745),(#53746,
#53747),(#53748,#53749),(#53750,#53751),(#53752,#53753),(#53754,#53755),
(#53756,#53757),(#53758,#53759),(#53760,#53761),(#53762,#53763),(#53764,
#53765),(#53766,#53767),(#53768,#53769),(#53770,#53771),(#53772,#53773),
(#53774,#53775),(#53776,#53777),(#53778,#53779),(#53780,#53781),(#53782,
#53783),(#53784,#53785),(#53786,#53787),(#53788,#53789),(#53790,#53791),
(#53792,#53793),(#53794,#53795),(#53796,#53797),(#53798,#53799),(#53800,
#53801),(#53802,#53803),(#53804,#53805),(#53806,#53807),(#53808,#53809),
(#53810,#53811),(#53812,#53813),(#53814,#53815),(#53816,#53817),(#53818,
#53819),(#53820,#53821),(#53822,#53823),(#53824,#53825)),.UNSPECIFIED.,
 .F.,.F.,.F.)
B_SPLINE_SURFACE_WITH_KNOTS((6,1,1,1,1,1,1,1,1,1,1,1,1,1,1,1,1,1,1,1,1,
1,1,1,1,1,1,1,1,1,1,1,1,1,1,1,1,1,1,1,1,1,1,1,1,1,1,1,1,1,1,1,1,1,1,1,1,
1,1,1,1,1,1,1,1,6),(2,2),(-1.,-0.984615384615383,-0.969230769230768,-0.953846153846152,
-0.938461538461537,-0.923076923076922,-0.907692307692306,-0.892307692307691,
-0.876923076923076,-0.86153846153846,-0.846153846153845,-0.83076923076923,
-0.815384615384614,-0.799999999999999,-0.784615384615384,-0.769230769230768,
-0.753846153846153,-0.738461538461538,-0.723076923076922,-0.707692307692307,
-0.692307692307692,-0.676923076923076,-0.661538461538461,-0.646153846153846,
-0.63076923076923,-0.615384615384615,-0.6,-0.584615384615384,-0.569230769230769,
-0.553846153846154,-0.538461538461538,-0.523076923076923,-0.507692307692308,
-0.492307692307692,-0.476923076923077,-0.461538461538462,-0.446153846153846,
-0.430769230769231,-0.415384615384615,-0.4,-0.384615384615385,-0.369230769230769,
-0.353846153846154,-0.338461538461538,-0.323076923076923,-0.307692307692308,
-0.292307692307692,-0.276923076923077,-0.261538461538462,-0.246153846153846,
-0.230769230769231,-0.215384615384615,-0.2,-0.184615384615385,-0.169230769230769,
-0.153846153846154,-0.138461538461538,-0.123076923076923,-0.107692307692308,
-0.0923076923076923,-0.0769230769230769,-0.0615384615384615,-0.0461538461538462,
-0.0307692307692308,-0.0153846153846154,0.),(-1.,1.),.UNSPECIFIED.)
GEOMETRIC_REPRESENTATION_ITEM()
RATIONAL_B_SPLINE_SURFACE(((1.,1.),(1.,1.),(1.,1.),(1.,1.),(1.,1.),(1.,
1.),(1.,1.),(1.,1.),(1.,1.),(1.,1.),(1.,1.),(1.,1.),(1.,1.),(1.,1.),(1.,
1.),(1.,1.),(1.,1.),(1.,1.),(1.,1.),(1.,1.),(1.,1.),(1.,1.),(1.,1.),(1.,
1.),(1.,1.),(1.,1.),(1.,1.),(1.,1.),(1.,1.),(1.,1.),(1.,1.),(1.,1.),(1.,
1.),(1.,1.),(1.,1.),(1.,1.),(1.,1.),(1.,1.),(1.,1.),(1.,1.),(1.,1.),(1.,
1.),(1.,1.),(1.,1.),(1.,1.),(1.,1.),(1.,1.),(1.,1.),(1.,1.),(1.,1.),(1.,
1.),(1.,1.),(1.,1.),(1.,1.),(1.,1.),(1.,1.),(1.,1.),(1.,1.),(1.,1.),(1.,
1.),(1.,1.),(1.,1.),(1.,1.),(1.,1.),(1.,1.),(1.,1.),(1.,1.),(1.,1.),(1.,
1.),(1.,1.)))
REPRESENTATION_ITEM('')
SURFACE()
);
#93=(
BOUNDED_SURFACE()
B_SPLINE_SURFACE(5,1,((#53916,#53917),(#53918,#53919),(#53920,#53921),(#53922,
#53923),(#53924,#53925),(#53926,#53927),(#53928,#53929),(#53930,#53931),
(#53932,#53933),(#53934,#53935),(#53936,#53937),(#53938,#53939),(#53940,
#53941),(#53942,#53943),(#53944,#53945),(#53946,#53947),(#53948,#53949),
(#53950,#53951),(#53952,#53953),(#53954,#53955),(#53956,#53957),(#53958,
#53959),(#53960,#53961),(#53962,#53963),(#53964,#53965),(#53966,#53967),
(#53968,#53969),(#53970,#53971),(#53972,#53973),(#53974,#53975),(#53976,
#53977),(#53978,#53979),(#53980,#53981),(#53982,#53983),(#53984,#53985),
(#53986,#53987),(#53988,#53989),(#53990,#53991),(#53992,#53993),(#53994,
#53995),(#53996,#53997),(#53998,#53999),(#54000,#54001),(#54002,#54003),
(#54004,#54005),(#54006,#54007),(#54008,#54009),(#54010,#54011),(#54012,
#54013),(#54014,#54015),(#54016,#54017),(#54018,#54019),(#54020,#54021),
(#54022,#54023),(#54024,#54025),(#54026,#54027),(#54028,#54029),(#54030,
#54031),(#54032,#54033),(#54034,#54035),(#54036,#54037),(#54038,#54039),
(#54040,#54041),(#54042,#54043),(#54044,#54045),(#54046,#54047),(#54048,
#54049),(#54050,#54051),(#54052,#54053),(#54054,#54055)),.UNSPECIFIED.,
 .F.,.F.,.F.)
B_SPLINE_SURFACE_WITH_KNOTS((6,1,1,1,1,1,1,1,1,1,1,1,1,1,1,1,1,1,1,1,1,
1,1,1,1,1,1,1,1,1,1,1,1,1,1,1,1,1,1,1,1,1,1,1,1,1,1,1,1,1,1,1,1,1,1,1,1,
1,1,1,1,1,1,1,1,6),(2,2),(-1.,-0.984615384615383,-0.969230769230768,-0.953846153846152,
-0.938461538461537,-0.923076923076922,-0.907692307692306,-0.892307692307691,
-0.876923076923076,-0.86153846153846,-0.846153846153845,-0.83076923076923,
-0.815384615384614,-0.799999999999999,-0.784615384615384,-0.769230769230768,
-0.753846153846153,-0.738461538461538,-0.723076923076922,-0.707692307692307,
-0.692307692307692,-0.676923076923076,-0.661538461538461,-0.646153846153846,
-0.63076923076923,-0.615384615384615,-0.6,-0.584615384615384,-0.569230769230769,
-0.553846153846154,-0.538461538461538,-0.523076923076923,-0.507692307692308,
-0.492307692307692,-0.476923076923077,-0.461538461538462,-0.446153846153846,
-0.430769230769231,-0.415384615384615,-0.4,-0.384615384615385,-0.369230769230769,
-0.353846153846154,-0.338461538461538,-0.323076923076923,-0.307692307692308,
-0.292307692307692,-0.276923076923077,-0.261538461538462,-0.246153846153846,
-0.230769230769231,-0.215384615384615,-0.2,-0.184615384615385,-0.169230769230769,
-0.153846153846154,-0.138461538461538,-0.123076923076923,-0.107692307692308,
-0.0923076923076923,-0.0769230769230769,-0.0615384615384615,-0.0461538461538462,
-0.0307692307692308,-0.0153846153846154,0.),(-1.,1.),.UNSPECIFIED.)
GEOMETRIC_REPRESENTATION_ITEM()
RATIONAL_B_SPLINE_SURFACE(((1.,1.),(1.,1.),(1.,1.),(1.,1.),(1.,1.),(1.,
1.),(1.,1.),(1.,1.),(1.,1.),(1.,1.),(1.,1.),(1.,1.),(1.,1.),(1.,1.),(1.,
1.),(1.,1.),(1.,1.),(1.,1.),(1.,1.),(1.,1.),(1.,1.),(1.,1.),(1.,1.),(1.,
1.),(1.,1.),(1.,1.),(1.,1.),(1.,1.),(1.,1.),(1.,1.),(1.,1.),(1.,1.),(1.,
1.),(1.,1.),(1.,1.),(1.,1.),(1.,1.),(1.,1.),(1.,1.),(1.,1.),(1.,1.),(1.,
1.),(1.,1.),(1.,1.),(1.,1.),(1.,1.),(1.,1.),(1.,1.),(1.,1.),(1.,1.),(1.,
1.),(1.,1.),(1.,1.),(1.,1.),(1.,1.),(1.,1.),(1.,1.),(1.,1.),(1.,1.),(1.,
1.),(1.,1.),(1.,1.),(1.,1.),(1.,1.),(1.,1.),(1.,1.),(1.,1.),(1.,1.),(1.,
1.),(1.,1.)))
REPRESENTATION_ITEM('')
SURFACE()
);
#94=(
BOUNDED_SURFACE()
B_SPLINE_SURFACE(5,1,((#54128,#54129),(#54130,#54131),(#54132,#54133),(#54134,
#54135),(#54136,#54137),(#54138,#54139),(#54140,#54141),(#54142,#54143),
(#54144,#54145),(#54146,#54147),(#54148,#54149),(#54150,#54151),(#54152,
#54153),(#54154,#54155),(#54156,#54157),(#54158,#54159),(#54160,#54161),
(#54162,#54163),(#54164,#54165),(#54166,#54167),(#54168,#54169),(#54170,
#54171),(#54172,#54173),(#54174,#54175),(#54176,#54177),(#54178,#54179),
(#54180,#54181),(#54182,#54183),(#54184,#54185),(#54186,#54187),(#54188,
#54189),(#54190,#54191),(#54192,#54193),(#54194,#54195),(#54196,#54197),
(#54198,#54199),(#54200,#54201),(#54202,#54203),(#54204,#54205),(#54206,
#54207),(#54208,#54209),(#54210,#54211),(#54212,#54213),(#54214,#54215),
(#54216,#54217),(#54218,#54219),(#54220,#54221),(#54222,#54223),(#54224,
#54225),(#54226,#54227),(#54228,#54229),(#54230,#54231),(#54232,#54233),
(#54234,#54235),(#54236,#54237),(#54238,#54239),(#54240,#54241),(#54242,
#54243),(#54244,#54245),(#54246,#54247),(#54248,#54249),(#54250,#54251),
(#54252,#54253),(#54254,#54255),(#54256,#54257),(#54258,#54259),(#54260,
#54261),(#54262,#54263),(#54264,#54265),(#54266,#54267)),.UNSPECIFIED.,
 .F.,.F.,.F.)
B_SPLINE_SURFACE_WITH_KNOTS((6,1,1,1,1,1,1,1,1,1,1,1,1,1,1,1,1,1,1,1,1,
1,1,1,1,1,1,1,1,1,1,1,1,1,1,1,1,1,1,1,1,1,1,1,1,1,1,1,1,1,1,1,1,1,1,1,1,
1,1,1,1,1,1,1,1,6),(2,2),(-1.,-0.984615384615383,-0.969230769230768,-0.953846153846152,
-0.938461538461537,-0.923076923076922,-0.907692307692306,-0.892307692307691,
-0.876923076923076,-0.86153846153846,-0.846153846153845,-0.83076923076923,
-0.815384615384614,-0.799999999999999,-0.784615384615384,-0.769230769230768,
-0.753846153846153,-0.738461538461538,-0.723076923076922,-0.707692307692307,
-0.692307692307692,-0.676923076923076,-0.661538461538461,-0.646153846153846,
-0.63076923076923,-0.615384615384615,-0.6,-0.584615384615384,-0.569230769230769,
-0.553846153846154,-0.538461538461538,-0.523076923076923,-0.507692307692308,
-0.492307692307692,-0.476923076923077,-0.461538461538462,-0.446153846153846,
-0.430769230769231,-0.415384615384615,-0.4,-0.384615384615385,-0.369230769230769,
-0.353846153846154,-0.338461538461538,-0.323076923076923,-0.307692307692308,
-0.292307692307692,-0.276923076923077,-0.261538461538462,-0.246153846153846,
-0.230769230769231,-0.215384615384615,-0.2,-0.184615384615385,-0.169230769230769,
-0.153846153846154,-0.138461538461538,-0.123076923076923,-0.107692307692308,
-0.0923076923076923,-0.0769230769230769,-0.0615384615384615,-0.0461538461538462,
-0.0307692307692308,-0.0153846153846154,0.),(-1.,1.),.UNSPECIFIED.)
GEOMETRIC_REPRESENTATION_ITEM()
RATIONAL_B_SPLINE_SURFACE(((1.,1.),(1.,1.),(1.,1.),(1.,1.),(1.,1.),(1.,
1.),(1.,1.),(1.,1.),(1.,1.),(1.,1.),(1.,1.),(1.,1.),(1.,1.),(1.,1.),(1.,
1.),(1.,1.),(1.,1.),(1.,1.),(1.,1.),(1.,1.),(1.,1.),(1.,1.),(1.,1.),(1.,
1.),(1.,1.),(1.,1.),(1.,1.),(1.,1.),(1.,1.),(1.,1.),(1.,1.),(1.,1.),(1.,
1.),(1.,1.),(1.,1.),(1.,1.),(1.,1.),(1.,1.),(1.,1.),(1.,1.),(1.,1.),(1.,
1.),(1.,1.),(1.,1.),(1.,1.),(1.,1.),(1.,1.),(1.,1.),(1.,1.),(1.,1.),(1.,
1.),(1.,1.),(1.,1.),(1.,1.),(1.,1.),(1.,1.),(1.,1.),(1.,1.),(1.,1.),(1.,
1.),(1.,1.),(1.,1.),(1.,1.),(1.,1.),(1.,1.),(1.,1.),(1.,1.),(1.,1.),(1.,
1.),(1.,1.)))
REPRESENTATION_ITEM('')
SURFACE()
);
#95=(
BOUNDED_SURFACE()
B_SPLINE_SURFACE(5,1,((#54358,#54359),(#54360,#54361),(#54362,#54363),(#54364,
#54365),(#54366,#54367),(#54368,#54369),(#54370,#54371),(#54372,#54373),
(#54374,#54375),(#54376,#54377),(#54378,#54379),(#54380,#54381),(#54382,
#54383),(#54384,#54385),(#54386,#54387),(#54388,#54389),(#54390,#54391),
(#54392,#54393),(#54394,#54395),(#54396,#54397),(#54398,#54399),(#54400,
#54401),(#54402,#54403),(#54404,#54405),(#54406,#54407),(#54408,#54409),
(#54410,#54411),(#54412,#54413),(#54414,#54415),(#54416,#54417),(#54418,
#54419),(#54420,#54421),(#54422,#54423),(#54424,#54425),(#54426,#54427),
(#54428,#54429),(#54430,#54431),(#54432,#54433),(#54434,#54435),(#54436,
#54437),(#54438,#54439),(#54440,#54441),(#54442,#54443),(#54444,#54445),
(#54446,#54447),(#54448,#54449),(#54450,#54451),(#54452,#54453),(#54454,
#54455),(#54456,#54457),(#54458,#54459),(#54460,#54461),(#54462,#54463),
(#54464,#54465),(#54466,#54467),(#54468,#54469),(#54470,#54471),(#54472,
#54473),(#54474,#54475),(#54476,#54477),(#54478,#54479),(#54480,#54481),
(#54482,#54483),(#54484,#54485),(#54486,#54487),(#54488,#54489),(#54490,
#54491),(#54492,#54493),(#54494,#54495),(#54496,#54497)),.UNSPECIFIED.,
 .F.,.F.,.F.)
B_SPLINE_SURFACE_WITH_KNOTS((6,1,1,1,1,1,1,1,1,1,1,1,1,1,1,1,1,1,1,1,1,
1,1,1,1,1,1,1,1,1,1,1,1,1,1,1,1,1,1,1,1,1,1,1,1,1,1,1,1,1,1,1,1,1,1,1,1,
1,1,1,1,1,1,1,1,6),(2,2),(-1.,-0.984615384615383,-0.969230769230768,-0.953846153846152,
-0.938461538461537,-0.923076923076922,-0.907692307692306,-0.892307692307691,
-0.876923076923076,-0.86153846153846,-0.846153846153845,-0.83076923076923,
-0.815384615384614,-0.799999999999999,-0.784615384615384,-0.769230769230768,
-0.753846153846153,-0.738461538461538,-0.723076923076922,-0.707692307692307,
-0.692307692307692,-0.676923076923076,-0.661538461538461,-0.646153846153846,
-0.63076923076923,-0.615384615384615,-0.6,-0.584615384615384,-0.569230769230769,
-0.553846153846154,-0.538461538461538,-0.523076923076923,-0.507692307692308,
-0.492307692307692,-0.476923076923077,-0.461538461538462,-0.446153846153846,
-0.430769230769231,-0.415384615384615,-0.4,-0.384615384615385,-0.369230769230769,
-0.353846153846154,-0.338461538461538,-0.323076923076923,-0.307692307692308,
-0.292307692307692,-0.276923076923077,-0.261538461538462,-0.246153846153846,
-0.230769230769231,-0.215384615384615,-0.2,-0.184615384615385,-0.169230769230769,
-0.153846153846154,-0.138461538461538,-0.123076923076923,-0.107692307692308,
-0.0923076923076923,-0.0769230769230769,-0.0615384615384615,-0.0461538461538462,
-0.0307692307692308,-0.0153846153846154,0.),(-1.,1.),.UNSPECIFIED.)
GEOMETRIC_REPRESENTATION_ITEM()
RATIONAL_B_SPLINE_SURFACE(((1.,1.),(1.,1.),(1.,1.),(1.,1.),(1.,1.),(1.,
1.),(1.,1.),(1.,1.),(1.,1.),(1.,1.),(1.,1.),(1.,1.),(1.,1.),(1.,1.),(1.,
1.),(1.,1.),(1.,1.),(1.,1.),(1.,1.),(1.,1.),(1.,1.),(1.,1.),(1.,1.),(1.,
1.),(1.,1.),(1.,1.),(1.,1.),(1.,1.),(1.,1.),(1.,1.),(1.,1.),(1.,1.),(1.,
1.),(1.,1.),(1.,1.),(1.,1.),(1.,1.),(1.,1.),(1.,1.),(1.,1.),(1.,1.),(1.,
1.),(1.,1.),(1.,1.),(1.,1.),(1.,1.),(1.,1.),(1.,1.),(1.,1.),(1.,1.),(1.,
1.),(1.,1.),(1.,1.),(1.,1.),(1.,1.),(1.,1.),(1.,1.),(1.,1.),(1.,1.),(1.,
1.),(1.,1.),(1.,1.),(1.,1.),(1.,1.),(1.,1.),(1.,1.),(1.,1.),(1.,1.),(1.,
1.),(1.,1.)))
REPRESENTATION_ITEM('')
SURFACE()
);
#96=(
BOUNDED_SURFACE()
B_SPLINE_SURFACE(5,1,((#54570,#54571),(#54572,#54573),(#54574,#54575),(#54576,
#54577),(#54578,#54579),(#54580,#54581),(#54582,#54583),(#54584,#54585),
(#54586,#54587),(#54588,#54589),(#54590,#54591),(#54592,#54593),(#54594,
#54595),(#54596,#54597),(#54598,#54599),(#54600,#54601),(#54602,#54603),
(#54604,#54605),(#54606,#54607),(#54608,#54609),(#54610,#54611),(#54612,
#54613),(#54614,#54615),(#54616,#54617),(#54618,#54619),(#54620,#54621),
(#54622,#54623),(#54624,#54625),(#54626,#54627),(#54628,#54629),(#54630,
#54631),(#54632,#54633),(#54634,#54635),(#54636,#54637),(#54638,#54639),
(#54640,#54641),(#54642,#54643),(#54644,#54645),(#54646,#54647),(#54648,
#54649),(#54650,#54651),(#54652,#54653),(#54654,#54655),(#54656,#54657),
(#54658,#54659),(#54660,#54661),(#54662,#54663),(#54664,#54665),(#54666,
#54667),(#54668,#54669),(#54670,#54671),(#54672,#54673),(#54674,#54675),
(#54676,#54677),(#54678,#54679),(#54680,#54681),(#54682,#54683),(#54684,
#54685),(#54686,#54687),(#54688,#54689),(#54690,#54691),(#54692,#54693),
(#54694,#54695),(#54696,#54697),(#54698,#54699),(#54700,#54701),(#54702,
#54703),(#54704,#54705),(#54706,#54707),(#54708,#54709)),.UNSPECIFIED.,
 .F.,.F.,.F.)
B_SPLINE_SURFACE_WITH_KNOTS((6,1,1,1,1,1,1,1,1,1,1,1,1,1,1,1,1,1,1,1,1,
1,1,1,1,1,1,1,1,1,1,1,1,1,1,1,1,1,1,1,1,1,1,1,1,1,1,1,1,1,1,1,1,1,1,1,1,
1,1,1,1,1,1,1,1,6),(2,2),(-1.,-0.984615384615383,-0.969230769230768,-0.953846153846152,
-0.938461538461537,-0.923076923076922,-0.907692307692306,-0.892307692307691,
-0.876923076923076,-0.86153846153846,-0.846153846153845,-0.83076923076923,
-0.815384615384614,-0.799999999999999,-0.784615384615384,-0.769230769230768,
-0.753846153846153,-0.738461538461538,-0.723076923076922,-0.707692307692307,
-0.692307692307692,-0.676923076923076,-0.661538461538461,-0.646153846153846,
-0.63076923076923,-0.615384615384615,-0.6,-0.584615384615384,-0.569230769230769,
-0.553846153846154,-0.538461538461538,-0.523076923076923,-0.507692307692308,
-0.492307692307692,-0.476923076923077,-0.461538461538462,-0.446153846153846,
-0.430769230769231,-0.415384615384615,-0.4,-0.384615384615385,-0.369230769230769,
-0.353846153846154,-0.338461538461538,-0.323076923076923,-0.307692307692308,
-0.292307692307692,-0.276923076923077,-0.261538461538462,-0.246153846153846,
-0.230769230769231,-0.215384615384615,-0.2,-0.184615384615385,-0.169230769230769,
-0.153846153846154,-0.138461538461538,-0.123076923076923,-0.107692307692308,
-0.0923076923076923,-0.0769230769230769,-0.0615384615384615,-0.0461538461538462,
-0.0307692307692308,-0.0153846153846154,0.),(-1.,1.),.UNSPECIFIED.)
GEOMETRIC_REPRESENTATION_ITEM()
RATIONAL_B_SPLINE_SURFACE(((1.,1.),(1.,1.),(1.,1.),(1.,1.),(1.,1.),(1.,
1.),(1.,1.),(1.,1.),(1.,1.),(1.,1.),(1.,1.),(1.,1.),(1.,1.),(1.,1.),(1.,
1.),(1.,1.),(1.,1.),(1.,1.),(1.,1.),(1.,1.),(1.,1.),(1.,1.),(1.,1.),(1.,
1.),(1.,1.),(1.,1.),(1.,1.),(1.,1.),(1.,1.),(1.,1.),(1.,1.),(1.,1.),(1.,
1.),(1.,1.),(1.,1.),(1.,1.),(1.,1.),(1.,1.),(1.,1.),(1.,1.),(1.,1.),(1.,
1.),(1.,1.),(1.,1.),(1.,1.),(1.,1.),(1.,1.),(1.,1.),(1.,1.),(1.,1.),(1.,
1.),(1.,1.),(1.,1.),(1.,1.),(1.,1.),(1.,1.),(1.,1.),(1.,1.),(1.,1.),(1.,
1.),(1.,1.),(1.,1.),(1.,1.),(1.,1.),(1.,1.),(1.,1.),(1.,1.),(1.,1.),(1.,
1.),(1.,1.)))
REPRESENTATION_ITEM('')
SURFACE()
);
#97=(
BOUNDED_SURFACE()
B_SPLINE_SURFACE(5,1,((#54800,#54801),(#54802,#54803),(#54804,#54805),(#54806,
#54807),(#54808,#54809),(#54810,#54811),(#54812,#54813),(#54814,#54815),
(#54816,#54817),(#54818,#54819),(#54820,#54821),(#54822,#54823),(#54824,
#54825),(#54826,#54827),(#54828,#54829),(#54830,#54831),(#54832,#54833),
(#54834,#54835),(#54836,#54837),(#54838,#54839),(#54840,#54841),(#54842,
#54843),(#54844,#54845),(#54846,#54847),(#54848,#54849),(#54850,#54851),
(#54852,#54853),(#54854,#54855),(#54856,#54857),(#54858,#54859),(#54860,
#54861),(#54862,#54863),(#54864,#54865),(#54866,#54867),(#54868,#54869),
(#54870,#54871),(#54872,#54873),(#54874,#54875),(#54876,#54877),(#54878,
#54879),(#54880,#54881),(#54882,#54883),(#54884,#54885),(#54886,#54887),
(#54888,#54889),(#54890,#54891),(#54892,#54893),(#54894,#54895),(#54896,
#54897),(#54898,#54899),(#54900,#54901),(#54902,#54903),(#54904,#54905),
(#54906,#54907),(#54908,#54909),(#54910,#54911),(#54912,#54913),(#54914,
#54915),(#54916,#54917),(#54918,#54919),(#54920,#54921),(#54922,#54923),
(#54924,#54925),(#54926,#54927),(#54928,#54929),(#54930,#54931),(#54932,
#54933),(#54934,#54935),(#54936,#54937),(#54938,#54939)),.UNSPECIFIED.,
 .F.,.F.,.F.)
B_SPLINE_SURFACE_WITH_KNOTS((6,1,1,1,1,1,1,1,1,1,1,1,1,1,1,1,1,1,1,1,1,
1,1,1,1,1,1,1,1,1,1,1,1,1,1,1,1,1,1,1,1,1,1,1,1,1,1,1,1,1,1,1,1,1,1,1,1,
1,1,1,1,1,1,1,1,6),(2,2),(-1.,-0.984615384615383,-0.969230769230768,-0.953846153846152,
-0.938461538461537,-0.923076923076922,-0.907692307692306,-0.892307692307691,
-0.876923076923076,-0.86153846153846,-0.846153846153845,-0.83076923076923,
-0.815384615384614,-0.799999999999999,-0.784615384615384,-0.769230769230768,
-0.753846153846153,-0.738461538461538,-0.723076923076922,-0.707692307692307,
-0.692307692307692,-0.676923076923076,-0.661538461538461,-0.646153846153846,
-0.63076923076923,-0.615384615384615,-0.6,-0.584615384615384,-0.569230769230769,
-0.553846153846154,-0.538461538461538,-0.523076923076923,-0.507692307692308,
-0.492307692307692,-0.476923076923077,-0.461538461538462,-0.446153846153846,
-0.430769230769231,-0.415384615384615,-0.4,-0.384615384615385,-0.369230769230769,
-0.353846153846154,-0.338461538461538,-0.323076923076923,-0.307692307692308,
-0.292307692307692,-0.276923076923077,-0.261538461538462,-0.246153846153846,
-0.230769230769231,-0.215384615384615,-0.2,-0.184615384615385,-0.169230769230769,
-0.153846153846154,-0.138461538461538,-0.123076923076923,-0.107692307692308,
-0.0923076923076923,-0.0769230769230769,-0.0615384615384615,-0.0461538461538462,
-0.0307692307692308,-0.0153846153846154,0.),(-1.,1.),.UNSPECIFIED.)
GEOMETRIC_REPRESENTATION_ITEM()
RATIONAL_B_SPLINE_SURFACE(((1.,1.),(1.,1.),(1.,1.),(1.,1.),(1.,1.),(1.,
1.),(1.,1.),(1.,1.),(1.,1.),(1.,1.),(1.,1.),(1.,1.),(1.,1.),(1.,1.),(1.,
1.),(1.,1.),(1.,1.),(1.,1.),(1.,1.),(1.,1.),(1.,1.),(1.,1.),(1.,1.),(1.,
1.),(1.,1.),(1.,1.),(1.,1.),(1.,1.),(1.,1.),(1.,1.),(1.,1.),(1.,1.),(1.,
1.),(1.,1.),(1.,1.),(1.,1.),(1.,1.),(1.,1.),(1.,1.),(1.,1.),(1.,1.),(1.,
1.),(1.,1.),(1.,1.),(1.,1.),(1.,1.),(1.,1.),(1.,1.),(1.,1.),(1.,1.),(1.,
1.),(1.,1.),(1.,1.),(1.,1.),(1.,1.),(1.,1.),(1.,1.),(1.,1.),(1.,1.),(1.,
1.),(1.,1.),(1.,1.),(1.,1.),(1.,1.),(1.,1.),(1.,1.),(1.,1.),(1.,1.),(1.,
1.),(1.,1.)))
REPRESENTATION_ITEM('')
SURFACE()
);
#98=(
BOUNDED_SURFACE()
B_SPLINE_SURFACE(5,1,((#55012,#55013),(#55014,#55015),(#55016,#55017),(#55018,
#55019),(#55020,#55021),(#55022,#55023),(#55024,#55025),(#55026,#55027),
(#55028,#55029),(#55030,#55031),(#55032,#55033),(#55034,#55035),(#55036,
#55037),(#55038,#55039),(#55040,#55041),(#55042,#55043),(#55044,#55045),
(#55046,#55047),(#55048,#55049),(#55050,#55051),(#55052,#55053),(#55054,
#55055),(#55056,#55057),(#55058,#55059),(#55060,#55061),(#55062,#55063),
(#55064,#55065),(#55066,#55067),(#55068,#55069),(#55070,#55071),(#55072,
#55073),(#55074,#55075),(#55076,#55077),(#55078,#55079),(#55080,#55081),
(#55082,#55083),(#55084,#55085),(#55086,#55087),(#55088,#55089),(#55090,
#55091),(#55092,#55093),(#55094,#55095),(#55096,#55097),(#55098,#55099),
(#55100,#55101),(#55102,#55103),(#55104,#55105),(#55106,#55107),(#55108,
#55109),(#55110,#55111),(#55112,#55113),(#55114,#55115),(#55116,#55117),
(#55118,#55119),(#55120,#55121),(#55122,#55123),(#55124,#55125),(#55126,
#55127),(#55128,#55129),(#55130,#55131),(#55132,#55133),(#55134,#55135),
(#55136,#55137),(#55138,#55139),(#55140,#55141),(#55142,#55143),(#55144,
#55145),(#55146,#55147),(#55148,#55149),(#55150,#55151)),.UNSPECIFIED.,
 .F.,.F.,.F.)
B_SPLINE_SURFACE_WITH_KNOTS((6,1,1,1,1,1,1,1,1,1,1,1,1,1,1,1,1,1,1,1,1,
1,1,1,1,1,1,1,1,1,1,1,1,1,1,1,1,1,1,1,1,1,1,1,1,1,1,1,1,1,1,1,1,1,1,1,1,
1,1,1,1,1,1,1,1,6),(2,2),(-1.,-0.984615384615383,-0.969230769230768,-0.953846153846152,
-0.938461538461537,-0.923076923076922,-0.907692307692306,-0.892307692307691,
-0.876923076923076,-0.86153846153846,-0.846153846153845,-0.83076923076923,
-0.815384615384614,-0.799999999999999,-0.784615384615384,-0.769230769230768,
-0.753846153846153,-0.738461538461538,-0.723076923076922,-0.707692307692307,
-0.692307692307692,-0.676923076923076,-0.661538461538461,-0.646153846153846,
-0.63076923076923,-0.615384615384615,-0.6,-0.584615384615384,-0.569230769230769,
-0.553846153846154,-0.538461538461538,-0.523076923076923,-0.507692307692308,
-0.492307692307692,-0.476923076923077,-0.461538461538462,-0.446153846153846,
-0.430769230769231,-0.415384615384615,-0.4,-0.384615384615385,-0.369230769230769,
-0.353846153846154,-0.338461538461538,-0.323076923076923,-0.307692307692308,
-0.292307692307692,-0.276923076923077,-0.261538461538462,-0.246153846153846,
-0.230769230769231,-0.215384615384615,-0.2,-0.184615384615385,-0.169230769230769,
-0.153846153846154,-0.138461538461538,-0.123076923076923,-0.107692307692308,
-0.0923076923076923,-0.0769230769230769,-0.0615384615384615,-0.0461538461538462,
-0.0307692307692308,-0.0153846153846154,0.),(-1.,1.),.UNSPECIFIED.)
GEOMETRIC_REPRESENTATION_ITEM()
RATIONAL_B_SPLINE_SURFACE(((1.,1.),(1.,1.),(1.,1.),(1.,1.),(1.,1.),(1.,
1.),(1.,1.),(1.,1.),(1.,1.),(1.,1.),(1.,1.),(1.,1.),(1.,1.),(1.,1.),(1.,
1.),(1.,1.),(1.,1.),(1.,1.),(1.,1.),(1.,1.),(1.,1.),(1.,1.),(1.,1.),(1.,
1.),(1.,1.),(1.,1.),(1.,1.),(1.,1.),(1.,1.),(1.,1.),(1.,1.),(1.,1.),(1.,
1.),(1.,1.),(1.,1.),(1.,1.),(1.,1.),(1.,1.),(1.,1.),(1.,1.),(1.,1.),(1.,
1.),(1.,1.),(1.,1.),(1.,1.),(1.,1.),(1.,1.),(1.,1.),(1.,1.),(1.,1.),(1.,
1.),(1.,1.),(1.,1.),(1.,1.),(1.,1.),(1.,1.),(1.,1.),(1.,1.),(1.,1.),(1.,
1.),(1.,1.),(1.,1.),(1.,1.),(1.,1.),(1.,1.),(1.,1.),(1.,1.),(1.,1.),(1.,
1.),(1.,1.)))
REPRESENTATION_ITEM('')
SURFACE()
);
#99=(
BOUNDED_SURFACE()
B_SPLINE_SURFACE(5,1,((#55242,#55243),(#55244,#55245),(#55246,#55247),(#55248,
#55249),(#55250,#55251),(#55252,#55253),(#55254,#55255),(#55256,#55257),
(#55258,#55259),(#55260,#55261),(#55262,#55263),(#55264,#55265),(#55266,
#55267),(#55268,#55269),(#55270,#55271),(#55272,#55273),(#55274,#55275),
(#55276,#55277),(#55278,#55279),(#55280,#55281),(#55282,#55283),(#55284,
#55285),(#55286,#55287),(#55288,#55289),(#55290,#55291),(#55292,#55293),
(#55294,#55295),(#55296,#55297),(#55298,#55299),(#55300,#55301),(#55302,
#55303),(#55304,#55305),(#55306,#55307),(#55308,#55309),(#55310,#55311),
(#55312,#55313),(#55314,#55315),(#55316,#55317),(#55318,#55319),(#55320,
#55321),(#55322,#55323),(#55324,#55325),(#55326,#55327),(#55328,#55329),
(#55330,#55331),(#55332,#55333),(#55334,#55335),(#55336,#55337),(#55338,
#55339),(#55340,#55341),(#55342,#55343),(#55344,#55345),(#55346,#55347),
(#55348,#55349),(#55350,#55351),(#55352,#55353),(#55354,#55355),(#55356,
#55357),(#55358,#55359),(#55360,#55361),(#55362,#55363),(#55364,#55365),
(#55366,#55367),(#55368,#55369),(#55370,#55371),(#55372,#55373),(#55374,
#55375),(#55376,#55377),(#55378,#55379),(#55380,#55381)),.UNSPECIFIED.,
 .F.,.F.,.F.)
B_SPLINE_SURFACE_WITH_KNOTS((6,1,1,1,1,1,1,1,1,1,1,1,1,1,1,1,1,1,1,1,1,
1,1,1,1,1,1,1,1,1,1,1,1,1,1,1,1,1,1,1,1,1,1,1,1,1,1,1,1,1,1,1,1,1,1,1,1,
1,1,1,1,1,1,1,1,6),(2,2),(-1.,-0.984615384615383,-0.969230769230768,-0.953846153846152,
-0.938461538461537,-0.923076923076922,-0.907692307692306,-0.892307692307691,
-0.876923076923076,-0.86153846153846,-0.846153846153845,-0.83076923076923,
-0.815384615384614,-0.799999999999999,-0.784615384615384,-0.769230769230768,
-0.753846153846153,-0.738461538461538,-0.723076923076922,-0.707692307692307,
-0.692307692307692,-0.676923076923076,-0.661538461538461,-0.646153846153846,
-0.63076923076923,-0.615384615384615,-0.6,-0.584615384615384,-0.569230769230769,
-0.553846153846154,-0.538461538461538,-0.523076923076923,-0.507692307692308,
-0.492307692307692,-0.476923076923077,-0.461538461538462,-0.446153846153846,
-0.430769230769231,-0.415384615384615,-0.4,-0.384615384615385,-0.369230769230769,
-0.353846153846154,-0.338461538461538,-0.323076923076923,-0.307692307692308,
-0.292307692307692,-0.276923076923077,-0.261538461538462,-0.246153846153846,
-0.230769230769231,-0.215384615384615,-0.2,-0.184615384615385,-0.169230769230769,
-0.153846153846154,-0.138461538461538,-0.123076923076923,-0.107692307692308,
-0.0923076923076923,-0.0769230769230769,-0.0615384615384615,-0.0461538461538462,
-0.0307692307692308,-0.0153846153846154,0.),(-1.,1.),.UNSPECIFIED.)
GEOMETRIC_REPRESENTATION_ITEM()
RATIONAL_B_SPLINE_SURFACE(((1.,1.),(1.,1.),(1.,1.),(1.,1.),(1.,1.),(1.,
1.),(1.,1.),(1.,1.),(1.,1.),(1.,1.),(1.,1.),(1.,1.),(1.,1.),(1.,1.),(1.,
1.),(1.,1.),(1.,1.),(1.,1.),(1.,1.),(1.,1.),(1.,1.),(1.,1.),(1.,1.),(1.,
1.),(1.,1.),(1.,1.),(1.,1.),(1.,1.),(1.,1.),(1.,1.),(1.,1.),(1.,1.),(1.,
1.),(1.,1.),(1.,1.),(1.,1.),(1.,1.),(1.,1.),(1.,1.),(1.,1.),(1.,1.),(1.,
1.),(1.,1.),(1.,1.),(1.,1.),(1.,1.),(1.,1.),(1.,1.),(1.,1.),(1.,1.),(1.,
1.),(1.,1.),(1.,1.),(1.,1.),(1.,1.),(1.,1.),(1.,1.),(1.,1.),(1.,1.),(1.,
1.),(1.,1.),(1.,1.),(1.,1.),(1.,1.),(1.,1.),(1.,1.),(1.,1.),(1.,1.),(1.,
1.),(1.,1.)))
REPRESENTATION_ITEM('')
SURFACE()
);
#100=(
BOUNDED_SURFACE()
B_SPLINE_SURFACE(5,1,((#55454,#55455),(#55456,#55457),(#55458,#55459),(#55460,
#55461),(#55462,#55463),(#55464,#55465),(#55466,#55467),(#55468,#55469),
(#55470,#55471),(#55472,#55473),(#55474,#55475),(#55476,#55477),(#55478,
#55479),(#55480,#55481),(#55482,#55483),(#55484,#55485),(#55486,#55487),
(#55488,#55489),(#55490,#55491),(#55492,#55493),(#55494,#55495),(#55496,
#55497),(#55498,#55499),(#55500,#55501),(#55502,#55503),(#55504,#55505),
(#55506,#55507),(#55508,#55509),(#55510,#55511),(#55512,#55513),(#55514,
#55515),(#55516,#55517),(#55518,#55519),(#55520,#55521),(#55522,#55523),
(#55524,#55525),(#55526,#55527),(#55528,#55529),(#55530,#55531),(#55532,
#55533),(#55534,#55535),(#55536,#55537),(#55538,#55539),(#55540,#55541),
(#55542,#55543),(#55544,#55545),(#55546,#55547),(#55548,#55549),(#55550,
#55551),(#55552,#55553),(#55554,#55555),(#55556,#55557),(#55558,#55559),
(#55560,#55561),(#55562,#55563),(#55564,#55565),(#55566,#55567),(#55568,
#55569),(#55570,#55571),(#55572,#55573),(#55574,#55575),(#55576,#55577),
(#55578,#55579),(#55580,#55581),(#55582,#55583),(#55584,#55585),(#55586,
#55587),(#55588,#55589),(#55590,#55591),(#55592,#55593)),.UNSPECIFIED.,
 .F.,.F.,.F.)
B_SPLINE_SURFACE_WITH_KNOTS((6,1,1,1,1,1,1,1,1,1,1,1,1,1,1,1,1,1,1,1,1,
1,1,1,1,1,1,1,1,1,1,1,1,1,1,1,1,1,1,1,1,1,1,1,1,1,1,1,1,1,1,1,1,1,1,1,1,
1,1,1,1,1,1,1,1,6),(2,2),(-1.,-0.984615384615383,-0.969230769230768,-0.953846153846152,
-0.938461538461537,-0.923076923076922,-0.907692307692306,-0.892307692307691,
-0.876923076923076,-0.86153846153846,-0.846153846153845,-0.83076923076923,
-0.815384615384614,-0.799999999999999,-0.784615384615384,-0.769230769230768,
-0.753846153846153,-0.738461538461538,-0.723076923076922,-0.707692307692307,
-0.692307692307692,-0.676923076923076,-0.661538461538461,-0.646153846153846,
-0.63076923076923,-0.615384615384615,-0.6,-0.584615384615384,-0.569230769230769,
-0.553846153846154,-0.538461538461538,-0.523076923076923,-0.507692307692308,
-0.492307692307692,-0.476923076923077,-0.461538461538462,-0.446153846153846,
-0.430769230769231,-0.415384615384615,-0.4,-0.384615384615385,-0.369230769230769,
-0.353846153846154,-0.338461538461538,-0.323076923076923,-0.307692307692308,
-0.292307692307692,-0.276923076923077,-0.261538461538462,-0.246153846153846,
-0.230769230769231,-0.215384615384615,-0.2,-0.184615384615385,-0.169230769230769,
-0.153846153846154,-0.138461538461538,-0.123076923076923,-0.107692307692308,
-0.0923076923076923,-0.0769230769230769,-0.0615384615384615,-0.0461538461538462,
-0.0307692307692308,-0.0153846153846154,0.),(-1.,1.),.UNSPECIFIED.)
GEOMETRIC_REPRESENTATION_ITEM()
RATIONAL_B_SPLINE_SURFACE(((1.,1.),(1.,1.),(1.,1.),(1.,1.),(1.,1.),(1.,
1.),(1.,1.),(1.,1.),(1.,1.),(1.,1.),(1.,1.),(1.,1.),(1.,1.),(1.,1.),(1.,
1.),(1.,1.),(1.,1.),(1.,1.),(1.,1.),(1.,1.),(1.,1.),(1.,1.),(1.,1.),(1.,
1.),(1.,1.),(1.,1.),(1.,1.),(1.,1.),(1.,1.),(1.,1.),(1.,1.),(1.,1.),(1.,
1.),(1.,1.),(1.,1.),(1.,1.),(1.,1.),(1.,1.),(1.,1.),(1.,1.),(1.,1.),(1.,
1.),(1.,1.),(1.,1.),(1.,1.),(1.,1.),(1.,1.),(1.,1.),(1.,1.),(1.,1.),(1.,
1.),(1.,1.),(1.,1.),(1.,1.),(1.,1.),(1.,1.),(1.,1.),(1.,1.),(1.,1.),(1.,
1.),(1.,1.),(1.,1.),(1.,1.),(1.,1.),(1.,1.),(1.,1.),(1.,1.),(1.,1.),(1.,
1.),(1.,1.)))
REPRESENTATION_ITEM('')
SURFACE()
);
#101=(
BOUNDED_SURFACE()
B_SPLINE_SURFACE(5,1,((#55684,#55685),(#55686,#55687),(#55688,#55689),(#55690,
#55691),(#55692,#55693),(#55694,#55695),(#55696,#55697),(#55698,#55699),
(#55700,#55701),(#55702,#55703),(#55704,#55705),(#55706,#55707),(#55708,
#55709),(#55710,#55711),(#55712,#55713),(#55714,#55715),(#55716,#55717),
(#55718,#55719),(#55720,#55721),(#55722,#55723),(#55724,#55725),(#55726,
#55727),(#55728,#55729),(#55730,#55731),(#55732,#55733),(#55734,#55735),
(#55736,#55737),(#55738,#55739),(#55740,#55741),(#55742,#55743),(#55744,
#55745),(#55746,#55747),(#55748,#55749),(#55750,#55751),(#55752,#55753),
(#55754,#55755),(#55756,#55757),(#55758,#55759),(#55760,#55761),(#55762,
#55763),(#55764,#55765),(#55766,#55767),(#55768,#55769),(#55770,#55771),
(#55772,#55773),(#55774,#55775),(#55776,#55777),(#55778,#55779),(#55780,
#55781),(#55782,#55783),(#55784,#55785),(#55786,#55787),(#55788,#55789),
(#55790,#55791),(#55792,#55793),(#55794,#55795),(#55796,#55797),(#55798,
#55799),(#55800,#55801),(#55802,#55803),(#55804,#55805),(#55806,#55807),
(#55808,#55809),(#55810,#55811),(#55812,#55813),(#55814,#55815),(#55816,
#55817),(#55818,#55819),(#55820,#55821),(#55822,#55823)),.UNSPECIFIED.,
 .F.,.F.,.F.)
B_SPLINE_SURFACE_WITH_KNOTS((6,1,1,1,1,1,1,1,1,1,1,1,1,1,1,1,1,1,1,1,1,
1,1,1,1,1,1,1,1,1,1,1,1,1,1,1,1,1,1,1,1,1,1,1,1,1,1,1,1,1,1,1,1,1,1,1,1,
1,1,1,1,1,1,1,1,6),(2,2),(-1.,-0.984615384615383,-0.969230769230768,-0.953846153846152,
-0.938461538461537,-0.923076923076922,-0.907692307692306,-0.892307692307691,
-0.876923076923076,-0.86153846153846,-0.846153846153845,-0.83076923076923,
-0.815384615384614,-0.799999999999999,-0.784615384615384,-0.769230769230768,
-0.753846153846153,-0.738461538461538,-0.723076923076922,-0.707692307692307,
-0.692307692307692,-0.676923076923076,-0.661538461538461,-0.646153846153846,
-0.63076923076923,-0.615384615384615,-0.6,-0.584615384615384,-0.569230769230769,
-0.553846153846154,-0.538461538461538,-0.523076923076923,-0.507692307692308,
-0.492307692307692,-0.476923076923077,-0.461538461538462,-0.446153846153846,
-0.430769230769231,-0.415384615384615,-0.4,-0.384615384615385,-0.369230769230769,
-0.353846153846154,-0.338461538461538,-0.323076923076923,-0.307692307692308,
-0.292307692307692,-0.276923076923077,-0.261538461538462,-0.246153846153846,
-0.230769230769231,-0.215384615384615,-0.2,-0.184615384615385,-0.169230769230769,
-0.153846153846154,-0.138461538461538,-0.123076923076923,-0.107692307692308,
-0.0923076923076923,-0.0769230769230769,-0.0615384615384615,-0.0461538461538462,
-0.0307692307692308,-0.0153846153846154,0.),(-1.,1.),.UNSPECIFIED.)
GEOMETRIC_REPRESENTATION_ITEM()
RATIONAL_B_SPLINE_SURFACE(((1.,1.),(1.,1.),(1.,1.),(1.,1.),(1.,1.),(1.,
1.),(1.,1.),(1.,1.),(1.,1.),(1.,1.),(1.,1.),(1.,1.),(1.,1.),(1.,1.),(1.,
1.),(1.,1.),(1.,1.),(1.,1.),(1.,1.),(1.,1.),(1.,1.),(1.,1.),(1.,1.),(1.,
1.),(1.,1.),(1.,1.),(1.,1.),(1.,1.),(1.,1.),(1.,1.),(1.,1.),(1.,1.),(1.,
1.),(1.,1.),(1.,1.),(1.,1.),(1.,1.),(1.,1.),(1.,1.),(1.,1.),(1.,1.),(1.,
1.),(1.,1.),(1.,1.),(1.,1.),(1.,1.),(1.,1.),(1.,1.),(1.,1.),(1.,1.),(1.,
1.),(1.,1.),(1.,1.),(1.,1.),(1.,1.),(1.,1.),(1.,1.),(1.,1.),(1.,1.),(1.,
1.),(1.,1.),(1.,1.),(1.,1.),(1.,1.),(1.,1.),(1.,1.),(1.,1.),(1.,1.),(1.,
1.),(1.,1.)))
REPRESENTATION_ITEM('')
SURFACE()
);
#102=(
BOUNDED_SURFACE()
B_SPLINE_SURFACE(5,1,((#55896,#55897),(#55898,#55899),(#55900,#55901),(#55902,
#55903),(#55904,#55905),(#55906,#55907),(#55908,#55909),(#55910,#55911),
(#55912,#55913),(#55914,#55915),(#55916,#55917),(#55918,#55919),(#55920,
#55921),(#55922,#55923),(#55924,#55925),(#55926,#55927),(#55928,#55929),
(#55930,#55931),(#55932,#55933),(#55934,#55935),(#55936,#55937),(#55938,
#55939),(#55940,#55941),(#55942,#55943),(#55944,#55945),(#55946,#55947),
(#55948,#55949),(#55950,#55951),(#55952,#55953),(#55954,#55955),(#55956,
#55957),(#55958,#55959),(#55960,#55961),(#55962,#55963),(#55964,#55965),
(#55966,#55967),(#55968,#55969),(#55970,#55971),(#55972,#55973),(#55974,
#55975),(#55976,#55977),(#55978,#55979),(#55980,#55981),(#55982,#55983),
(#55984,#55985),(#55986,#55987),(#55988,#55989),(#55990,#55991),(#55992,
#55993),(#55994,#55995),(#55996,#55997),(#55998,#55999),(#56000,#56001),
(#56002,#56003),(#56004,#56005),(#56006,#56007),(#56008,#56009),(#56010,
#56011),(#56012,#56013),(#56014,#56015),(#56016,#56017),(#56018,#56019),
(#56020,#56021),(#56022,#56023),(#56024,#56025),(#56026,#56027),(#56028,
#56029),(#56030,#56031),(#56032,#56033),(#56034,#56035)),.UNSPECIFIED.,
 .F.,.F.,.F.)
B_SPLINE_SURFACE_WITH_KNOTS((6,1,1,1,1,1,1,1,1,1,1,1,1,1,1,1,1,1,1,1,1,
1,1,1,1,1,1,1,1,1,1,1,1,1,1,1,1,1,1,1,1,1,1,1,1,1,1,1,1,1,1,1,1,1,1,1,1,
1,1,1,1,1,1,1,1,6),(2,2),(-1.,-0.984615384615383,-0.969230769230768,-0.953846153846152,
-0.938461538461537,-0.923076923076922,-0.907692307692306,-0.892307692307691,
-0.876923076923076,-0.86153846153846,-0.846153846153845,-0.83076923076923,
-0.815384615384614,-0.799999999999999,-0.784615384615384,-0.769230769230768,
-0.753846153846153,-0.738461538461538,-0.723076923076922,-0.707692307692307,
-0.692307692307692,-0.676923076923076,-0.661538461538461,-0.646153846153846,
-0.63076923076923,-0.615384615384615,-0.6,-0.584615384615384,-0.569230769230769,
-0.553846153846154,-0.538461538461538,-0.523076923076923,-0.507692307692308,
-0.492307692307692,-0.476923076923077,-0.461538461538462,-0.446153846153846,
-0.430769230769231,-0.415384615384615,-0.4,-0.384615384615385,-0.369230769230769,
-0.353846153846154,-0.338461538461538,-0.323076923076923,-0.307692307692308,
-0.292307692307692,-0.276923076923077,-0.261538461538462,-0.246153846153846,
-0.230769230769231,-0.215384615384615,-0.2,-0.184615384615385,-0.169230769230769,
-0.153846153846154,-0.138461538461538,-0.123076923076923,-0.107692307692308,
-0.0923076923076923,-0.0769230769230769,-0.0615384615384615,-0.0461538461538462,
-0.0307692307692308,-0.0153846153846154,0.),(-1.,1.),.UNSPECIFIED.)
GEOMETRIC_REPRESENTATION_ITEM()
RATIONAL_B_SPLINE_SURFACE(((1.,1.),(1.,1.),(1.,1.),(1.,1.),(1.,1.),(1.,
1.),(1.,1.),(1.,1.),(1.,1.),(1.,1.),(1.,1.),(1.,1.),(1.,1.),(1.,1.),(1.,
1.),(1.,1.),(1.,1.),(1.,1.),(1.,1.),(1.,1.),(1.,1.),(1.,1.),(1.,1.),(1.,
1.),(1.,1.),(1.,1.),(1.,1.),(1.,1.),(1.,1.),(1.,1.),(1.,1.),(1.,1.),(1.,
1.),(1.,1.),(1.,1.),(1.,1.),(1.,1.),(1.,1.),(1.,1.),(1.,1.),(1.,1.),(1.,
1.),(1.,1.),(1.,1.),(1.,1.),(1.,1.),(1.,1.),(1.,1.),(1.,1.),(1.,1.),(1.,
1.),(1.,1.),(1.,1.),(1.,1.),(1.,1.),(1.,1.),(1.,1.),(1.,1.),(1.,1.),(1.,
1.),(1.,1.),(1.,1.),(1.,1.),(1.,1.),(1.,1.),(1.,1.),(1.,1.),(1.,1.),(1.,
1.),(1.,1.)))
REPRESENTATION_ITEM('')
SURFACE()
);
#103=(
BOUNDED_SURFACE()
B_SPLINE_SURFACE(5,1,((#56126,#56127),(#56128,#56129),(#56130,#56131),(#56132,
#56133),(#56134,#56135),(#56136,#56137),(#56138,#56139),(#56140,#56141),
(#56142,#56143),(#56144,#56145),(#56146,#56147),(#56148,#56149),(#56150,
#56151),(#56152,#56153),(#56154,#56155),(#56156,#56157),(#56158,#56159),
(#56160,#56161),(#56162,#56163),(#56164,#56165),(#56166,#56167),(#56168,
#56169),(#56170,#56171),(#56172,#56173),(#56174,#56175),(#56176,#56177),
(#56178,#56179),(#56180,#56181),(#56182,#56183),(#56184,#56185),(#56186,
#56187),(#56188,#56189),(#56190,#56191),(#56192,#56193),(#56194,#56195),
(#56196,#56197),(#56198,#56199),(#56200,#56201),(#56202,#56203),(#56204,
#56205),(#56206,#56207),(#56208,#56209),(#56210,#56211),(#56212,#56213),
(#56214,#56215),(#56216,#56217),(#56218,#56219),(#56220,#56221),(#56222,
#56223),(#56224,#56225),(#56226,#56227),(#56228,#56229),(#56230,#56231),
(#56232,#56233),(#56234,#56235),(#56236,#56237),(#56238,#56239),(#56240,
#56241),(#56242,#56243),(#56244,#56245),(#56246,#56247),(#56248,#56249),
(#56250,#56251),(#56252,#56253),(#56254,#56255),(#56256,#56257),(#56258,
#56259),(#56260,#56261),(#56262,#56263),(#56264,#56265)),.UNSPECIFIED.,
 .F.,.F.,.F.)
B_SPLINE_SURFACE_WITH_KNOTS((6,1,1,1,1,1,1,1,1,1,1,1,1,1,1,1,1,1,1,1,1,
1,1,1,1,1,1,1,1,1,1,1,1,1,1,1,1,1,1,1,1,1,1,1,1,1,1,1,1,1,1,1,1,1,1,1,1,
1,1,1,1,1,1,1,1,6),(2,2),(-1.,-0.984615384615383,-0.969230769230768,-0.953846153846152,
-0.938461538461537,-0.923076923076922,-0.907692307692306,-0.892307692307691,
-0.876923076923076,-0.86153846153846,-0.846153846153845,-0.83076923076923,
-0.815384615384614,-0.799999999999999,-0.784615384615384,-0.769230769230768,
-0.753846153846153,-0.738461538461538,-0.723076923076922,-0.707692307692307,
-0.692307692307692,-0.676923076923076,-0.661538461538461,-0.646153846153846,
-0.63076923076923,-0.615384615384615,-0.6,-0.584615384615384,-0.569230769230769,
-0.553846153846154,-0.538461538461538,-0.523076923076923,-0.507692307692308,
-0.492307692307692,-0.476923076923077,-0.461538461538462,-0.446153846153846,
-0.430769230769231,-0.415384615384615,-0.4,-0.384615384615385,-0.369230769230769,
-0.353846153846154,-0.338461538461538,-0.323076923076923,-0.307692307692308,
-0.292307692307692,-0.276923076923077,-0.261538461538462,-0.246153846153846,
-0.230769230769231,-0.215384615384615,-0.2,-0.184615384615385,-0.169230769230769,
-0.153846153846154,-0.138461538461538,-0.123076923076923,-0.107692307692308,
-0.0923076923076923,-0.0769230769230769,-0.0615384615384615,-0.0461538461538462,
-0.0307692307692308,-0.0153846153846154,0.),(-1.,1.),.UNSPECIFIED.)
GEOMETRIC_REPRESENTATION_ITEM()
RATIONAL_B_SPLINE_SURFACE(((1.,1.),(1.,1.),(1.,1.),(1.,1.),(1.,1.),(1.,
1.),(1.,1.),(1.,1.),(1.,1.),(1.,1.),(1.,1.),(1.,1.),(1.,1.),(1.,1.),(1.,
1.),(1.,1.),(1.,1.),(1.,1.),(1.,1.),(1.,1.),(1.,1.),(1.,1.),(1.,1.),(1.,
1.),(1.,1.),(1.,1.),(1.,1.),(1.,1.),(1.,1.),(1.,1.),(1.,1.),(1.,1.),(1.,
1.),(1.,1.),(1.,1.),(1.,1.),(1.,1.),(1.,1.),(1.,1.),(1.,1.),(1.,1.),(1.,
1.),(1.,1.),(1.,1.),(1.,1.),(1.,1.),(1.,1.),(1.,1.),(1.,1.),(1.,1.),(1.,
1.),(1.,1.),(1.,1.),(1.,1.),(1.,1.),(1.,1.),(1.,1.),(1.,1.),(1.,1.),(1.,
1.),(1.,1.),(1.,1.),(1.,1.),(1.,1.),(1.,1.),(1.,1.),(1.,1.),(1.,1.),(1.,
1.),(1.,1.)))
REPRESENTATION_ITEM('')
SURFACE()
);
#104=(
BOUNDED_SURFACE()
B_SPLINE_SURFACE(5,1,((#56338,#56339),(#56340,#56341),(#56342,#56343),(#56344,
#56345),(#56346,#56347),(#56348,#56349),(#56350,#56351),(#56352,#56353),
(#56354,#56355),(#56356,#56357),(#56358,#56359),(#56360,#56361),(#56362,
#56363),(#56364,#56365),(#56366,#56367),(#56368,#56369),(#56370,#56371),
(#56372,#56373),(#56374,#56375),(#56376,#56377),(#56378,#56379),(#56380,
#56381),(#56382,#56383),(#56384,#56385),(#56386,#56387),(#56388,#56389),
(#56390,#56391),(#56392,#56393),(#56394,#56395),(#56396,#56397),(#56398,
#56399),(#56400,#56401),(#56402,#56403),(#56404,#56405),(#56406,#56407),
(#56408,#56409),(#56410,#56411),(#56412,#56413),(#56414,#56415),(#56416,
#56417),(#56418,#56419),(#56420,#56421),(#56422,#56423),(#56424,#56425),
(#56426,#56427),(#56428,#56429),(#56430,#56431),(#56432,#56433),(#56434,
#56435),(#56436,#56437),(#56438,#56439),(#56440,#56441),(#56442,#56443),
(#56444,#56445),(#56446,#56447),(#56448,#56449),(#56450,#56451),(#56452,
#56453),(#56454,#56455),(#56456,#56457),(#56458,#56459),(#56460,#56461),
(#56462,#56463),(#56464,#56465),(#56466,#56467),(#56468,#56469),(#56470,
#56471),(#56472,#56473),(#56474,#56475),(#56476,#56477)),.UNSPECIFIED.,
 .F.,.F.,.F.)
B_SPLINE_SURFACE_WITH_KNOTS((6,1,1,1,1,1,1,1,1,1,1,1,1,1,1,1,1,1,1,1,1,
1,1,1,1,1,1,1,1,1,1,1,1,1,1,1,1,1,1,1,1,1,1,1,1,1,1,1,1,1,1,1,1,1,1,1,1,
1,1,1,1,1,1,1,1,6),(2,2),(-1.,-0.984615384615383,-0.969230769230768,-0.953846153846152,
-0.938461538461537,-0.923076923076922,-0.907692307692306,-0.892307692307691,
-0.876923076923076,-0.86153846153846,-0.846153846153845,-0.83076923076923,
-0.815384615384614,-0.799999999999999,-0.784615384615384,-0.769230769230768,
-0.753846153846153,-0.738461538461538,-0.723076923076922,-0.707692307692307,
-0.692307692307692,-0.676923076923076,-0.661538461538461,-0.646153846153846,
-0.63076923076923,-0.615384615384615,-0.6,-0.584615384615384,-0.569230769230769,
-0.553846153846154,-0.538461538461538,-0.523076923076923,-0.507692307692308,
-0.492307692307692,-0.476923076923077,-0.461538461538462,-0.446153846153846,
-0.430769230769231,-0.415384615384615,-0.4,-0.384615384615385,-0.369230769230769,
-0.353846153846154,-0.338461538461538,-0.323076923076923,-0.307692307692308,
-0.292307692307692,-0.276923076923077,-0.261538461538462,-0.246153846153846,
-0.230769230769231,-0.215384615384615,-0.2,-0.184615384615385,-0.169230769230769,
-0.153846153846154,-0.138461538461538,-0.123076923076923,-0.107692307692308,
-0.0923076923076923,-0.0769230769230769,-0.0615384615384615,-0.0461538461538462,
-0.0307692307692308,-0.0153846153846154,0.),(-1.,1.),.UNSPECIFIED.)
GEOMETRIC_REPRESENTATION_ITEM()
RATIONAL_B_SPLINE_SURFACE(((1.,1.),(1.,1.),(1.,1.),(1.,1.),(1.,1.),(1.,
1.),(1.,1.),(1.,1.),(1.,1.),(1.,1.),(1.,1.),(1.,1.),(1.,1.),(1.,1.),(1.,
1.),(1.,1.),(1.,1.),(1.,1.),(1.,1.),(1.,1.),(1.,1.),(1.,1.),(1.,1.),(1.,
1.),(1.,1.),(1.,1.),(1.,1.),(1.,1.),(1.,1.),(1.,1.),(1.,1.),(1.,1.),(1.,
1.),(1.,1.),(1.,1.),(1.,1.),(1.,1.),(1.,1.),(1.,1.),(1.,1.),(1.,1.),(1.,
1.),(1.,1.),(1.,1.),(1.,1.),(1.,1.),(1.,1.),(1.,1.),(1.,1.),(1.,1.),(1.,
1.),(1.,1.),(1.,1.),(1.,1.),(1.,1.),(1.,1.),(1.,1.),(1.,1.),(1.,1.),(1.,
1.),(1.,1.),(1.,1.),(1.,1.),(1.,1.),(1.,1.),(1.,1.),(1.,1.),(1.,1.),(1.,
1.),(1.,1.)))
REPRESENTATION_ITEM('')
SURFACE()
);
#105=(
BOUNDED_SURFACE()
B_SPLINE_SURFACE(5,1,((#56568,#56569),(#56570,#56571),(#56572,#56573),(#56574,
#56575),(#56576,#56577),(#56578,#56579),(#56580,#56581),(#56582,#56583),
(#56584,#56585),(#56586,#56587),(#56588,#56589),(#56590,#56591),(#56592,
#56593),(#56594,#56595),(#56596,#56597),(#56598,#56599),(#56600,#56601),
(#56602,#56603),(#56604,#56605),(#56606,#56607),(#56608,#56609),(#56610,
#56611),(#56612,#56613),(#56614,#56615),(#56616,#56617),(#56618,#56619),
(#56620,#56621),(#56622,#56623),(#56624,#56625),(#56626,#56627),(#56628,
#56629),(#56630,#56631),(#56632,#56633),(#56634,#56635),(#56636,#56637),
(#56638,#56639),(#56640,#56641),(#56642,#56643),(#56644,#56645),(#56646,
#56647),(#56648,#56649),(#56650,#56651),(#56652,#56653),(#56654,#56655),
(#56656,#56657),(#56658,#56659),(#56660,#56661),(#56662,#56663),(#56664,
#56665),(#56666,#56667),(#56668,#56669),(#56670,#56671),(#56672,#56673),
(#56674,#56675),(#56676,#56677),(#56678,#56679),(#56680,#56681),(#56682,
#56683),(#56684,#56685),(#56686,#56687),(#56688,#56689),(#56690,#56691),
(#56692,#56693),(#56694,#56695),(#56696,#56697),(#56698,#56699),(#56700,
#56701),(#56702,#56703),(#56704,#56705),(#56706,#56707)),.UNSPECIFIED.,
 .F.,.F.,.F.)
B_SPLINE_SURFACE_WITH_KNOTS((6,1,1,1,1,1,1,1,1,1,1,1,1,1,1,1,1,1,1,1,1,
1,1,1,1,1,1,1,1,1,1,1,1,1,1,1,1,1,1,1,1,1,1,1,1,1,1,1,1,1,1,1,1,1,1,1,1,
1,1,1,1,1,1,1,1,6),(2,2),(-1.,-0.984615384615383,-0.969230769230768,-0.953846153846152,
-0.938461538461537,-0.923076923076922,-0.907692307692306,-0.892307692307691,
-0.876923076923076,-0.86153846153846,-0.846153846153845,-0.83076923076923,
-0.815384615384614,-0.799999999999999,-0.784615384615384,-0.769230769230768,
-0.753846153846153,-0.738461538461538,-0.723076923076922,-0.707692307692307,
-0.692307692307692,-0.676923076923076,-0.661538461538461,-0.646153846153846,
-0.63076923076923,-0.615384615384615,-0.6,-0.584615384615384,-0.569230769230769,
-0.553846153846154,-0.538461538461538,-0.523076923076923,-0.507692307692308,
-0.492307692307692,-0.476923076923077,-0.461538461538462,-0.446153846153846,
-0.430769230769231,-0.415384615384615,-0.4,-0.384615384615385,-0.369230769230769,
-0.353846153846154,-0.338461538461538,-0.323076923076923,-0.307692307692308,
-0.292307692307692,-0.276923076923077,-0.261538461538462,-0.246153846153846,
-0.230769230769231,-0.215384615384615,-0.2,-0.184615384615385,-0.169230769230769,
-0.153846153846154,-0.138461538461538,-0.123076923076923,-0.107692307692308,
-0.0923076923076923,-0.0769230769230769,-0.0615384615384615,-0.0461538461538462,
-0.0307692307692308,-0.0153846153846154,0.),(-1.,1.),.UNSPECIFIED.)
GEOMETRIC_REPRESENTATION_ITEM()
RATIONAL_B_SPLINE_SURFACE(((1.,1.),(1.,1.),(1.,1.),(1.,1.),(1.,1.),(1.,
1.),(1.,1.),(1.,1.),(1.,1.),(1.,1.),(1.,1.),(1.,1.),(1.,1.),(1.,1.),(1.,
1.),(1.,1.),(1.,1.),(1.,1.),(1.,1.),(1.,1.),(1.,1.),(1.,1.),(1.,1.),(1.,
1.),(1.,1.),(1.,1.),(1.,1.),(1.,1.),(1.,1.),(1.,1.),(1.,1.),(1.,1.),(1.,
1.),(1.,1.),(1.,1.),(1.,1.),(1.,1.),(1.,1.),(1.,1.),(1.,1.),(1.,1.),(1.,
1.),(1.,1.),(1.,1.),(1.,1.),(1.,1.),(1.,1.),(1.,1.),(1.,1.),(1.,1.),(1.,
1.),(1.,1.),(1.,1.),(1.,1.),(1.,1.),(1.,1.),(1.,1.),(1.,1.),(1.,1.),(1.,
1.),(1.,1.),(1.,1.),(1.,1.),(1.,1.),(1.,1.),(1.,1.),(1.,1.),(1.,1.),(1.,
1.),(1.,1.)))
REPRESENTATION_ITEM('')
SURFACE()
);
#106=(
BOUNDED_SURFACE()
B_SPLINE_SURFACE(5,1,((#56780,#56781),(#56782,#56783),(#56784,#56785),(#56786,
#56787),(#56788,#56789),(#56790,#56791),(#56792,#56793),(#56794,#56795),
(#56796,#56797),(#56798,#56799),(#56800,#56801),(#56802,#56803),(#56804,
#56805),(#56806,#56807),(#56808,#56809),(#56810,#56811),(#56812,#56813),
(#56814,#56815),(#56816,#56817),(#56818,#56819),(#56820,#56821),(#56822,
#56823),(#56824,#56825),(#56826,#56827),(#56828,#56829),(#56830,#56831),
(#56832,#56833),(#56834,#56835),(#56836,#56837),(#56838,#56839),(#56840,
#56841),(#56842,#56843),(#56844,#56845),(#56846,#56847),(#56848,#56849),
(#56850,#56851),(#56852,#56853),(#56854,#56855),(#56856,#56857),(#56858,
#56859),(#56860,#56861),(#56862,#56863),(#56864,#56865),(#56866,#56867),
(#56868,#56869),(#56870,#56871),(#56872,#56873),(#56874,#56875),(#56876,
#56877),(#56878,#56879),(#56880,#56881),(#56882,#56883),(#56884,#56885),
(#56886,#56887),(#56888,#56889),(#56890,#56891),(#56892,#56893),(#56894,
#56895),(#56896,#56897),(#56898,#56899),(#56900,#56901),(#56902,#56903),
(#56904,#56905),(#56906,#56907),(#56908,#56909),(#56910,#56911),(#56912,
#56913),(#56914,#56915),(#56916,#56917),(#56918,#56919)),.UNSPECIFIED.,
 .F.,.F.,.F.)
B_SPLINE_SURFACE_WITH_KNOTS((6,1,1,1,1,1,1,1,1,1,1,1,1,1,1,1,1,1,1,1,1,
1,1,1,1,1,1,1,1,1,1,1,1,1,1,1,1,1,1,1,1,1,1,1,1,1,1,1,1,1,1,1,1,1,1,1,1,
1,1,1,1,1,1,1,1,6),(2,2),(-1.,-0.984615384615383,-0.969230769230768,-0.953846153846152,
-0.938461538461537,-0.923076923076922,-0.907692307692306,-0.892307692307691,
-0.876923076923076,-0.86153846153846,-0.846153846153845,-0.83076923076923,
-0.815384615384614,-0.799999999999999,-0.784615384615384,-0.769230769230768,
-0.753846153846153,-0.738461538461538,-0.723076923076922,-0.707692307692307,
-0.692307692307692,-0.676923076923076,-0.661538461538461,-0.646153846153846,
-0.63076923076923,-0.615384615384615,-0.6,-0.584615384615384,-0.569230769230769,
-0.553846153846154,-0.538461538461538,-0.523076923076923,-0.507692307692308,
-0.492307692307692,-0.476923076923077,-0.461538461538462,-0.446153846153846,
-0.430769230769231,-0.415384615384615,-0.4,-0.384615384615385,-0.369230769230769,
-0.353846153846154,-0.338461538461538,-0.323076923076923,-0.307692307692308,
-0.292307692307692,-0.276923076923077,-0.261538461538462,-0.246153846153846,
-0.230769230769231,-0.215384615384615,-0.2,-0.184615384615385,-0.169230769230769,
-0.153846153846154,-0.138461538461538,-0.123076923076923,-0.107692307692308,
-0.0923076923076923,-0.0769230769230769,-0.0615384615384615,-0.0461538461538462,
-0.0307692307692308,-0.0153846153846154,0.),(-1.,1.),.UNSPECIFIED.)
GEOMETRIC_REPRESENTATION_ITEM()
RATIONAL_B_SPLINE_SURFACE(((1.,1.),(1.,1.),(1.,1.),(1.,1.),(1.,1.),(1.,
1.),(1.,1.),(1.,1.),(1.,1.),(1.,1.),(1.,1.),(1.,1.),(1.,1.),(1.,1.),(1.,
1.),(1.,1.),(1.,1.),(1.,1.),(1.,1.),(1.,1.),(1.,1.),(1.,1.),(1.,1.),(1.,
1.),(1.,1.),(1.,1.),(1.,1.),(1.,1.),(1.,1.),(1.,1.),(1.,1.),(1.,1.),(1.,
1.),(1.,1.),(1.,1.),(1.,1.),(1.,1.),(1.,1.),(1.,1.),(1.,1.),(1.,1.),(1.,
1.),(1.,1.),(1.,1.),(1.,1.),(1.,1.),(1.,1.),(1.,1.),(1.,1.),(1.,1.),(1.,
1.),(1.,1.),(1.,1.),(1.,1.),(1.,1.),(1.,1.),(1.,1.),(1.,1.),(1.,1.),(1.,
1.),(1.,1.),(1.,1.),(1.,1.),(1.,1.),(1.,1.),(1.,1.),(1.,1.),(1.,1.),(1.,
1.),(1.,1.)))
REPRESENTATION_ITEM('')
SURFACE()
);
#107=(
BOUNDED_SURFACE()
B_SPLINE_SURFACE(5,1,((#57010,#57011),(#57012,#57013),(#57014,#57015),(#57016,
#57017),(#57018,#57019),(#57020,#57021),(#57022,#57023),(#57024,#57025),
(#57026,#57027),(#57028,#57029),(#57030,#57031),(#57032,#57033),(#57034,
#57035),(#57036,#57037),(#57038,#57039),(#57040,#57041),(#57042,#57043),
(#57044,#57045),(#57046,#57047),(#57048,#57049),(#57050,#57051),(#57052,
#57053),(#57054,#57055),(#57056,#57057),(#57058,#57059),(#57060,#57061),
(#57062,#57063),(#57064,#57065),(#57066,#57067),(#57068,#57069),(#57070,
#57071),(#57072,#57073),(#57074,#57075),(#57076,#57077),(#57078,#57079),
(#57080,#57081),(#57082,#57083),(#57084,#57085),(#57086,#57087),(#57088,
#57089),(#57090,#57091),(#57092,#57093),(#57094,#57095),(#57096,#57097),
(#57098,#57099),(#57100,#57101),(#57102,#57103),(#57104,#57105),(#57106,
#57107),(#57108,#57109),(#57110,#57111),(#57112,#57113),(#57114,#57115),
(#57116,#57117),(#57118,#57119),(#57120,#57121),(#57122,#57123),(#57124,
#57125),(#57126,#57127),(#57128,#57129),(#57130,#57131),(#57132,#57133),
(#57134,#57135),(#57136,#57137),(#57138,#57139),(#57140,#57141),(#57142,
#57143),(#57144,#57145),(#57146,#57147),(#57148,#57149)),.UNSPECIFIED.,
 .F.,.F.,.F.)
B_SPLINE_SURFACE_WITH_KNOTS((6,1,1,1,1,1,1,1,1,1,1,1,1,1,1,1,1,1,1,1,1,
1,1,1,1,1,1,1,1,1,1,1,1,1,1,1,1,1,1,1,1,1,1,1,1,1,1,1,1,1,1,1,1,1,1,1,1,
1,1,1,1,1,1,1,1,6),(2,2),(-1.,-0.984615384615383,-0.969230769230768,-0.953846153846152,
-0.938461538461537,-0.923076923076922,-0.907692307692306,-0.892307692307691,
-0.876923076923076,-0.86153846153846,-0.846153846153845,-0.83076923076923,
-0.815384615384614,-0.799999999999999,-0.784615384615384,-0.769230769230768,
-0.753846153846153,-0.738461538461538,-0.723076923076922,-0.707692307692307,
-0.692307692307692,-0.676923076923076,-0.661538461538461,-0.646153846153846,
-0.63076923076923,-0.615384615384615,-0.6,-0.584615384615384,-0.569230769230769,
-0.553846153846154,-0.538461538461538,-0.523076923076923,-0.507692307692308,
-0.492307692307692,-0.476923076923077,-0.461538461538462,-0.446153846153846,
-0.430769230769231,-0.415384615384615,-0.4,-0.384615384615385,-0.369230769230769,
-0.353846153846154,-0.338461538461538,-0.323076923076923,-0.307692307692308,
-0.292307692307692,-0.276923076923077,-0.261538461538462,-0.246153846153846,
-0.230769230769231,-0.215384615384615,-0.2,-0.184615384615385,-0.169230769230769,
-0.153846153846154,-0.138461538461538,-0.123076923076923,-0.107692307692308,
-0.0923076923076923,-0.0769230769230769,-0.0615384615384615,-0.0461538461538462,
-0.0307692307692308,-0.0153846153846154,0.),(-1.,1.),.UNSPECIFIED.)
GEOMETRIC_REPRESENTATION_ITEM()
RATIONAL_B_SPLINE_SURFACE(((1.,1.),(1.,1.),(1.,1.),(1.,1.),(1.,1.),(1.,
1.),(1.,1.),(1.,1.),(1.,1.),(1.,1.),(1.,1.),(1.,1.),(1.,1.),(1.,1.),(1.,
1.),(1.,1.),(1.,1.),(1.,1.),(1.,1.),(1.,1.),(1.,1.),(1.,1.),(1.,1.),(1.,
1.),(1.,1.),(1.,1.),(1.,1.),(1.,1.),(1.,1.),(1.,1.),(1.,1.),(1.,1.),(1.,
1.),(1.,1.),(1.,1.),(1.,1.),(1.,1.),(1.,1.),(1.,1.),(1.,1.),(1.,1.),(1.,
1.),(1.,1.),(1.,1.),(1.,1.),(1.,1.),(1.,1.),(1.,1.),(1.,1.),(1.,1.),(1.,
1.),(1.,1.),(1.,1.),(1.,1.),(1.,1.),(1.,1.),(1.,1.),(1.,1.),(1.,1.),(1.,
1.),(1.,1.),(1.,1.),(1.,1.),(1.,1.),(1.,1.),(1.,1.),(1.,1.),(1.,1.),(1.,
1.),(1.,1.)))
REPRESENTATION_ITEM('')
SURFACE()
);
#108=(
BOUNDED_SURFACE()
B_SPLINE_SURFACE(5,1,((#57222,#57223),(#57224,#57225),(#57226,#57227),(#57228,
#57229),(#57230,#57231),(#57232,#57233),(#57234,#57235),(#57236,#57237),
(#57238,#57239),(#57240,#57241),(#57242,#57243),(#57244,#57245),(#57246,
#57247),(#57248,#57249),(#57250,#57251),(#57252,#57253),(#57254,#57255),
(#57256,#57257),(#57258,#57259),(#57260,#57261),(#57262,#57263),(#57264,
#57265),(#57266,#57267),(#57268,#57269),(#57270,#57271),(#57272,#57273),
(#57274,#57275),(#57276,#57277),(#57278,#57279),(#57280,#57281),(#57282,
#57283),(#57284,#57285),(#57286,#57287),(#57288,#57289),(#57290,#57291),
(#57292,#57293),(#57294,#57295),(#57296,#57297),(#57298,#57299),(#57300,
#57301),(#57302,#57303),(#57304,#57305),(#57306,#57307),(#57308,#57309),
(#57310,#57311),(#57312,#57313),(#57314,#57315),(#57316,#57317),(#57318,
#57319),(#57320,#57321),(#57322,#57323),(#57324,#57325),(#57326,#57327),
(#57328,#57329),(#57330,#57331),(#57332,#57333),(#57334,#57335),(#57336,
#57337),(#57338,#57339),(#57340,#57341),(#57342,#57343),(#57344,#57345),
(#57346,#57347),(#57348,#57349),(#57350,#57351),(#57352,#57353),(#57354,
#57355),(#57356,#57357),(#57358,#57359),(#57360,#57361)),.UNSPECIFIED.,
 .F.,.F.,.F.)
B_SPLINE_SURFACE_WITH_KNOTS((6,1,1,1,1,1,1,1,1,1,1,1,1,1,1,1,1,1,1,1,1,
1,1,1,1,1,1,1,1,1,1,1,1,1,1,1,1,1,1,1,1,1,1,1,1,1,1,1,1,1,1,1,1,1,1,1,1,
1,1,1,1,1,1,1,1,6),(2,2),(-1.,-0.984615384615383,-0.969230769230768,-0.953846153846152,
-0.938461538461537,-0.923076923076922,-0.907692307692306,-0.892307692307691,
-0.876923076923076,-0.86153846153846,-0.846153846153845,-0.83076923076923,
-0.815384615384614,-0.799999999999999,-0.784615384615384,-0.769230769230768,
-0.753846153846153,-0.738461538461538,-0.723076923076922,-0.707692307692307,
-0.692307692307692,-0.676923076923076,-0.661538461538461,-0.646153846153846,
-0.63076923076923,-0.615384615384615,-0.6,-0.584615384615384,-0.569230769230769,
-0.553846153846154,-0.538461538461538,-0.523076923076923,-0.507692307692308,
-0.492307692307692,-0.476923076923077,-0.461538461538462,-0.446153846153846,
-0.430769230769231,-0.415384615384615,-0.4,-0.384615384615385,-0.369230769230769,
-0.353846153846154,-0.338461538461538,-0.323076923076923,-0.307692307692308,
-0.292307692307692,-0.276923076923077,-0.261538461538462,-0.246153846153846,
-0.230769230769231,-0.215384615384615,-0.2,-0.184615384615385,-0.169230769230769,
-0.153846153846154,-0.138461538461538,-0.123076923076923,-0.107692307692308,
-0.0923076923076923,-0.0769230769230769,-0.0615384615384615,-0.0461538461538462,
-0.0307692307692308,-0.0153846153846154,0.),(-1.,1.),.UNSPECIFIED.)
GEOMETRIC_REPRESENTATION_ITEM()
RATIONAL_B_SPLINE_SURFACE(((1.,1.),(1.,1.),(1.,1.),(1.,1.),(1.,1.),(1.,
1.),(1.,1.),(1.,1.),(1.,1.),(1.,1.),(1.,1.),(1.,1.),(1.,1.),(1.,1.),(1.,
1.),(1.,1.),(1.,1.),(1.,1.),(1.,1.),(1.,1.),(1.,1.),(1.,1.),(1.,1.),(1.,
1.),(1.,1.),(1.,1.),(1.,1.),(1.,1.),(1.,1.),(1.,1.),(1.,1.),(1.,1.),(1.,
1.),(1.,1.),(1.,1.),(1.,1.),(1.,1.),(1.,1.),(1.,1.),(1.,1.),(1.,1.),(1.,
1.),(1.,1.),(1.,1.),(1.,1.),(1.,1.),(1.,1.),(1.,1.),(1.,1.),(1.,1.),(1.,
1.),(1.,1.),(1.,1.),(1.,1.),(1.,1.),(1.,1.),(1.,1.),(1.,1.),(1.,1.),(1.,
1.),(1.,1.),(1.,1.),(1.,1.),(1.,1.),(1.,1.),(1.,1.),(1.,1.),(1.,1.),(1.,
1.),(1.,1.)))
REPRESENTATION_ITEM('')
SURFACE()
);
#109=(
BOUNDED_SURFACE()
B_SPLINE_SURFACE(5,1,((#57452,#57453),(#57454,#57455),(#57456,#57457),(#57458,
#57459),(#57460,#57461),(#57462,#57463),(#57464,#57465),(#57466,#57467),
(#57468,#57469),(#57470,#57471),(#57472,#57473),(#57474,#57475),(#57476,
#57477),(#57478,#57479),(#57480,#57481),(#57482,#57483),(#57484,#57485),
(#57486,#57487),(#57488,#57489),(#57490,#57491),(#57492,#57493),(#57494,
#57495),(#57496,#57497),(#57498,#57499),(#57500,#57501),(#57502,#57503),
(#57504,#57505),(#57506,#57507),(#57508,#57509),(#57510,#57511),(#57512,
#57513),(#57514,#57515),(#57516,#57517),(#57518,#57519),(#57520,#57521),
(#57522,#57523),(#57524,#57525),(#57526,#57527),(#57528,#57529),(#57530,
#57531),(#57532,#57533),(#57534,#57535),(#57536,#57537),(#57538,#57539),
(#57540,#57541),(#57542,#57543),(#57544,#57545),(#57546,#57547),(#57548,
#57549),(#57550,#57551),(#57552,#57553),(#57554,#57555),(#57556,#57557),
(#57558,#57559),(#57560,#57561),(#57562,#57563),(#57564,#57565),(#57566,
#57567),(#57568,#57569),(#57570,#57571),(#57572,#57573),(#57574,#57575),
(#57576,#57577),(#57578,#57579),(#57580,#57581),(#57582,#57583),(#57584,
#57585),(#57586,#57587),(#57588,#57589),(#57590,#57591)),.UNSPECIFIED.,
 .F.,.F.,.F.)
B_SPLINE_SURFACE_WITH_KNOTS((6,1,1,1,1,1,1,1,1,1,1,1,1,1,1,1,1,1,1,1,1,
1,1,1,1,1,1,1,1,1,1,1,1,1,1,1,1,1,1,1,1,1,1,1,1,1,1,1,1,1,1,1,1,1,1,1,1,
1,1,1,1,1,1,1,1,6),(2,2),(-1.,-0.984615384615383,-0.969230769230768,-0.953846153846152,
-0.938461538461537,-0.923076923076922,-0.907692307692306,-0.892307692307691,
-0.876923076923076,-0.86153846153846,-0.846153846153845,-0.83076923076923,
-0.815384615384614,-0.799999999999999,-0.784615384615384,-0.769230769230768,
-0.753846153846153,-0.738461538461538,-0.723076923076922,-0.707692307692307,
-0.692307692307692,-0.676923076923076,-0.661538461538461,-0.646153846153846,
-0.63076923076923,-0.615384615384615,-0.6,-0.584615384615384,-0.569230769230769,
-0.553846153846154,-0.538461538461538,-0.523076923076923,-0.507692307692308,
-0.492307692307692,-0.476923076923077,-0.461538461538462,-0.446153846153846,
-0.430769230769231,-0.415384615384615,-0.4,-0.384615384615385,-0.369230769230769,
-0.353846153846154,-0.338461538461538,-0.323076923076923,-0.307692307692308,
-0.292307692307692,-0.276923076923077,-0.261538461538462,-0.246153846153846,
-0.230769230769231,-0.215384615384615,-0.2,-0.184615384615385,-0.169230769230769,
-0.153846153846154,-0.138461538461538,-0.123076923076923,-0.107692307692308,
-0.0923076923076923,-0.0769230769230769,-0.0615384615384615,-0.0461538461538462,
-0.0307692307692308,-0.0153846153846154,0.),(-1.,1.),.UNSPECIFIED.)
GEOMETRIC_REPRESENTATION_ITEM()
RATIONAL_B_SPLINE_SURFACE(((1.,1.),(1.,1.),(1.,1.),(1.,1.),(1.,1.),(1.,
1.),(1.,1.),(1.,1.),(1.,1.),(1.,1.),(1.,1.),(1.,1.),(1.,1.),(1.,1.),(1.,
1.),(1.,1.),(1.,1.),(1.,1.),(1.,1.),(1.,1.),(1.,1.),(1.,1.),(1.,1.),(1.,
1.),(1.,1.),(1.,1.),(1.,1.),(1.,1.),(1.,1.),(1.,1.),(1.,1.),(1.,1.),(1.,
1.),(1.,1.),(1.,1.),(1.,1.),(1.,1.),(1.,1.),(1.,1.),(1.,1.),(1.,1.),(1.,
1.),(1.,1.),(1.,1.),(1.,1.),(1.,1.),(1.,1.),(1.,1.),(1.,1.),(1.,1.),(1.,
1.),(1.,1.),(1.,1.),(1.,1.),(1.,1.),(1.,1.),(1.,1.),(1.,1.),(1.,1.),(1.,
1.),(1.,1.),(1.,1.),(1.,1.),(1.,1.),(1.,1.),(1.,1.),(1.,1.),(1.,1.),(1.,
1.),(1.,1.)))
REPRESENTATION_ITEM('')
SURFACE()
);
#110=(
BOUNDED_SURFACE()
B_SPLINE_SURFACE(5,1,((#57664,#57665),(#57666,#57667),(#57668,#57669),(#57670,
#57671),(#57672,#57673),(#57674,#57675),(#57676,#57677),(#57678,#57679),
(#57680,#57681),(#57682,#57683),(#57684,#57685),(#57686,#57687),(#57688,
#57689),(#57690,#57691),(#57692,#57693),(#57694,#57695),(#57696,#57697),
(#57698,#57699),(#57700,#57701),(#57702,#57703),(#57704,#57705),(#57706,
#57707),(#57708,#57709),(#57710,#57711),(#57712,#57713),(#57714,#57715),
(#57716,#57717),(#57718,#57719),(#57720,#57721),(#57722,#57723),(#57724,
#57725),(#57726,#57727),(#57728,#57729),(#57730,#57731),(#57732,#57733),
(#57734,#57735),(#57736,#57737),(#57738,#57739),(#57740,#57741),(#57742,
#57743),(#57744,#57745),(#57746,#57747),(#57748,#57749),(#57750,#57751),
(#57752,#57753),(#57754,#57755),(#57756,#57757),(#57758,#57759),(#57760,
#57761),(#57762,#57763),(#57764,#57765),(#57766,#57767),(#57768,#57769),
(#57770,#57771),(#57772,#57773),(#57774,#57775),(#57776,#57777),(#57778,
#57779),(#57780,#57781),(#57782,#57783),(#57784,#57785),(#57786,#57787),
(#57788,#57789),(#57790,#57791),(#57792,#57793),(#57794,#57795),(#57796,
#57797),(#57798,#57799),(#57800,#57801),(#57802,#57803)),.UNSPECIFIED.,
 .F.,.F.,.F.)
B_SPLINE_SURFACE_WITH_KNOTS((6,1,1,1,1,1,1,1,1,1,1,1,1,1,1,1,1,1,1,1,1,
1,1,1,1,1,1,1,1,1,1,1,1,1,1,1,1,1,1,1,1,1,1,1,1,1,1,1,1,1,1,1,1,1,1,1,1,
1,1,1,1,1,1,1,1,6),(2,2),(-1.,-0.984615384615383,-0.969230769230768,-0.953846153846152,
-0.938461538461537,-0.923076923076922,-0.907692307692306,-0.892307692307691,
-0.876923076923076,-0.86153846153846,-0.846153846153845,-0.83076923076923,
-0.815384615384614,-0.799999999999999,-0.784615384615384,-0.769230769230768,
-0.753846153846153,-0.738461538461538,-0.723076923076922,-0.707692307692307,
-0.692307692307692,-0.676923076923076,-0.661538461538461,-0.646153846153846,
-0.63076923076923,-0.615384615384615,-0.6,-0.584615384615384,-0.569230769230769,
-0.553846153846154,-0.538461538461538,-0.523076923076923,-0.507692307692308,
-0.492307692307692,-0.476923076923077,-0.461538461538462,-0.446153846153846,
-0.430769230769231,-0.415384615384615,-0.4,-0.384615384615385,-0.369230769230769,
-0.353846153846154,-0.338461538461538,-0.323076923076923,-0.307692307692308,
-0.292307692307692,-0.276923076923077,-0.261538461538462,-0.246153846153846,
-0.230769230769231,-0.215384615384615,-0.2,-0.184615384615385,-0.169230769230769,
-0.153846153846154,-0.138461538461538,-0.123076923076923,-0.107692307692308,
-0.0923076923076923,-0.0769230769230769,-0.0615384615384615,-0.0461538461538462,
-0.0307692307692308,-0.0153846153846154,0.),(-1.,1.),.UNSPECIFIED.)
GEOMETRIC_REPRESENTATION_ITEM()
RATIONAL_B_SPLINE_SURFACE(((1.,1.),(1.,1.),(1.,1.),(1.,1.),(1.,1.),(1.,
1.),(1.,1.),(1.,1.),(1.,1.),(1.,1.),(1.,1.),(1.,1.),(1.,1.),(1.,1.),(1.,
1.),(1.,1.),(1.,1.),(1.,1.),(1.,1.),(1.,1.),(1.,1.),(1.,1.),(1.,1.),(1.,
1.),(1.,1.),(1.,1.),(1.,1.),(1.,1.),(1.,1.),(1.,1.),(1.,1.),(1.,1.),(1.,
1.),(1.,1.),(1.,1.),(1.,1.),(1.,1.),(1.,1.),(1.,1.),(1.,1.),(1.,1.),(1.,
1.),(1.,1.),(1.,1.),(1.,1.),(1.,1.),(1.,1.),(1.,1.),(1.,1.),(1.,1.),(1.,
1.),(1.,1.),(1.,1.),(1.,1.),(1.,1.),(1.,1.),(1.,1.),(1.,1.),(1.,1.),(1.,
1.),(1.,1.),(1.,1.),(1.,1.),(1.,1.),(1.,1.),(1.,1.),(1.,1.),(1.,1.),(1.,
1.),(1.,1.)))
REPRESENTATION_ITEM('')
SURFACE()
);
#111=(
BOUNDED_SURFACE()
B_SPLINE_SURFACE(5,1,((#57894,#57895),(#57896,#57897),(#57898,#57899),(#57900,
#57901),(#57902,#57903),(#57904,#57905),(#57906,#57907),(#57908,#57909),
(#57910,#57911),(#57912,#57913),(#57914,#57915),(#57916,#57917),(#57918,
#57919),(#57920,#57921),(#57922,#57923),(#57924,#57925),(#57926,#57927),
(#57928,#57929),(#57930,#57931),(#57932,#57933),(#57934,#57935),(#57936,
#57937),(#57938,#57939),(#57940,#57941),(#57942,#57943),(#57944,#57945),
(#57946,#57947),(#57948,#57949),(#57950,#57951),(#57952,#57953),(#57954,
#57955),(#57956,#57957),(#57958,#57959),(#57960,#57961),(#57962,#57963),
(#57964,#57965),(#57966,#57967),(#57968,#57969),(#57970,#57971),(#57972,
#57973),(#57974,#57975),(#57976,#57977),(#57978,#57979),(#57980,#57981),
(#57982,#57983),(#57984,#57985),(#57986,#57987),(#57988,#57989),(#57990,
#57991),(#57992,#57993),(#57994,#57995),(#57996,#57997),(#57998,#57999),
(#58000,#58001),(#58002,#58003),(#58004,#58005),(#58006,#58007),(#58008,
#58009),(#58010,#58011),(#58012,#58013),(#58014,#58015),(#58016,#58017),
(#58018,#58019),(#58020,#58021),(#58022,#58023),(#58024,#58025),(#58026,
#58027),(#58028,#58029),(#58030,#58031),(#58032,#58033)),.UNSPECIFIED.,
 .F.,.F.,.F.)
B_SPLINE_SURFACE_WITH_KNOTS((6,1,1,1,1,1,1,1,1,1,1,1,1,1,1,1,1,1,1,1,1,
1,1,1,1,1,1,1,1,1,1,1,1,1,1,1,1,1,1,1,1,1,1,1,1,1,1,1,1,1,1,1,1,1,1,1,1,
1,1,1,1,1,1,1,1,6),(2,2),(-1.,-0.984615384615383,-0.969230769230768,-0.953846153846152,
-0.938461538461537,-0.923076923076922,-0.907692307692306,-0.892307692307691,
-0.876923076923076,-0.86153846153846,-0.846153846153845,-0.83076923076923,
-0.815384615384614,-0.799999999999999,-0.784615384615384,-0.769230769230768,
-0.753846153846153,-0.738461538461538,-0.723076923076922,-0.707692307692307,
-0.692307692307692,-0.676923076923076,-0.661538461538461,-0.646153846153846,
-0.63076923076923,-0.615384615384615,-0.6,-0.584615384615384,-0.569230769230769,
-0.553846153846154,-0.538461538461538,-0.523076923076923,-0.507692307692308,
-0.492307692307692,-0.476923076923077,-0.461538461538462,-0.446153846153846,
-0.430769230769231,-0.415384615384615,-0.4,-0.384615384615385,-0.369230769230769,
-0.353846153846154,-0.338461538461538,-0.323076923076923,-0.307692307692308,
-0.292307692307692,-0.276923076923077,-0.261538461538462,-0.246153846153846,
-0.230769230769231,-0.215384615384615,-0.2,-0.184615384615385,-0.169230769230769,
-0.153846153846154,-0.138461538461538,-0.123076923076923,-0.107692307692308,
-0.0923076923076923,-0.0769230769230769,-0.0615384615384615,-0.0461538461538462,
-0.0307692307692308,-0.0153846153846154,0.),(-1.,1.),.UNSPECIFIED.)
GEOMETRIC_REPRESENTATION_ITEM()
RATIONAL_B_SPLINE_SURFACE(((1.,1.),(1.,1.),(1.,1.),(1.,1.),(1.,1.),(1.,
1.),(1.,1.),(1.,1.),(1.,1.),(1.,1.),(1.,1.),(1.,1.),(1.,1.),(1.,1.),(1.,
1.),(1.,1.),(1.,1.),(1.,1.),(1.,1.),(1.,1.),(1.,1.),(1.,1.),(1.,1.),(1.,
1.),(1.,1.),(1.,1.),(1.,1.),(1.,1.),(1.,1.),(1.,1.),(1.,1.),(1.,1.),(1.,
1.),(1.,1.),(1.,1.),(1.,1.),(1.,1.),(1.,1.),(1.,1.),(1.,1.),(1.,1.),(1.,
1.),(1.,1.),(1.,1.),(1.,1.),(1.,1.),(1.,1.),(1.,1.),(1.,1.),(1.,1.),(1.,
1.),(1.,1.),(1.,1.),(1.,1.),(1.,1.),(1.,1.),(1.,1.),(1.,1.),(1.,1.),(1.,
1.),(1.,1.),(1.,1.),(1.,1.),(1.,1.),(1.,1.),(1.,1.),(1.,1.),(1.,1.),(1.,
1.),(1.,1.)))
REPRESENTATION_ITEM('')
SURFACE()
);
#112=(
BOUNDED_SURFACE()
B_SPLINE_SURFACE(5,1,((#58106,#58107),(#58108,#58109),(#58110,#58111),(#58112,
#58113),(#58114,#58115),(#58116,#58117),(#58118,#58119),(#58120,#58121),
(#58122,#58123),(#58124,#58125),(#58126,#58127),(#58128,#58129),(#58130,
#58131),(#58132,#58133),(#58134,#58135),(#58136,#58137),(#58138,#58139),
(#58140,#58141),(#58142,#58143),(#58144,#58145),(#58146,#58147),(#58148,
#58149),(#58150,#58151),(#58152,#58153),(#58154,#58155),(#58156,#58157),
(#58158,#58159),(#58160,#58161),(#58162,#58163),(#58164,#58165),(#58166,
#58167),(#58168,#58169),(#58170,#58171),(#58172,#58173),(#58174,#58175),
(#58176,#58177),(#58178,#58179),(#58180,#58181),(#58182,#58183),(#58184,
#58185),(#58186,#58187),(#58188,#58189),(#58190,#58191),(#58192,#58193),
(#58194,#58195),(#58196,#58197),(#58198,#58199),(#58200,#58201),(#58202,
#58203),(#58204,#58205),(#58206,#58207),(#58208,#58209),(#58210,#58211),
(#58212,#58213),(#58214,#58215),(#58216,#58217),(#58218,#58219),(#58220,
#58221),(#58222,#58223),(#58224,#58225),(#58226,#58227),(#58228,#58229),
(#58230,#58231),(#58232,#58233),(#58234,#58235),(#58236,#58237),(#58238,
#58239),(#58240,#58241),(#58242,#58243),(#58244,#58245)),.UNSPECIFIED.,
 .F.,.F.,.F.)
B_SPLINE_SURFACE_WITH_KNOTS((6,1,1,1,1,1,1,1,1,1,1,1,1,1,1,1,1,1,1,1,1,
1,1,1,1,1,1,1,1,1,1,1,1,1,1,1,1,1,1,1,1,1,1,1,1,1,1,1,1,1,1,1,1,1,1,1,1,
1,1,1,1,1,1,1,1,6),(2,2),(-1.,-0.984615384615383,-0.969230769230768,-0.953846153846152,
-0.938461538461537,-0.923076923076922,-0.907692307692306,-0.892307692307691,
-0.876923076923076,-0.86153846153846,-0.846153846153845,-0.83076923076923,
-0.815384615384614,-0.799999999999999,-0.784615384615384,-0.769230769230768,
-0.753846153846153,-0.738461538461538,-0.723076923076922,-0.707692307692307,
-0.692307692307692,-0.676923076923076,-0.661538461538461,-0.646153846153846,
-0.63076923076923,-0.615384615384615,-0.6,-0.584615384615384,-0.569230769230769,
-0.553846153846154,-0.538461538461538,-0.523076923076923,-0.507692307692308,
-0.492307692307692,-0.476923076923077,-0.461538461538462,-0.446153846153846,
-0.430769230769231,-0.415384615384615,-0.4,-0.384615384615385,-0.369230769230769,
-0.353846153846154,-0.338461538461538,-0.323076923076923,-0.307692307692308,
-0.292307692307692,-0.276923076923077,-0.261538461538462,-0.246153846153846,
-0.230769230769231,-0.215384615384615,-0.2,-0.184615384615385,-0.169230769230769,
-0.153846153846154,-0.138461538461538,-0.123076923076923,-0.107692307692308,
-0.0923076923076923,-0.0769230769230769,-0.0615384615384615,-0.0461538461538462,
-0.0307692307692308,-0.0153846153846154,0.),(-1.,1.),.UNSPECIFIED.)
GEOMETRIC_REPRESENTATION_ITEM()
RATIONAL_B_SPLINE_SURFACE(((1.,1.),(1.,1.),(1.,1.),(1.,1.),(1.,1.),(1.,
1.),(1.,1.),(1.,1.),(1.,1.),(1.,1.),(1.,1.),(1.,1.),(1.,1.),(1.,1.),(1.,
1.),(1.,1.),(1.,1.),(1.,1.),(1.,1.),(1.,1.),(1.,1.),(1.,1.),(1.,1.),(1.,
1.),(1.,1.),(1.,1.),(1.,1.),(1.,1.),(1.,1.),(1.,1.),(1.,1.),(1.,1.),(1.,
1.),(1.,1.),(1.,1.),(1.,1.),(1.,1.),(1.,1.),(1.,1.),(1.,1.),(1.,1.),(1.,
1.),(1.,1.),(1.,1.),(1.,1.),(1.,1.),(1.,1.),(1.,1.),(1.,1.),(1.,1.),(1.,
1.),(1.,1.),(1.,1.),(1.,1.),(1.,1.),(1.,1.),(1.,1.),(1.,1.),(1.,1.),(1.,
1.),(1.,1.),(1.,1.),(1.,1.),(1.,1.),(1.,1.),(1.,1.),(1.,1.),(1.,1.),(1.,
1.),(1.,1.)))
REPRESENTATION_ITEM('')
SURFACE()
);
#113=(
BOUNDED_SURFACE()
B_SPLINE_SURFACE(5,1,((#58336,#58337),(#58338,#58339),(#58340,#58341),(#58342,
#58343),(#58344,#58345),(#58346,#58347),(#58348,#58349),(#58350,#58351),
(#58352,#58353),(#58354,#58355),(#58356,#58357),(#58358,#58359),(#58360,
#58361),(#58362,#58363),(#58364,#58365),(#58366,#58367),(#58368,#58369),
(#58370,#58371),(#58372,#58373),(#58374,#58375),(#58376,#58377),(#58378,
#58379),(#58380,#58381),(#58382,#58383),(#58384,#58385),(#58386,#58387),
(#58388,#58389),(#58390,#58391),(#58392,#58393),(#58394,#58395),(#58396,
#58397),(#58398,#58399),(#58400,#58401),(#58402,#58403),(#58404,#58405),
(#58406,#58407),(#58408,#58409),(#58410,#58411),(#58412,#58413),(#58414,
#58415),(#58416,#58417),(#58418,#58419),(#58420,#58421),(#58422,#58423),
(#58424,#58425),(#58426,#58427),(#58428,#58429),(#58430,#58431),(#58432,
#58433),(#58434,#58435),(#58436,#58437),(#58438,#58439),(#58440,#58441),
(#58442,#58443),(#58444,#58445),(#58446,#58447),(#58448,#58449),(#58450,
#58451),(#58452,#58453),(#58454,#58455),(#58456,#58457),(#58458,#58459),
(#58460,#58461),(#58462,#58463),(#58464,#58465),(#58466,#58467),(#58468,
#58469),(#58470,#58471),(#58472,#58473),(#58474,#58475)),.UNSPECIFIED.,
 .F.,.F.,.F.)
B_SPLINE_SURFACE_WITH_KNOTS((6,1,1,1,1,1,1,1,1,1,1,1,1,1,1,1,1,1,1,1,1,
1,1,1,1,1,1,1,1,1,1,1,1,1,1,1,1,1,1,1,1,1,1,1,1,1,1,1,1,1,1,1,1,1,1,1,1,
1,1,1,1,1,1,1,1,6),(2,2),(-1.,-0.984615384615383,-0.969230769230768,-0.953846153846152,
-0.938461538461537,-0.923076923076922,-0.907692307692306,-0.892307692307691,
-0.876923076923076,-0.86153846153846,-0.846153846153845,-0.83076923076923,
-0.815384615384614,-0.799999999999999,-0.784615384615384,-0.769230769230768,
-0.753846153846153,-0.738461538461538,-0.723076923076922,-0.707692307692307,
-0.692307692307692,-0.676923076923076,-0.661538461538461,-0.646153846153846,
-0.63076923076923,-0.615384615384615,-0.6,-0.584615384615384,-0.569230769230769,
-0.553846153846154,-0.538461538461538,-0.523076923076923,-0.507692307692308,
-0.492307692307692,-0.476923076923077,-0.461538461538462,-0.446153846153846,
-0.430769230769231,-0.415384615384615,-0.4,-0.384615384615385,-0.369230769230769,
-0.353846153846154,-0.338461538461538,-0.323076923076923,-0.307692307692308,
-0.292307692307692,-0.276923076923077,-0.261538461538462,-0.246153846153846,
-0.230769230769231,-0.215384615384615,-0.2,-0.184615384615385,-0.169230769230769,
-0.153846153846154,-0.138461538461538,-0.123076923076923,-0.107692307692308,
-0.0923076923076923,-0.0769230769230769,-0.0615384615384615,-0.0461538461538462,
-0.0307692307692308,-0.0153846153846154,0.),(-1.,1.),.UNSPECIFIED.)
GEOMETRIC_REPRESENTATION_ITEM()
RATIONAL_B_SPLINE_SURFACE(((1.,1.),(1.,1.),(1.,1.),(1.,1.),(1.,1.),(1.,
1.),(1.,1.),(1.,1.),(1.,1.),(1.,1.),(1.,1.),(1.,1.),(1.,1.),(1.,1.),(1.,
1.),(1.,1.),(1.,1.),(1.,1.),(1.,1.),(1.,1.),(1.,1.),(1.,1.),(1.,1.),(1.,
1.),(1.,1.),(1.,1.),(1.,1.),(1.,1.),(1.,1.),(1.,1.),(1.,1.),(1.,1.),(1.,
1.),(1.,1.),(1.,1.),(1.,1.),(1.,1.),(1.,1.),(1.,1.),(1.,1.),(1.,1.),(1.,
1.),(1.,1.),(1.,1.),(1.,1.),(1.,1.),(1.,1.),(1.,1.),(1.,1.),(1.,1.),(1.,
1.),(1.,1.),(1.,1.),(1.,1.),(1.,1.),(1.,1.),(1.,1.),(1.,1.),(1.,1.),(1.,
1.),(1.,1.),(1.,1.),(1.,1.),(1.,1.),(1.,1.),(1.,1.),(1.,1.),(1.,1.),(1.,
1.),(1.,1.)))
REPRESENTATION_ITEM('')
SURFACE()
);
#114=(
BOUNDED_SURFACE()
B_SPLINE_SURFACE(5,1,((#58548,#58549),(#58550,#58551),(#58552,#58553),(#58554,
#58555),(#58556,#58557),(#58558,#58559),(#58560,#58561),(#58562,#58563),
(#58564,#58565),(#58566,#58567),(#58568,#58569),(#58570,#58571),(#58572,
#58573),(#58574,#58575),(#58576,#58577),(#58578,#58579),(#58580,#58581),
(#58582,#58583),(#58584,#58585),(#58586,#58587),(#58588,#58589),(#58590,
#58591),(#58592,#58593),(#58594,#58595),(#58596,#58597),(#58598,#58599),
(#58600,#58601),(#58602,#58603),(#58604,#58605),(#58606,#58607),(#58608,
#58609),(#58610,#58611),(#58612,#58613),(#58614,#58615),(#58616,#58617),
(#58618,#58619),(#58620,#58621),(#58622,#58623),(#58624,#58625),(#58626,
#58627),(#58628,#58629),(#58630,#58631),(#58632,#58633),(#58634,#58635),
(#58636,#58637),(#58638,#58639),(#58640,#58641),(#58642,#58643),(#58644,
#58645),(#58646,#58647),(#58648,#58649),(#58650,#58651),(#58652,#58653),
(#58654,#58655),(#58656,#58657),(#58658,#58659),(#58660,#58661),(#58662,
#58663),(#58664,#58665),(#58666,#58667),(#58668,#58669),(#58670,#58671),
(#58672,#58673),(#58674,#58675),(#58676,#58677),(#58678,#58679),(#58680,
#58681),(#58682,#58683),(#58684,#58685),(#58686,#58687)),.UNSPECIFIED.,
 .F.,.F.,.F.)
B_SPLINE_SURFACE_WITH_KNOTS((6,1,1,1,1,1,1,1,1,1,1,1,1,1,1,1,1,1,1,1,1,
1,1,1,1,1,1,1,1,1,1,1,1,1,1,1,1,1,1,1,1,1,1,1,1,1,1,1,1,1,1,1,1,1,1,1,1,
1,1,1,1,1,1,1,1,6),(2,2),(-1.,-0.984615384615383,-0.969230769230768,-0.953846153846152,
-0.938461538461537,-0.923076923076922,-0.907692307692306,-0.892307692307691,
-0.876923076923076,-0.86153846153846,-0.846153846153845,-0.83076923076923,
-0.815384615384614,-0.799999999999999,-0.784615384615384,-0.769230769230768,
-0.753846153846153,-0.738461538461538,-0.723076923076922,-0.707692307692307,
-0.692307692307692,-0.676923076923076,-0.661538461538461,-0.646153846153846,
-0.63076923076923,-0.615384615384615,-0.6,-0.584615384615384,-0.569230769230769,
-0.553846153846154,-0.538461538461538,-0.523076923076923,-0.507692307692308,
-0.492307692307692,-0.476923076923077,-0.461538461538462,-0.446153846153846,
-0.430769230769231,-0.415384615384615,-0.4,-0.384615384615385,-0.369230769230769,
-0.353846153846154,-0.338461538461538,-0.323076923076923,-0.307692307692308,
-0.292307692307692,-0.276923076923077,-0.261538461538462,-0.246153846153846,
-0.230769230769231,-0.215384615384615,-0.2,-0.184615384615385,-0.169230769230769,
-0.153846153846154,-0.138461538461538,-0.123076923076923,-0.107692307692308,
-0.0923076923076923,-0.0769230769230769,-0.0615384615384615,-0.0461538461538462,
-0.0307692307692308,-0.0153846153846154,0.),(-1.,1.),.UNSPECIFIED.)
GEOMETRIC_REPRESENTATION_ITEM()
RATIONAL_B_SPLINE_SURFACE(((1.,1.),(1.,1.),(1.,1.),(1.,1.),(1.,1.),(1.,
1.),(1.,1.),(1.,1.),(1.,1.),(1.,1.),(1.,1.),(1.,1.),(1.,1.),(1.,1.),(1.,
1.),(1.,1.),(1.,1.),(1.,1.),(1.,1.),(1.,1.),(1.,1.),(1.,1.),(1.,1.),(1.,
1.),(1.,1.),(1.,1.),(1.,1.),(1.,1.),(1.,1.),(1.,1.),(1.,1.),(1.,1.),(1.,
1.),(1.,1.),(1.,1.),(1.,1.),(1.,1.),(1.,1.),(1.,1.),(1.,1.),(1.,1.),(1.,
1.),(1.,1.),(1.,1.),(1.,1.),(1.,1.),(1.,1.),(1.,1.),(1.,1.),(1.,1.),(1.,
1.),(1.,1.),(1.,1.),(1.,1.),(1.,1.),(1.,1.),(1.,1.),(1.,1.),(1.,1.),(1.,
1.),(1.,1.),(1.,1.),(1.,1.),(1.,1.),(1.,1.),(1.,1.),(1.,1.),(1.,1.),(1.,
1.),(1.,1.)))
REPRESENTATION_ITEM('')
SURFACE()
);
#115=(
BOUNDED_SURFACE()
B_SPLINE_SURFACE(5,1,((#58778,#58779),(#58780,#58781),(#58782,#58783),(#58784,
#58785),(#58786,#58787),(#58788,#58789),(#58790,#58791),(#58792,#58793),
(#58794,#58795),(#58796,#58797),(#58798,#58799),(#58800,#58801),(#58802,
#58803),(#58804,#58805),(#58806,#58807),(#58808,#58809),(#58810,#58811),
(#58812,#58813),(#58814,#58815),(#58816,#58817),(#58818,#58819),(#58820,
#58821),(#58822,#58823),(#58824,#58825),(#58826,#58827),(#58828,#58829),
(#58830,#58831),(#58832,#58833),(#58834,#58835),(#58836,#58837),(#58838,
#58839),(#58840,#58841),(#58842,#58843),(#58844,#58845),(#58846,#58847),
(#58848,#58849),(#58850,#58851),(#58852,#58853),(#58854,#58855),(#58856,
#58857),(#58858,#58859),(#58860,#58861),(#58862,#58863),(#58864,#58865),
(#58866,#58867),(#58868,#58869),(#58870,#58871),(#58872,#58873),(#58874,
#58875),(#58876,#58877),(#58878,#58879),(#58880,#58881),(#58882,#58883),
(#58884,#58885),(#58886,#58887),(#58888,#58889),(#58890,#58891),(#58892,
#58893),(#58894,#58895),(#58896,#58897),(#58898,#58899),(#58900,#58901),
(#58902,#58903),(#58904,#58905),(#58906,#58907),(#58908,#58909),(#58910,
#58911),(#58912,#58913),(#58914,#58915),(#58916,#58917)),.UNSPECIFIED.,
 .F.,.F.,.F.)
B_SPLINE_SURFACE_WITH_KNOTS((6,1,1,1,1,1,1,1,1,1,1,1,1,1,1,1,1,1,1,1,1,
1,1,1,1,1,1,1,1,1,1,1,1,1,1,1,1,1,1,1,1,1,1,1,1,1,1,1,1,1,1,1,1,1,1,1,1,
1,1,1,1,1,1,1,1,6),(2,2),(-1.,-0.984615384615383,-0.969230769230768,-0.953846153846152,
-0.938461538461537,-0.923076923076922,-0.907692307692306,-0.892307692307691,
-0.876923076923076,-0.86153846153846,-0.846153846153845,-0.83076923076923,
-0.815384615384614,-0.799999999999999,-0.784615384615384,-0.769230769230768,
-0.753846153846153,-0.738461538461538,-0.723076923076922,-0.707692307692307,
-0.692307692307692,-0.676923076923076,-0.661538461538461,-0.646153846153846,
-0.63076923076923,-0.615384615384615,-0.6,-0.584615384615384,-0.569230769230769,
-0.553846153846154,-0.538461538461538,-0.523076923076923,-0.507692307692308,
-0.492307692307692,-0.476923076923077,-0.461538461538462,-0.446153846153846,
-0.430769230769231,-0.415384615384615,-0.4,-0.384615384615385,-0.369230769230769,
-0.353846153846154,-0.338461538461538,-0.323076923076923,-0.307692307692308,
-0.292307692307692,-0.276923076923077,-0.261538461538462,-0.246153846153846,
-0.230769230769231,-0.215384615384615,-0.2,-0.184615384615385,-0.169230769230769,
-0.153846153846154,-0.138461538461538,-0.123076923076923,-0.107692307692308,
-0.0923076923076923,-0.0769230769230769,-0.0615384615384615,-0.0461538461538462,
-0.0307692307692308,-0.0153846153846154,0.),(-1.,1.),.UNSPECIFIED.)
GEOMETRIC_REPRESENTATION_ITEM()
RATIONAL_B_SPLINE_SURFACE(((1.,1.),(1.,1.),(1.,1.),(1.,1.),(1.,1.),(1.,
1.),(1.,1.),(1.,1.),(1.,1.),(1.,1.),(1.,1.),(1.,1.),(1.,1.),(1.,1.),(1.,
1.),(1.,1.),(1.,1.),(1.,1.),(1.,1.),(1.,1.),(1.,1.),(1.,1.),(1.,1.),(1.,
1.),(1.,1.),(1.,1.),(1.,1.),(1.,1.),(1.,1.),(1.,1.),(1.,1.),(1.,1.),(1.,
1.),(1.,1.),(1.,1.),(1.,1.),(1.,1.),(1.,1.),(1.,1.),(1.,1.),(1.,1.),(1.,
1.),(1.,1.),(1.,1.),(1.,1.),(1.,1.),(1.,1.),(1.,1.),(1.,1.),(1.,1.),(1.,
1.),(1.,1.),(1.,1.),(1.,1.),(1.,1.),(1.,1.),(1.,1.),(1.,1.),(1.,1.),(1.,
1.),(1.,1.),(1.,1.),(1.,1.),(1.,1.),(1.,1.),(1.,1.),(1.,1.),(1.,1.),(1.,
1.),(1.,1.)))
REPRESENTATION_ITEM('')
SURFACE()
);
#116=(
BOUNDED_SURFACE()
B_SPLINE_SURFACE(5,1,((#58990,#58991),(#58992,#58993),(#58994,#58995),(#58996,
#58997),(#58998,#58999),(#59000,#59001),(#59002,#59003),(#59004,#59005),
(#59006,#59007),(#59008,#59009),(#59010,#59011),(#59012,#59013),(#59014,
#59015),(#59016,#59017),(#59018,#59019),(#59020,#59021),(#59022,#59023),
(#59024,#59025),(#59026,#59027),(#59028,#59029),(#59030,#59031),(#59032,
#59033),(#59034,#59035),(#59036,#59037),(#59038,#59039),(#59040,#59041),
(#59042,#59043),(#59044,#59045),(#59046,#59047),(#59048,#59049),(#59050,
#59051),(#59052,#59053),(#59054,#59055),(#59056,#59057),(#59058,#59059),
(#59060,#59061),(#59062,#59063),(#59064,#59065),(#59066,#59067),(#59068,
#59069),(#59070,#59071),(#59072,#59073),(#59074,#59075),(#59076,#59077),
(#59078,#59079),(#59080,#59081),(#59082,#59083),(#59084,#59085),(#59086,
#59087),(#59088,#59089),(#59090,#59091),(#59092,#59093),(#59094,#59095),
(#59096,#59097),(#59098,#59099),(#59100,#59101),(#59102,#59103),(#59104,
#59105),(#59106,#59107),(#59108,#59109),(#59110,#59111),(#59112,#59113),
(#59114,#59115),(#59116,#59117),(#59118,#59119),(#59120,#59121),(#59122,
#59123),(#59124,#59125),(#59126,#59127),(#59128,#59129)),.UNSPECIFIED.,
 .F.,.F.,.F.)
B_SPLINE_SURFACE_WITH_KNOTS((6,1,1,1,1,1,1,1,1,1,1,1,1,1,1,1,1,1,1,1,1,
1,1,1,1,1,1,1,1,1,1,1,1,1,1,1,1,1,1,1,1,1,1,1,1,1,1,1,1,1,1,1,1,1,1,1,1,
1,1,1,1,1,1,1,1,6),(2,2),(-1.,-0.984615384615383,-0.969230769230768,-0.953846153846152,
-0.938461538461537,-0.923076923076922,-0.907692307692306,-0.892307692307691,
-0.876923076923076,-0.86153846153846,-0.846153846153845,-0.83076923076923,
-0.815384615384614,-0.799999999999999,-0.784615384615384,-0.769230769230768,
-0.753846153846153,-0.738461538461538,-0.723076923076922,-0.707692307692307,
-0.692307692307692,-0.676923076923076,-0.661538461538461,-0.646153846153846,
-0.63076923076923,-0.615384615384615,-0.6,-0.584615384615384,-0.569230769230769,
-0.553846153846154,-0.538461538461538,-0.523076923076923,-0.507692307692308,
-0.492307692307692,-0.476923076923077,-0.461538461538462,-0.446153846153846,
-0.430769230769231,-0.415384615384615,-0.4,-0.384615384615385,-0.369230769230769,
-0.353846153846154,-0.338461538461538,-0.323076923076923,-0.307692307692308,
-0.292307692307692,-0.276923076923077,-0.261538461538462,-0.246153846153846,
-0.230769230769231,-0.215384615384615,-0.2,-0.184615384615385,-0.169230769230769,
-0.153846153846154,-0.138461538461538,-0.123076923076923,-0.107692307692308,
-0.0923076923076923,-0.0769230769230769,-0.0615384615384615,-0.0461538461538462,
-0.0307692307692308,-0.0153846153846154,0.),(-1.,1.),.UNSPECIFIED.)
GEOMETRIC_REPRESENTATION_ITEM()
RATIONAL_B_SPLINE_SURFACE(((1.,1.),(1.,1.),(1.,1.),(1.,1.),(1.,1.),(1.,
1.),(1.,1.),(1.,1.),(1.,1.),(1.,1.),(1.,1.),(1.,1.),(1.,1.),(1.,1.),(1.,
1.),(1.,1.),(1.,1.),(1.,1.),(1.,1.),(1.,1.),(1.,1.),(1.,1.),(1.,1.),(1.,
1.),(1.,1.),(1.,1.),(1.,1.),(1.,1.),(1.,1.),(1.,1.),(1.,1.),(1.,1.),(1.,
1.),(1.,1.),(1.,1.),(1.,1.),(1.,1.),(1.,1.),(1.,1.),(1.,1.),(1.,1.),(1.,
1.),(1.,1.),(1.,1.),(1.,1.),(1.,1.),(1.,1.),(1.,1.),(1.,1.),(1.,1.),(1.,
1.),(1.,1.),(1.,1.),(1.,1.),(1.,1.),(1.,1.),(1.,1.),(1.,1.),(1.,1.),(1.,
1.),(1.,1.),(1.,1.),(1.,1.),(1.,1.),(1.,1.),(1.,1.),(1.,1.),(1.,1.),(1.,
1.),(1.,1.)))
REPRESENTATION_ITEM('')
SURFACE()
);
#117=(
BOUNDED_SURFACE()
B_SPLINE_SURFACE(5,1,((#59220,#59221),(#59222,#59223),(#59224,#59225),(#59226,
#59227),(#59228,#59229),(#59230,#59231),(#59232,#59233),(#59234,#59235),
(#59236,#59237),(#59238,#59239),(#59240,#59241),(#59242,#59243),(#59244,
#59245),(#59246,#59247),(#59248,#59249),(#59250,#59251),(#59252,#59253),
(#59254,#59255),(#59256,#59257),(#59258,#59259),(#59260,#59261),(#59262,
#59263),(#59264,#59265),(#59266,#59267),(#59268,#59269),(#59270,#59271),
(#59272,#59273),(#59274,#59275),(#59276,#59277),(#59278,#59279),(#59280,
#59281),(#59282,#59283),(#59284,#59285),(#59286,#59287),(#59288,#59289),
(#59290,#59291),(#59292,#59293),(#59294,#59295),(#59296,#59297),(#59298,
#59299),(#59300,#59301),(#59302,#59303),(#59304,#59305),(#59306,#59307),
(#59308,#59309),(#59310,#59311),(#59312,#59313),(#59314,#59315),(#59316,
#59317),(#59318,#59319),(#59320,#59321),(#59322,#59323),(#59324,#59325),
(#59326,#59327),(#59328,#59329),(#59330,#59331),(#59332,#59333),(#59334,
#59335),(#59336,#59337),(#59338,#59339),(#59340,#59341),(#59342,#59343),
(#59344,#59345),(#59346,#59347),(#59348,#59349),(#59350,#59351),(#59352,
#59353),(#59354,#59355),(#59356,#59357),(#59358,#59359)),.UNSPECIFIED.,
 .F.,.F.,.F.)
B_SPLINE_SURFACE_WITH_KNOTS((6,1,1,1,1,1,1,1,1,1,1,1,1,1,1,1,1,1,1,1,1,
1,1,1,1,1,1,1,1,1,1,1,1,1,1,1,1,1,1,1,1,1,1,1,1,1,1,1,1,1,1,1,1,1,1,1,1,
1,1,1,1,1,1,1,1,6),(2,2),(-1.,-0.984615384615383,-0.969230769230768,-0.953846153846152,
-0.938461538461537,-0.923076923076922,-0.907692307692306,-0.892307692307691,
-0.876923076923076,-0.86153846153846,-0.846153846153845,-0.83076923076923,
-0.815384615384614,-0.799999999999999,-0.784615384615384,-0.769230769230768,
-0.753846153846153,-0.738461538461538,-0.723076923076922,-0.707692307692307,
-0.692307692307692,-0.676923076923076,-0.661538461538461,-0.646153846153846,
-0.63076923076923,-0.615384615384615,-0.6,-0.584615384615384,-0.569230769230769,
-0.553846153846154,-0.538461538461538,-0.523076923076923,-0.507692307692308,
-0.492307692307692,-0.476923076923077,-0.461538461538462,-0.446153846153846,
-0.430769230769231,-0.415384615384615,-0.4,-0.384615384615385,-0.369230769230769,
-0.353846153846154,-0.338461538461538,-0.323076923076923,-0.307692307692308,
-0.292307692307692,-0.276923076923077,-0.261538461538462,-0.246153846153846,
-0.230769230769231,-0.215384615384615,-0.2,-0.184615384615385,-0.169230769230769,
-0.153846153846154,-0.138461538461538,-0.123076923076923,-0.107692307692308,
-0.0923076923076923,-0.0769230769230769,-0.0615384615384615,-0.0461538461538462,
-0.0307692307692308,-0.0153846153846154,0.),(-1.,1.),.UNSPECIFIED.)
GEOMETRIC_REPRESENTATION_ITEM()
RATIONAL_B_SPLINE_SURFACE(((1.,1.),(1.,1.),(1.,1.),(1.,1.),(1.,1.),(1.,
1.),(1.,1.),(1.,1.),(1.,1.),(1.,1.),(1.,1.),(1.,1.),(1.,1.),(1.,1.),(1.,
1.),(1.,1.),(1.,1.),(1.,1.),(1.,1.),(1.,1.),(1.,1.),(1.,1.),(1.,1.),(1.,
1.),(1.,1.),(1.,1.),(1.,1.),(1.,1.),(1.,1.),(1.,1.),(1.,1.),(1.,1.),(1.,
1.),(1.,1.),(1.,1.),(1.,1.),(1.,1.),(1.,1.),(1.,1.),(1.,1.),(1.,1.),(1.,
1.),(1.,1.),(1.,1.),(1.,1.),(1.,1.),(1.,1.),(1.,1.),(1.,1.),(1.,1.),(1.,
1.),(1.,1.),(1.,1.),(1.,1.),(1.,1.),(1.,1.),(1.,1.),(1.,1.),(1.,1.),(1.,
1.),(1.,1.),(1.,1.),(1.,1.),(1.,1.),(1.,1.),(1.,1.),(1.,1.),(1.,1.),(1.,
1.),(1.,1.)))
REPRESENTATION_ITEM('')
SURFACE()
);
#118=(
BOUNDED_SURFACE()
B_SPLINE_SURFACE(5,1,((#59432,#59433),(#59434,#59435),(#59436,#59437),(#59438,
#59439),(#59440,#59441),(#59442,#59443),(#59444,#59445),(#59446,#59447),
(#59448,#59449),(#59450,#59451),(#59452,#59453),(#59454,#59455),(#59456,
#59457),(#59458,#59459),(#59460,#59461),(#59462,#59463),(#59464,#59465),
(#59466,#59467),(#59468,#59469),(#59470,#59471),(#59472,#59473),(#59474,
#59475),(#59476,#59477),(#59478,#59479),(#59480,#59481),(#59482,#59483),
(#59484,#59485),(#59486,#59487),(#59488,#59489),(#59490,#59491),(#59492,
#59493),(#59494,#59495),(#59496,#59497),(#59498,#59499),(#59500,#59501),
(#59502,#59503),(#59504,#59505),(#59506,#59507),(#59508,#59509),(#59510,
#59511),(#59512,#59513),(#59514,#59515),(#59516,#59517),(#59518,#59519),
(#59520,#59521),(#59522,#59523),(#59524,#59525),(#59526,#59527),(#59528,
#59529),(#59530,#59531),(#59532,#59533),(#59534,#59535),(#59536,#59537),
(#59538,#59539),(#59540,#59541),(#59542,#59543),(#59544,#59545),(#59546,
#59547),(#59548,#59549),(#59550,#59551),(#59552,#59553),(#59554,#59555),
(#59556,#59557),(#59558,#59559),(#59560,#59561),(#59562,#59563),(#59564,
#59565),(#59566,#59567),(#59568,#59569),(#59570,#59571)),.UNSPECIFIED.,
 .F.,.F.,.F.)
B_SPLINE_SURFACE_WITH_KNOTS((6,1,1,1,1,1,1,1,1,1,1,1,1,1,1,1,1,1,1,1,1,
1,1,1,1,1,1,1,1,1,1,1,1,1,1,1,1,1,1,1,1,1,1,1,1,1,1,1,1,1,1,1,1,1,1,1,1,
1,1,1,1,1,1,1,1,6),(2,2),(-1.,-0.984615384615383,-0.969230769230768,-0.953846153846152,
-0.938461538461537,-0.923076923076922,-0.907692307692306,-0.892307692307691,
-0.876923076923076,-0.86153846153846,-0.846153846153845,-0.83076923076923,
-0.815384615384614,-0.799999999999999,-0.784615384615384,-0.769230769230768,
-0.753846153846153,-0.738461538461538,-0.723076923076922,-0.707692307692307,
-0.692307692307692,-0.676923076923076,-0.661538461538461,-0.646153846153846,
-0.63076923076923,-0.615384615384615,-0.6,-0.584615384615384,-0.569230769230769,
-0.553846153846154,-0.538461538461538,-0.523076923076923,-0.507692307692308,
-0.492307692307692,-0.476923076923077,-0.461538461538462,-0.446153846153846,
-0.430769230769231,-0.415384615384615,-0.4,-0.384615384615385,-0.369230769230769,
-0.353846153846154,-0.338461538461538,-0.323076923076923,-0.307692307692308,
-0.292307692307692,-0.276923076923077,-0.261538461538462,-0.246153846153846,
-0.230769230769231,-0.215384615384615,-0.2,-0.184615384615385,-0.169230769230769,
-0.153846153846154,-0.138461538461538,-0.123076923076923,-0.107692307692308,
-0.0923076923076923,-0.0769230769230769,-0.0615384615384615,-0.0461538461538462,
-0.0307692307692308,-0.0153846153846154,0.),(-1.,1.),.UNSPECIFIED.)
GEOMETRIC_REPRESENTATION_ITEM()
RATIONAL_B_SPLINE_SURFACE(((1.,1.),(1.,1.),(1.,1.),(1.,1.),(1.,1.),(1.,
1.),(1.,1.),(1.,1.),(1.,1.),(1.,1.),(1.,1.),(1.,1.),(1.,1.),(1.,1.),(1.,
1.),(1.,1.),(1.,1.),(1.,1.),(1.,1.),(1.,1.),(1.,1.),(1.,1.),(1.,1.),(1.,
1.),(1.,1.),(1.,1.),(1.,1.),(1.,1.),(1.,1.),(1.,1.),(1.,1.),(1.,1.),(1.,
1.),(1.,1.),(1.,1.),(1.,1.),(1.,1.),(1.,1.),(1.,1.),(1.,1.),(1.,1.),(1.,
1.),(1.,1.),(1.,1.),(1.,1.),(1.,1.),(1.,1.),(1.,1.),(1.,1.),(1.,1.),(1.,
1.),(1.,1.),(1.,1.),(1.,1.),(1.,1.),(1.,1.),(1.,1.),(1.,1.),(1.,1.),(1.,
1.),(1.,1.),(1.,1.),(1.,1.),(1.,1.),(1.,1.),(1.,1.),(1.,1.),(1.,1.),(1.,
1.),(1.,1.)))
REPRESENTATION_ITEM('')
SURFACE()
);
#119=(
BOUNDED_SURFACE()
B_SPLINE_SURFACE(5,1,((#59662,#59663),(#59664,#59665),(#59666,#59667),(#59668,
#59669),(#59670,#59671),(#59672,#59673),(#59674,#59675),(#59676,#59677),
(#59678,#59679),(#59680,#59681),(#59682,#59683),(#59684,#59685),(#59686,
#59687),(#59688,#59689),(#59690,#59691),(#59692,#59693),(#59694,#59695),
(#59696,#59697),(#59698,#59699),(#59700,#59701),(#59702,#59703),(#59704,
#59705),(#59706,#59707),(#59708,#59709),(#59710,#59711),(#59712,#59713),
(#59714,#59715),(#59716,#59717),(#59718,#59719),(#59720,#59721),(#59722,
#59723),(#59724,#59725),(#59726,#59727),(#59728,#59729),(#59730,#59731),
(#59732,#59733),(#59734,#59735),(#59736,#59737),(#59738,#59739),(#59740,
#59741),(#59742,#59743),(#59744,#59745),(#59746,#59747),(#59748,#59749),
(#59750,#59751),(#59752,#59753),(#59754,#59755),(#59756,#59757),(#59758,
#59759),(#59760,#59761),(#59762,#59763),(#59764,#59765),(#59766,#59767),
(#59768,#59769),(#59770,#59771),(#59772,#59773),(#59774,#59775),(#59776,
#59777),(#59778,#59779),(#59780,#59781),(#59782,#59783),(#59784,#59785),
(#59786,#59787),(#59788,#59789),(#59790,#59791),(#59792,#59793),(#59794,
#59795),(#59796,#59797),(#59798,#59799),(#59800,#59801)),.UNSPECIFIED.,
 .F.,.F.,.F.)
B_SPLINE_SURFACE_WITH_KNOTS((6,1,1,1,1,1,1,1,1,1,1,1,1,1,1,1,1,1,1,1,1,
1,1,1,1,1,1,1,1,1,1,1,1,1,1,1,1,1,1,1,1,1,1,1,1,1,1,1,1,1,1,1,1,1,1,1,1,
1,1,1,1,1,1,1,1,6),(2,2),(-1.,-0.984615384615383,-0.969230769230768,-0.953846153846152,
-0.938461538461537,-0.923076923076922,-0.907692307692306,-0.892307692307691,
-0.876923076923076,-0.86153846153846,-0.846153846153845,-0.83076923076923,
-0.815384615384614,-0.799999999999999,-0.784615384615384,-0.769230769230768,
-0.753846153846153,-0.738461538461538,-0.723076923076922,-0.707692307692307,
-0.692307692307692,-0.676923076923076,-0.661538461538461,-0.646153846153846,
-0.63076923076923,-0.615384615384615,-0.6,-0.584615384615384,-0.569230769230769,
-0.553846153846154,-0.538461538461538,-0.523076923076923,-0.507692307692308,
-0.492307692307692,-0.476923076923077,-0.461538461538462,-0.446153846153846,
-0.430769230769231,-0.415384615384615,-0.4,-0.384615384615385,-0.369230769230769,
-0.353846153846154,-0.338461538461538,-0.323076923076923,-0.307692307692308,
-0.292307692307692,-0.276923076923077,-0.261538461538462,-0.246153846153846,
-0.230769230769231,-0.215384615384615,-0.2,-0.184615384615385,-0.169230769230769,
-0.153846153846154,-0.138461538461538,-0.123076923076923,-0.107692307692308,
-0.0923076923076923,-0.0769230769230769,-0.0615384615384615,-0.0461538461538462,
-0.0307692307692308,-0.0153846153846154,0.),(-1.,1.),.UNSPECIFIED.)
GEOMETRIC_REPRESENTATION_ITEM()
RATIONAL_B_SPLINE_SURFACE(((1.,1.),(1.,1.),(1.,1.),(1.,1.),(1.,1.),(1.,
1.),(1.,1.),(1.,1.),(1.,1.),(1.,1.),(1.,1.),(1.,1.),(1.,1.),(1.,1.),(1.,
1.),(1.,1.),(1.,1.),(1.,1.),(1.,1.),(1.,1.),(1.,1.),(1.,1.),(1.,1.),(1.,
1.),(1.,1.),(1.,1.),(1.,1.),(1.,1.),(1.,1.),(1.,1.),(1.,1.),(1.,1.),(1.,
1.),(1.,1.),(1.,1.),(1.,1.),(1.,1.),(1.,1.),(1.,1.),(1.,1.),(1.,1.),(1.,
1.),(1.,1.),(1.,1.),(1.,1.),(1.,1.),(1.,1.),(1.,1.),(1.,1.),(1.,1.),(1.,
1.),(1.,1.),(1.,1.),(1.,1.),(1.,1.),(1.,1.),(1.,1.),(1.,1.),(1.,1.),(1.,
1.),(1.,1.),(1.,1.),(1.,1.),(1.,1.),(1.,1.),(1.,1.),(1.,1.),(1.,1.),(1.,
1.),(1.,1.)))
REPRESENTATION_ITEM('')
SURFACE()
);
#120=(
BOUNDED_SURFACE()
B_SPLINE_SURFACE(5,1,((#59874,#59875),(#59876,#59877),(#59878,#59879),(#59880,
#59881),(#59882,#59883),(#59884,#59885),(#59886,#59887),(#59888,#59889),
(#59890,#59891),(#59892,#59893),(#59894,#59895),(#59896,#59897),(#59898,
#59899),(#59900,#59901),(#59902,#59903),(#59904,#59905),(#59906,#59907),
(#59908,#59909),(#59910,#59911),(#59912,#59913),(#59914,#59915),(#59916,
#59917),(#59918,#59919),(#59920,#59921),(#59922,#59923),(#59924,#59925),
(#59926,#59927),(#59928,#59929),(#59930,#59931),(#59932,#59933),(#59934,
#59935),(#59936,#59937),(#59938,#59939),(#59940,#59941),(#59942,#59943),
(#59944,#59945),(#59946,#59947),(#59948,#59949),(#59950,#59951),(#59952,
#59953),(#59954,#59955),(#59956,#59957),(#59958,#59959),(#59960,#59961),
(#59962,#59963),(#59964,#59965),(#59966,#59967),(#59968,#59969),(#59970,
#59971),(#59972,#59973),(#59974,#59975),(#59976,#59977),(#59978,#59979),
(#59980,#59981),(#59982,#59983),(#59984,#59985),(#59986,#59987),(#59988,
#59989),(#59990,#59991),(#59992,#59993),(#59994,#59995),(#59996,#59997),
(#59998,#59999),(#60000,#60001),(#60002,#60003),(#60004,#60005),(#60006,
#60007),(#60008,#60009),(#60010,#60011),(#60012,#60013)),.UNSPECIFIED.,
 .F.,.F.,.F.)
B_SPLINE_SURFACE_WITH_KNOTS((6,1,1,1,1,1,1,1,1,1,1,1,1,1,1,1,1,1,1,1,1,
1,1,1,1,1,1,1,1,1,1,1,1,1,1,1,1,1,1,1,1,1,1,1,1,1,1,1,1,1,1,1,1,1,1,1,1,
1,1,1,1,1,1,1,1,6),(2,2),(-1.,-0.984615384615383,-0.969230769230768,-0.953846153846152,
-0.938461538461537,-0.923076923076922,-0.907692307692306,-0.892307692307691,
-0.876923076923076,-0.86153846153846,-0.846153846153845,-0.83076923076923,
-0.815384615384614,-0.799999999999999,-0.784615384615384,-0.769230769230768,
-0.753846153846153,-0.738461538461538,-0.723076923076922,-0.707692307692307,
-0.692307692307692,-0.676923076923076,-0.661538461538461,-0.646153846153846,
-0.63076923076923,-0.615384615384615,-0.6,-0.584615384615384,-0.569230769230769,
-0.553846153846154,-0.538461538461538,-0.523076923076923,-0.507692307692308,
-0.492307692307692,-0.476923076923077,-0.461538461538462,-0.446153846153846,
-0.430769230769231,-0.415384615384615,-0.4,-0.384615384615385,-0.369230769230769,
-0.353846153846154,-0.338461538461538,-0.323076923076923,-0.307692307692308,
-0.292307692307692,-0.276923076923077,-0.261538461538462,-0.246153846153846,
-0.230769230769231,-0.215384615384615,-0.2,-0.184615384615385,-0.169230769230769,
-0.153846153846154,-0.138461538461538,-0.123076923076923,-0.107692307692308,
-0.0923076923076923,-0.0769230769230769,-0.0615384615384615,-0.0461538461538462,
-0.0307692307692308,-0.0153846153846154,0.),(-1.,1.),.UNSPECIFIED.)
GEOMETRIC_REPRESENTATION_ITEM()
RATIONAL_B_SPLINE_SURFACE(((1.,1.),(1.,1.),(1.,1.),(1.,1.),(1.,1.),(1.,
1.),(1.,1.),(1.,1.),(1.,1.),(1.,1.),(1.,1.),(1.,1.),(1.,1.),(1.,1.),(1.,
1.),(1.,1.),(1.,1.),(1.,1.),(1.,1.),(1.,1.),(1.,1.),(1.,1.),(1.,1.),(1.,
1.),(1.,1.),(1.,1.),(1.,1.),(1.,1.),(1.,1.),(1.,1.),(1.,1.),(1.,1.),(1.,
1.),(1.,1.),(1.,1.),(1.,1.),(1.,1.),(1.,1.),(1.,1.),(1.,1.),(1.,1.),(1.,
1.),(1.,1.),(1.,1.),(1.,1.),(1.,1.),(1.,1.),(1.,1.),(1.,1.),(1.,1.),(1.,
1.),(1.,1.),(1.,1.),(1.,1.),(1.,1.),(1.,1.),(1.,1.),(1.,1.),(1.,1.),(1.,
1.),(1.,1.),(1.,1.),(1.,1.),(1.,1.),(1.,1.),(1.,1.),(1.,1.),(1.,1.),(1.,
1.),(1.,1.)))
REPRESENTATION_ITEM('')
SURFACE()
);
#121=(
BOUNDED_SURFACE()
B_SPLINE_SURFACE(5,1,((#60104,#60105),(#60106,#60107),(#60108,#60109),(#60110,
#60111),(#60112,#60113),(#60114,#60115),(#60116,#60117),(#60118,#60119),
(#60120,#60121),(#60122,#60123),(#60124,#60125),(#60126,#60127),(#60128,
#60129),(#60130,#60131),(#60132,#60133),(#60134,#60135),(#60136,#60137),
(#60138,#60139),(#60140,#60141),(#60142,#60143),(#60144,#60145),(#60146,
#60147),(#60148,#60149),(#60150,#60151),(#60152,#60153),(#60154,#60155),
(#60156,#60157),(#60158,#60159),(#60160,#60161),(#60162,#60163),(#60164,
#60165),(#60166,#60167),(#60168,#60169),(#60170,#60171),(#60172,#60173),
(#60174,#60175),(#60176,#60177),(#60178,#60179),(#60180,#60181),(#60182,
#60183),(#60184,#60185),(#60186,#60187),(#60188,#60189),(#60190,#60191),
(#60192,#60193),(#60194,#60195),(#60196,#60197),(#60198,#60199),(#60200,
#60201),(#60202,#60203),(#60204,#60205),(#60206,#60207),(#60208,#60209),
(#60210,#60211),(#60212,#60213),(#60214,#60215),(#60216,#60217),(#60218,
#60219),(#60220,#60221),(#60222,#60223),(#60224,#60225),(#60226,#60227),
(#60228,#60229),(#60230,#60231),(#60232,#60233),(#60234,#60235),(#60236,
#60237),(#60238,#60239),(#60240,#60241),(#60242,#60243)),.UNSPECIFIED.,
 .F.,.F.,.F.)
B_SPLINE_SURFACE_WITH_KNOTS((6,1,1,1,1,1,1,1,1,1,1,1,1,1,1,1,1,1,1,1,1,
1,1,1,1,1,1,1,1,1,1,1,1,1,1,1,1,1,1,1,1,1,1,1,1,1,1,1,1,1,1,1,1,1,1,1,1,
1,1,1,1,1,1,1,1,6),(2,2),(-1.,-0.984615384615383,-0.969230769230768,-0.953846153846152,
-0.938461538461537,-0.923076923076922,-0.907692307692306,-0.892307692307691,
-0.876923076923076,-0.86153846153846,-0.846153846153845,-0.83076923076923,
-0.815384615384614,-0.799999999999999,-0.784615384615384,-0.769230769230768,
-0.753846153846153,-0.738461538461538,-0.723076923076922,-0.707692307692307,
-0.692307692307692,-0.676923076923076,-0.661538461538461,-0.646153846153846,
-0.63076923076923,-0.615384615384615,-0.6,-0.584615384615384,-0.569230769230769,
-0.553846153846154,-0.538461538461538,-0.523076923076923,-0.507692307692308,
-0.492307692307692,-0.476923076923077,-0.461538461538462,-0.446153846153846,
-0.430769230769231,-0.415384615384615,-0.4,-0.384615384615385,-0.369230769230769,
-0.353846153846154,-0.338461538461538,-0.323076923076923,-0.307692307692308,
-0.292307692307692,-0.276923076923077,-0.261538461538462,-0.246153846153846,
-0.230769230769231,-0.215384615384615,-0.2,-0.184615384615385,-0.169230769230769,
-0.153846153846154,-0.138461538461538,-0.123076923076923,-0.107692307692308,
-0.0923076923076923,-0.0769230769230769,-0.0615384615384615,-0.0461538461538462,
-0.0307692307692308,-0.0153846153846154,0.),(-1.,1.),.UNSPECIFIED.)
GEOMETRIC_REPRESENTATION_ITEM()
RATIONAL_B_SPLINE_SURFACE(((1.,1.),(1.,1.),(1.,1.),(1.,1.),(1.,1.),(1.,
1.),(1.,1.),(1.,1.),(1.,1.),(1.,1.),(1.,1.),(1.,1.),(1.,1.),(1.,1.),(1.,
1.),(1.,1.),(1.,1.),(1.,1.),(1.,1.),(1.,1.),(1.,1.),(1.,1.),(1.,1.),(1.,
1.),(1.,1.),(1.,1.),(1.,1.),(1.,1.),(1.,1.),(1.,1.),(1.,1.),(1.,1.),(1.,
1.),(1.,1.),(1.,1.),(1.,1.),(1.,1.),(1.,1.),(1.,1.),(1.,1.),(1.,1.),(1.,
1.),(1.,1.),(1.,1.),(1.,1.),(1.,1.),(1.,1.),(1.,1.),(1.,1.),(1.,1.),(1.,
1.),(1.,1.),(1.,1.),(1.,1.),(1.,1.),(1.,1.),(1.,1.),(1.,1.),(1.,1.),(1.,
1.),(1.,1.),(1.,1.),(1.,1.),(1.,1.),(1.,1.),(1.,1.),(1.,1.),(1.,1.),(1.,
1.),(1.,1.)))
REPRESENTATION_ITEM('')
SURFACE()
);
#122=(
BOUNDED_SURFACE()
B_SPLINE_SURFACE(5,1,((#60316,#60317),(#60318,#60319),(#60320,#60321),(#60322,
#60323),(#60324,#60325),(#60326,#60327),(#60328,#60329),(#60330,#60331),
(#60332,#60333),(#60334,#60335),(#60336,#60337),(#60338,#60339),(#60340,
#60341),(#60342,#60343),(#60344,#60345),(#60346,#60347),(#60348,#60349),
(#60350,#60351),(#60352,#60353),(#60354,#60355),(#60356,#60357),(#60358,
#60359),(#60360,#60361),(#60362,#60363),(#60364,#60365),(#60366,#60367),
(#60368,#60369),(#60370,#60371),(#60372,#60373),(#60374,#60375),(#60376,
#60377),(#60378,#60379),(#60380,#60381),(#60382,#60383),(#60384,#60385),
(#60386,#60387),(#60388,#60389),(#60390,#60391),(#60392,#60393),(#60394,
#60395),(#60396,#60397),(#60398,#60399),(#60400,#60401),(#60402,#60403),
(#60404,#60405),(#60406,#60407),(#60408,#60409),(#60410,#60411),(#60412,
#60413),(#60414,#60415),(#60416,#60417),(#60418,#60419),(#60420,#60421),
(#60422,#60423),(#60424,#60425),(#60426,#60427),(#60428,#60429),(#60430,
#60431),(#60432,#60433),(#60434,#60435),(#60436,#60437),(#60438,#60439),
(#60440,#60441),(#60442,#60443),(#60444,#60445),(#60446,#60447),(#60448,
#60449),(#60450,#60451),(#60452,#60453),(#60454,#60455)),.UNSPECIFIED.,
 .F.,.F.,.F.)
B_SPLINE_SURFACE_WITH_KNOTS((6,1,1,1,1,1,1,1,1,1,1,1,1,1,1,1,1,1,1,1,1,
1,1,1,1,1,1,1,1,1,1,1,1,1,1,1,1,1,1,1,1,1,1,1,1,1,1,1,1,1,1,1,1,1,1,1,1,
1,1,1,1,1,1,1,1,6),(2,2),(-1.,-0.984615384615383,-0.969230769230768,-0.953846153846152,
-0.938461538461537,-0.923076923076922,-0.907692307692306,-0.892307692307691,
-0.876923076923076,-0.86153846153846,-0.846153846153845,-0.83076923076923,
-0.815384615384614,-0.799999999999999,-0.784615384615384,-0.769230769230768,
-0.753846153846153,-0.738461538461538,-0.723076923076922,-0.707692307692307,
-0.692307692307692,-0.676923076923076,-0.661538461538461,-0.646153846153846,
-0.63076923076923,-0.615384615384615,-0.6,-0.584615384615384,-0.569230769230769,
-0.553846153846154,-0.538461538461538,-0.523076923076923,-0.507692307692308,
-0.492307692307692,-0.476923076923077,-0.461538461538462,-0.446153846153846,
-0.430769230769231,-0.415384615384615,-0.4,-0.384615384615385,-0.369230769230769,
-0.353846153846154,-0.338461538461538,-0.323076923076923,-0.307692307692308,
-0.292307692307692,-0.276923076923077,-0.261538461538462,-0.246153846153846,
-0.230769230769231,-0.215384615384615,-0.2,-0.184615384615385,-0.169230769230769,
-0.153846153846154,-0.138461538461538,-0.123076923076923,-0.107692307692308,
-0.0923076923076923,-0.0769230769230769,-0.0615384615384615,-0.0461538461538462,
-0.0307692307692308,-0.0153846153846154,0.),(-1.,1.),.UNSPECIFIED.)
GEOMETRIC_REPRESENTATION_ITEM()
RATIONAL_B_SPLINE_SURFACE(((1.,1.),(1.,1.),(1.,1.),(1.,1.),(1.,1.),(1.,
1.),(1.,1.),(1.,1.),(1.,1.),(1.,1.),(1.,1.),(1.,1.),(1.,1.),(1.,1.),(1.,
1.),(1.,1.),(1.,1.),(1.,1.),(1.,1.),(1.,1.),(1.,1.),(1.,1.),(1.,1.),(1.,
1.),(1.,1.),(1.,1.),(1.,1.),(1.,1.),(1.,1.),(1.,1.),(1.,1.),(1.,1.),(1.,
1.),(1.,1.),(1.,1.),(1.,1.),(1.,1.),(1.,1.),(1.,1.),(1.,1.),(1.,1.),(1.,
1.),(1.,1.),(1.,1.),(1.,1.),(1.,1.),(1.,1.),(1.,1.),(1.,1.),(1.,1.),(1.,
1.),(1.,1.),(1.,1.),(1.,1.),(1.,1.),(1.,1.),(1.,1.),(1.,1.),(1.,1.),(1.,
1.),(1.,1.),(1.,1.),(1.,1.),(1.,1.),(1.,1.),(1.,1.),(1.,1.),(1.,1.),(1.,
1.),(1.,1.)))
REPRESENTATION_ITEM('')
SURFACE()
);
#123=(
BOUNDED_SURFACE()
B_SPLINE_SURFACE(5,1,((#60546,#60547),(#60548,#60549),(#60550,#60551),(#60552,
#60553),(#60554,#60555),(#60556,#60557),(#60558,#60559),(#60560,#60561),
(#60562,#60563),(#60564,#60565),(#60566,#60567),(#60568,#60569),(#60570,
#60571),(#60572,#60573),(#60574,#60575),(#60576,#60577),(#60578,#60579),
(#60580,#60581),(#60582,#60583),(#60584,#60585),(#60586,#60587),(#60588,
#60589),(#60590,#60591),(#60592,#60593),(#60594,#60595),(#60596,#60597),
(#60598,#60599),(#60600,#60601),(#60602,#60603),(#60604,#60605),(#60606,
#60607),(#60608,#60609),(#60610,#60611),(#60612,#60613),(#60614,#60615),
(#60616,#60617),(#60618,#60619),(#60620,#60621),(#60622,#60623),(#60624,
#60625),(#60626,#60627),(#60628,#60629),(#60630,#60631),(#60632,#60633),
(#60634,#60635),(#60636,#60637),(#60638,#60639),(#60640,#60641),(#60642,
#60643),(#60644,#60645),(#60646,#60647),(#60648,#60649),(#60650,#60651),
(#60652,#60653),(#60654,#60655),(#60656,#60657),(#60658,#60659),(#60660,
#60661),(#60662,#60663),(#60664,#60665),(#60666,#60667),(#60668,#60669),
(#60670,#60671),(#60672,#60673),(#60674,#60675),(#60676,#60677),(#60678,
#60679),(#60680,#60681),(#60682,#60683),(#60684,#60685)),.UNSPECIFIED.,
 .F.,.F.,.F.)
B_SPLINE_SURFACE_WITH_KNOTS((6,1,1,1,1,1,1,1,1,1,1,1,1,1,1,1,1,1,1,1,1,
1,1,1,1,1,1,1,1,1,1,1,1,1,1,1,1,1,1,1,1,1,1,1,1,1,1,1,1,1,1,1,1,1,1,1,1,
1,1,1,1,1,1,1,1,6),(2,2),(-1.,-0.984615384615383,-0.969230769230768,-0.953846153846152,
-0.938461538461537,-0.923076923076922,-0.907692307692306,-0.892307692307691,
-0.876923076923076,-0.86153846153846,-0.846153846153845,-0.83076923076923,
-0.815384615384614,-0.799999999999999,-0.784615384615384,-0.769230769230768,
-0.753846153846153,-0.738461538461538,-0.723076923076922,-0.707692307692307,
-0.692307692307692,-0.676923076923076,-0.661538461538461,-0.646153846153846,
-0.63076923076923,-0.615384615384615,-0.6,-0.584615384615384,-0.569230769230769,
-0.553846153846154,-0.538461538461538,-0.523076923076923,-0.507692307692308,
-0.492307692307692,-0.476923076923077,-0.461538461538462,-0.446153846153846,
-0.430769230769231,-0.415384615384615,-0.4,-0.384615384615385,-0.369230769230769,
-0.353846153846154,-0.338461538461538,-0.323076923076923,-0.307692307692308,
-0.292307692307692,-0.276923076923077,-0.261538461538462,-0.246153846153846,
-0.230769230769231,-0.215384615384615,-0.2,-0.184615384615385,-0.169230769230769,
-0.153846153846154,-0.138461538461538,-0.123076923076923,-0.107692307692308,
-0.0923076923076923,-0.0769230769230769,-0.0615384615384615,-0.0461538461538462,
-0.0307692307692308,-0.0153846153846154,0.),(-1.,1.),.UNSPECIFIED.)
GEOMETRIC_REPRESENTATION_ITEM()
RATIONAL_B_SPLINE_SURFACE(((1.,1.),(1.,1.),(1.,1.),(1.,1.),(1.,1.),(1.,
1.),(1.,1.),(1.,1.),(1.,1.),(1.,1.),(1.,1.),(1.,1.),(1.,1.),(1.,1.),(1.,
1.),(1.,1.),(1.,1.),(1.,1.),(1.,1.),(1.,1.),(1.,1.),(1.,1.),(1.,1.),(1.,
1.),(1.,1.),(1.,1.),(1.,1.),(1.,1.),(1.,1.),(1.,1.),(1.,1.),(1.,1.),(1.,
1.),(1.,1.),(1.,1.),(1.,1.),(1.,1.),(1.,1.),(1.,1.),(1.,1.),(1.,1.),(1.,
1.),(1.,1.),(1.,1.),(1.,1.),(1.,1.),(1.,1.),(1.,1.),(1.,1.),(1.,1.),(1.,
1.),(1.,1.),(1.,1.),(1.,1.),(1.,1.),(1.,1.),(1.,1.),(1.,1.),(1.,1.),(1.,
1.),(1.,1.),(1.,1.),(1.,1.),(1.,1.),(1.,1.),(1.,1.),(1.,1.),(1.,1.),(1.,
1.),(1.,1.)))
REPRESENTATION_ITEM('')
SURFACE()
);
#124=(
BOUNDED_SURFACE()
B_SPLINE_SURFACE(5,1,((#60758,#60759),(#60760,#60761),(#60762,#60763),(#60764,
#60765),(#60766,#60767),(#60768,#60769),(#60770,#60771),(#60772,#60773),
(#60774,#60775),(#60776,#60777),(#60778,#60779),(#60780,#60781),(#60782,
#60783),(#60784,#60785),(#60786,#60787),(#60788,#60789),(#60790,#60791),
(#60792,#60793),(#60794,#60795),(#60796,#60797),(#60798,#60799),(#60800,
#60801),(#60802,#60803),(#60804,#60805),(#60806,#60807),(#60808,#60809),
(#60810,#60811),(#60812,#60813),(#60814,#60815),(#60816,#60817),(#60818,
#60819),(#60820,#60821),(#60822,#60823),(#60824,#60825),(#60826,#60827),
(#60828,#60829),(#60830,#60831),(#60832,#60833),(#60834,#60835),(#60836,
#60837),(#60838,#60839),(#60840,#60841),(#60842,#60843),(#60844,#60845),
(#60846,#60847),(#60848,#60849),(#60850,#60851),(#60852,#60853),(#60854,
#60855),(#60856,#60857),(#60858,#60859),(#60860,#60861),(#60862,#60863),
(#60864,#60865),(#60866,#60867),(#60868,#60869),(#60870,#60871),(#60872,
#60873),(#60874,#60875),(#60876,#60877),(#60878,#60879),(#60880,#60881),
(#60882,#60883),(#60884,#60885),(#60886,#60887),(#60888,#60889),(#60890,
#60891),(#60892,#60893),(#60894,#60895),(#60896,#60897)),.UNSPECIFIED.,
 .F.,.F.,.F.)
B_SPLINE_SURFACE_WITH_KNOTS((6,1,1,1,1,1,1,1,1,1,1,1,1,1,1,1,1,1,1,1,1,
1,1,1,1,1,1,1,1,1,1,1,1,1,1,1,1,1,1,1,1,1,1,1,1,1,1,1,1,1,1,1,1,1,1,1,1,
1,1,1,1,1,1,1,1,6),(2,2),(-1.,-0.984615384615383,-0.969230769230768,-0.953846153846152,
-0.938461538461537,-0.923076923076922,-0.907692307692306,-0.892307692307691,
-0.876923076923076,-0.86153846153846,-0.846153846153845,-0.83076923076923,
-0.815384615384614,-0.799999999999999,-0.784615384615384,-0.769230769230768,
-0.753846153846153,-0.738461538461538,-0.723076923076922,-0.707692307692307,
-0.692307692307692,-0.676923076923076,-0.661538461538461,-0.646153846153846,
-0.63076923076923,-0.615384615384615,-0.6,-0.584615384615384,-0.569230769230769,
-0.553846153846154,-0.538461538461538,-0.523076923076923,-0.507692307692308,
-0.492307692307692,-0.476923076923077,-0.461538461538462,-0.446153846153846,
-0.430769230769231,-0.415384615384615,-0.4,-0.384615384615385,-0.369230769230769,
-0.353846153846154,-0.338461538461538,-0.323076923076923,-0.307692307692308,
-0.292307692307692,-0.276923076923077,-0.261538461538462,-0.246153846153846,
-0.230769230769231,-0.215384615384615,-0.2,-0.184615384615385,-0.169230769230769,
-0.153846153846154,-0.138461538461538,-0.123076923076923,-0.107692307692308,
-0.0923076923076923,-0.0769230769230769,-0.0615384615384615,-0.0461538461538462,
-0.0307692307692308,-0.0153846153846154,0.),(-1.,1.),.UNSPECIFIED.)
GEOMETRIC_REPRESENTATION_ITEM()
RATIONAL_B_SPLINE_SURFACE(((1.,1.),(1.,1.),(1.,1.),(1.,1.),(1.,1.),(1.,
1.),(1.,1.),(1.,1.),(1.,1.),(1.,1.),(1.,1.),(1.,1.),(1.,1.),(1.,1.),(1.,
1.),(1.,1.),(1.,1.),(1.,1.),(1.,1.),(1.,1.),(1.,1.),(1.,1.),(1.,1.),(1.,
1.),(1.,1.),(1.,1.),(1.,1.),(1.,1.),(1.,1.),(1.,1.),(1.,1.),(1.,1.),(1.,
1.),(1.,1.),(1.,1.),(1.,1.),(1.,1.),(1.,1.),(1.,1.),(1.,1.),(1.,1.),(1.,
1.),(1.,1.),(1.,1.),(1.,1.),(1.,1.),(1.,1.),(1.,1.),(1.,1.),(1.,1.),(1.,
1.),(1.,1.),(1.,1.),(1.,1.),(1.,1.),(1.,1.),(1.,1.),(1.,1.),(1.,1.),(1.,
1.),(1.,1.),(1.,1.),(1.,1.),(1.,1.),(1.,1.),(1.,1.),(1.,1.),(1.,1.),(1.,
1.),(1.,1.)))
REPRESENTATION_ITEM('')
SURFACE()
);
#125=(
BOUNDED_SURFACE()
B_SPLINE_SURFACE(5,1,((#60988,#60989),(#60990,#60991),(#60992,#60993),(#60994,
#60995),(#60996,#60997),(#60998,#60999),(#61000,#61001),(#61002,#61003),
(#61004,#61005),(#61006,#61007),(#61008,#61009),(#61010,#61011),(#61012,
#61013),(#61014,#61015),(#61016,#61017),(#61018,#61019),(#61020,#61021),
(#61022,#61023),(#61024,#61025),(#61026,#61027),(#61028,#61029),(#61030,
#61031),(#61032,#61033),(#61034,#61035),(#61036,#61037),(#61038,#61039),
(#61040,#61041),(#61042,#61043),(#61044,#61045),(#61046,#61047),(#61048,
#61049),(#61050,#61051),(#61052,#61053),(#61054,#61055),(#61056,#61057),
(#61058,#61059),(#61060,#61061),(#61062,#61063),(#61064,#61065),(#61066,
#61067),(#61068,#61069),(#61070,#61071),(#61072,#61073),(#61074,#61075),
(#61076,#61077),(#61078,#61079),(#61080,#61081),(#61082,#61083),(#61084,
#61085),(#61086,#61087),(#61088,#61089),(#61090,#61091),(#61092,#61093),
(#61094,#61095),(#61096,#61097),(#61098,#61099),(#61100,#61101),(#61102,
#61103),(#61104,#61105),(#61106,#61107),(#61108,#61109),(#61110,#61111),
(#61112,#61113),(#61114,#61115),(#61116,#61117),(#61118,#61119),(#61120,
#61121),(#61122,#61123),(#61124,#61125),(#61126,#61127)),.UNSPECIFIED.,
 .F.,.F.,.F.)
B_SPLINE_SURFACE_WITH_KNOTS((6,1,1,1,1,1,1,1,1,1,1,1,1,1,1,1,1,1,1,1,1,
1,1,1,1,1,1,1,1,1,1,1,1,1,1,1,1,1,1,1,1,1,1,1,1,1,1,1,1,1,1,1,1,1,1,1,1,
1,1,1,1,1,1,1,1,6),(2,2),(-1.,-0.984615384615383,-0.969230769230768,-0.953846153846152,
-0.938461538461537,-0.923076923076922,-0.907692307692306,-0.892307692307691,
-0.876923076923076,-0.86153846153846,-0.846153846153845,-0.83076923076923,
-0.815384615384614,-0.799999999999999,-0.784615384615384,-0.769230769230768,
-0.753846153846153,-0.738461538461538,-0.723076923076922,-0.707692307692307,
-0.692307692307692,-0.676923076923076,-0.661538461538461,-0.646153846153846,
-0.63076923076923,-0.615384615384615,-0.6,-0.584615384615384,-0.569230769230769,
-0.553846153846154,-0.538461538461538,-0.523076923076923,-0.507692307692308,
-0.492307692307692,-0.476923076923077,-0.461538461538462,-0.446153846153846,
-0.430769230769231,-0.415384615384615,-0.4,-0.384615384615385,-0.369230769230769,
-0.353846153846154,-0.338461538461538,-0.323076923076923,-0.307692307692308,
-0.292307692307692,-0.276923076923077,-0.261538461538462,-0.246153846153846,
-0.230769230769231,-0.215384615384615,-0.2,-0.184615384615385,-0.169230769230769,
-0.153846153846154,-0.138461538461538,-0.123076923076923,-0.107692307692308,
-0.0923076923076923,-0.0769230769230769,-0.0615384615384615,-0.0461538461538462,
-0.0307692307692308,-0.0153846153846154,0.),(-1.,1.),.UNSPECIFIED.)
GEOMETRIC_REPRESENTATION_ITEM()
RATIONAL_B_SPLINE_SURFACE(((1.,1.),(1.,1.),(1.,1.),(1.,1.),(1.,1.),(1.,
1.),(1.,1.),(1.,1.),(1.,1.),(1.,1.),(1.,1.),(1.,1.),(1.,1.),(1.,1.),(1.,
1.),(1.,1.),(1.,1.),(1.,1.),(1.,1.),(1.,1.),(1.,1.),(1.,1.),(1.,1.),(1.,
1.),(1.,1.),(1.,1.),(1.,1.),(1.,1.),(1.,1.),(1.,1.),(1.,1.),(1.,1.),(1.,
1.),(1.,1.),(1.,1.),(1.,1.),(1.,1.),(1.,1.),(1.,1.),(1.,1.),(1.,1.),(1.,
1.),(1.,1.),(1.,1.),(1.,1.),(1.,1.),(1.,1.),(1.,1.),(1.,1.),(1.,1.),(1.,
1.),(1.,1.),(1.,1.),(1.,1.),(1.,1.),(1.,1.),(1.,1.),(1.,1.),(1.,1.),(1.,
1.),(1.,1.),(1.,1.),(1.,1.),(1.,1.),(1.,1.),(1.,1.),(1.,1.),(1.,1.),(1.,
1.),(1.,1.)))
REPRESENTATION_ITEM('')
SURFACE()
);
#126=(
BOUNDED_SURFACE()
B_SPLINE_SURFACE(5,1,((#61200,#61201),(#61202,#61203),(#61204,#61205),(#61206,
#61207),(#61208,#61209),(#61210,#61211),(#61212,#61213),(#61214,#61215),
(#61216,#61217),(#61218,#61219),(#61220,#61221),(#61222,#61223),(#61224,
#61225),(#61226,#61227),(#61228,#61229),(#61230,#61231),(#61232,#61233),
(#61234,#61235),(#61236,#61237),(#61238,#61239),(#61240,#61241),(#61242,
#61243),(#61244,#61245),(#61246,#61247),(#61248,#61249),(#61250,#61251),
(#61252,#61253),(#61254,#61255),(#61256,#61257),(#61258,#61259),(#61260,
#61261),(#61262,#61263),(#61264,#61265),(#61266,#61267),(#61268,#61269),
(#61270,#61271),(#61272,#61273),(#61274,#61275),(#61276,#61277),(#61278,
#61279),(#61280,#61281),(#61282,#61283),(#61284,#61285),(#61286,#61287),
(#61288,#61289),(#61290,#61291),(#61292,#61293),(#61294,#61295),(#61296,
#61297),(#61298,#61299),(#61300,#61301),(#61302,#61303),(#61304,#61305),
(#61306,#61307),(#61308,#61309),(#61310,#61311),(#61312,#61313),(#61314,
#61315),(#61316,#61317),(#61318,#61319),(#61320,#61321),(#61322,#61323),
(#61324,#61325),(#61326,#61327),(#61328,#61329),(#61330,#61331),(#61332,
#61333),(#61334,#61335),(#61336,#61337),(#61338,#61339)),.UNSPECIFIED.,
 .F.,.F.,.F.)
B_SPLINE_SURFACE_WITH_KNOTS((6,1,1,1,1,1,1,1,1,1,1,1,1,1,1,1,1,1,1,1,1,
1,1,1,1,1,1,1,1,1,1,1,1,1,1,1,1,1,1,1,1,1,1,1,1,1,1,1,1,1,1,1,1,1,1,1,1,
1,1,1,1,1,1,1,1,6),(2,2),(-1.,-0.984615384615383,-0.969230769230768,-0.953846153846152,
-0.938461538461537,-0.923076923076922,-0.907692307692306,-0.892307692307691,
-0.876923076923076,-0.86153846153846,-0.846153846153845,-0.83076923076923,
-0.815384615384614,-0.799999999999999,-0.784615384615384,-0.769230769230768,
-0.753846153846153,-0.738461538461538,-0.723076923076922,-0.707692307692307,
-0.692307692307692,-0.676923076923076,-0.661538461538461,-0.646153846153846,
-0.63076923076923,-0.615384615384615,-0.6,-0.584615384615384,-0.569230769230769,
-0.553846153846154,-0.538461538461538,-0.523076923076923,-0.507692307692308,
-0.492307692307692,-0.476923076923077,-0.461538461538462,-0.446153846153846,
-0.430769230769231,-0.415384615384615,-0.4,-0.384615384615385,-0.369230769230769,
-0.353846153846154,-0.338461538461538,-0.323076923076923,-0.307692307692308,
-0.292307692307692,-0.276923076923077,-0.261538461538462,-0.246153846153846,
-0.230769230769231,-0.215384615384615,-0.2,-0.184615384615385,-0.169230769230769,
-0.153846153846154,-0.138461538461538,-0.123076923076923,-0.107692307692308,
-0.0923076923076923,-0.0769230769230769,-0.0615384615384615,-0.0461538461538462,
-0.0307692307692308,-0.0153846153846154,0.),(-1.,1.),.UNSPECIFIED.)
GEOMETRIC_REPRESENTATION_ITEM()
RATIONAL_B_SPLINE_SURFACE(((1.,1.),(1.,1.),(1.,1.),(1.,1.),(1.,1.),(1.,
1.),(1.,1.),(1.,1.),(1.,1.),(1.,1.),(1.,1.),(1.,1.),(1.,1.),(1.,1.),(1.,
1.),(1.,1.),(1.,1.),(1.,1.),(1.,1.),(1.,1.),(1.,1.),(1.,1.),(1.,1.),(1.,
1.),(1.,1.),(1.,1.),(1.,1.),(1.,1.),(1.,1.),(1.,1.),(1.,1.),(1.,1.),(1.,
1.),(1.,1.),(1.,1.),(1.,1.),(1.,1.),(1.,1.),(1.,1.),(1.,1.),(1.,1.),(1.,
1.),(1.,1.),(1.,1.),(1.,1.),(1.,1.),(1.,1.),(1.,1.),(1.,1.),(1.,1.),(1.,
1.),(1.,1.),(1.,1.),(1.,1.),(1.,1.),(1.,1.),(1.,1.),(1.,1.),(1.,1.),(1.,
1.),(1.,1.),(1.,1.),(1.,1.),(1.,1.),(1.,1.),(1.,1.),(1.,1.),(1.,1.),(1.,
1.),(1.,1.)))
REPRESENTATION_ITEM('')
SURFACE()
);
#127=(
BOUNDED_SURFACE()
B_SPLINE_SURFACE(5,1,((#61430,#61431),(#61432,#61433),(#61434,#61435),(#61436,
#61437),(#61438,#61439),(#61440,#61441),(#61442,#61443),(#61444,#61445),
(#61446,#61447),(#61448,#61449),(#61450,#61451),(#61452,#61453),(#61454,
#61455),(#61456,#61457),(#61458,#61459),(#61460,#61461),(#61462,#61463),
(#61464,#61465),(#61466,#61467),(#61468,#61469),(#61470,#61471),(#61472,
#61473),(#61474,#61475),(#61476,#61477),(#61478,#61479),(#61480,#61481),
(#61482,#61483),(#61484,#61485),(#61486,#61487),(#61488,#61489),(#61490,
#61491),(#61492,#61493),(#61494,#61495),(#61496,#61497),(#61498,#61499),
(#61500,#61501),(#61502,#61503),(#61504,#61505),(#61506,#61507),(#61508,
#61509),(#61510,#61511),(#61512,#61513),(#61514,#61515),(#61516,#61517),
(#61518,#61519),(#61520,#61521),(#61522,#61523),(#61524,#61525),(#61526,
#61527),(#61528,#61529),(#61530,#61531),(#61532,#61533),(#61534,#61535),
(#61536,#61537),(#61538,#61539),(#61540,#61541),(#61542,#61543),(#61544,
#61545),(#61546,#61547),(#61548,#61549),(#61550,#61551),(#61552,#61553),
(#61554,#61555),(#61556,#61557),(#61558,#61559),(#61560,#61561),(#61562,
#61563),(#61564,#61565),(#61566,#61567),(#61568,#61569)),.UNSPECIFIED.,
 .F.,.F.,.F.)
B_SPLINE_SURFACE_WITH_KNOTS((6,1,1,1,1,1,1,1,1,1,1,1,1,1,1,1,1,1,1,1,1,
1,1,1,1,1,1,1,1,1,1,1,1,1,1,1,1,1,1,1,1,1,1,1,1,1,1,1,1,1,1,1,1,1,1,1,1,
1,1,1,1,1,1,1,1,6),(2,2),(-1.,-0.984615384615383,-0.969230769230768,-0.953846153846152,
-0.938461538461537,-0.923076923076922,-0.907692307692306,-0.892307692307691,
-0.876923076923076,-0.86153846153846,-0.846153846153845,-0.83076923076923,
-0.815384615384614,-0.799999999999999,-0.784615384615384,-0.769230769230768,
-0.753846153846153,-0.738461538461538,-0.723076923076922,-0.707692307692307,
-0.692307692307692,-0.676923076923076,-0.661538461538461,-0.646153846153846,
-0.63076923076923,-0.615384615384615,-0.6,-0.584615384615384,-0.569230769230769,
-0.553846153846154,-0.538461538461538,-0.523076923076923,-0.507692307692308,
-0.492307692307692,-0.476923076923077,-0.461538461538462,-0.446153846153846,
-0.430769230769231,-0.415384615384615,-0.4,-0.384615384615385,-0.369230769230769,
-0.353846153846154,-0.338461538461538,-0.323076923076923,-0.307692307692308,
-0.292307692307692,-0.276923076923077,-0.261538461538462,-0.246153846153846,
-0.230769230769231,-0.215384615384615,-0.2,-0.184615384615385,-0.169230769230769,
-0.153846153846154,-0.138461538461538,-0.123076923076923,-0.107692307692308,
-0.0923076923076923,-0.0769230769230769,-0.0615384615384615,-0.0461538461538462,
-0.0307692307692308,-0.0153846153846154,0.),(-1.,1.),.UNSPECIFIED.)
GEOMETRIC_REPRESENTATION_ITEM()
RATIONAL_B_SPLINE_SURFACE(((1.,1.),(1.,1.),(1.,1.),(1.,1.),(1.,1.),(1.,
1.),(1.,1.),(1.,1.),(1.,1.),(1.,1.),(1.,1.),(1.,1.),(1.,1.),(1.,1.),(1.,
1.),(1.,1.),(1.,1.),(1.,1.),(1.,1.),(1.,1.),(1.,1.),(1.,1.),(1.,1.),(1.,
1.),(1.,1.),(1.,1.),(1.,1.),(1.,1.),(1.,1.),(1.,1.),(1.,1.),(1.,1.),(1.,
1.),(1.,1.),(1.,1.),(1.,1.),(1.,1.),(1.,1.),(1.,1.),(1.,1.),(1.,1.),(1.,
1.),(1.,1.),(1.,1.),(1.,1.),(1.,1.),(1.,1.),(1.,1.),(1.,1.),(1.,1.),(1.,
1.),(1.,1.),(1.,1.),(1.,1.),(1.,1.),(1.,1.),(1.,1.),(1.,1.),(1.,1.),(1.,
1.),(1.,1.),(1.,1.),(1.,1.),(1.,1.),(1.,1.),(1.,1.),(1.,1.),(1.,1.),(1.,
1.),(1.,1.)))
REPRESENTATION_ITEM('')
SURFACE()
);
#128=(
BOUNDED_SURFACE()
B_SPLINE_SURFACE(5,1,((#61646,#61647),(#61648,#61649),(#61650,#61651),(#61652,
#61653),(#61654,#61655),(#61656,#61657),(#61658,#61659),(#61660,#61661),
(#61662,#61663),(#61664,#61665),(#61666,#61667),(#61668,#61669),(#61670,
#61671),(#61672,#61673),(#61674,#61675),(#61676,#61677),(#61678,#61679),
(#61680,#61681),(#61682,#61683),(#61684,#61685),(#61686,#61687),(#61688,
#61689),(#61690,#61691),(#61692,#61693),(#61694,#61695),(#61696,#61697),
(#61698,#61699),(#61700,#61701),(#61702,#61703),(#61704,#61705),(#61706,
#61707),(#61708,#61709),(#61710,#61711),(#61712,#61713),(#61714,#61715),
(#61716,#61717),(#61718,#61719),(#61720,#61721),(#61722,#61723),(#61724,
#61725),(#61726,#61727),(#61728,#61729),(#61730,#61731),(#61732,#61733),
(#61734,#61735),(#61736,#61737),(#61738,#61739),(#61740,#61741),(#61742,
#61743),(#61744,#61745),(#61746,#61747),(#61748,#61749),(#61750,#61751),
(#61752,#61753),(#61754,#61755),(#61756,#61757),(#61758,#61759),(#61760,
#61761),(#61762,#61763),(#61764,#61765),(#61766,#61767),(#61768,#61769),
(#61770,#61771),(#61772,#61773),(#61774,#61775),(#61776,#61777),(#61778,
#61779),(#61780,#61781),(#61782,#61783),(#61784,#61785)),.UNSPECIFIED.,
 .F.,.F.,.F.)
B_SPLINE_SURFACE_WITH_KNOTS((6,1,1,1,1,1,1,1,1,1,1,1,1,1,1,1,1,1,1,1,1,
1,1,1,1,1,1,1,1,1,1,1,1,1,1,1,1,1,1,1,1,1,1,1,1,1,1,1,1,1,1,1,1,1,1,1,1,
1,1,1,1,1,1,1,1,6),(2,2),(-1.,-0.984615384615383,-0.969230769230768,-0.953846153846152,
-0.938461538461537,-0.923076923076922,-0.907692307692306,-0.892307692307691,
-0.876923076923076,-0.86153846153846,-0.846153846153845,-0.83076923076923,
-0.815384615384614,-0.799999999999999,-0.784615384615384,-0.769230769230768,
-0.753846153846153,-0.738461538461538,-0.723076923076922,-0.707692307692307,
-0.692307692307692,-0.676923076923076,-0.661538461538461,-0.646153846153846,
-0.63076923076923,-0.615384615384615,-0.6,-0.584615384615384,-0.569230769230769,
-0.553846153846154,-0.538461538461538,-0.523076923076923,-0.507692307692308,
-0.492307692307692,-0.476923076923077,-0.461538461538462,-0.446153846153846,
-0.430769230769231,-0.415384615384615,-0.4,-0.384615384615385,-0.369230769230769,
-0.353846153846154,-0.338461538461538,-0.323076923076923,-0.307692307692308,
-0.292307692307692,-0.276923076923077,-0.261538461538462,-0.246153846153846,
-0.230769230769231,-0.215384615384615,-0.2,-0.184615384615385,-0.169230769230769,
-0.153846153846154,-0.138461538461538,-0.123076923076923,-0.107692307692308,
-0.0923076923076923,-0.0769230769230769,-0.0615384615384615,-0.0461538461538462,
-0.0307692307692308,-0.0153846153846154,0.),(-1.,1.),.UNSPECIFIED.)
GEOMETRIC_REPRESENTATION_ITEM()
RATIONAL_B_SPLINE_SURFACE(((1.,1.),(1.,1.),(1.,1.),(1.,1.),(1.,1.),(1.,
1.),(1.,1.),(1.,1.),(1.,1.),(1.,1.),(1.,1.),(1.,1.),(1.,1.),(1.,1.),(1.,
1.),(1.,1.),(1.,1.),(1.,1.),(1.,1.),(1.,1.),(1.,1.),(1.,1.),(1.,1.),(1.,
1.),(1.,1.),(1.,1.),(1.,1.),(1.,1.),(1.,1.),(1.,1.),(1.,1.),(1.,1.),(1.,
1.),(1.,1.),(1.,1.),(1.,1.),(1.,1.),(1.,1.),(1.,1.),(1.,1.),(1.,1.),(1.,
1.),(1.,1.),(1.,1.),(1.,1.),(1.,1.),(1.,1.),(1.,1.),(1.,1.),(1.,1.),(1.,
1.),(1.,1.),(1.,1.),(1.,1.),(1.,1.),(1.,1.),(1.,1.),(1.,1.),(1.,1.),(1.,
1.),(1.,1.),(1.,1.),(1.,1.),(1.,1.),(1.,1.),(1.,1.),(1.,1.),(1.,1.),(1.,
1.),(1.,1.)))
REPRESENTATION_ITEM('')
SURFACE()
);
#129=(
BOUNDED_SURFACE()
B_SPLINE_SURFACE(5,1,((#61872,#61873),(#61874,#61875),(#61876,#61877),(#61878,
#61879),(#61880,#61881),(#61882,#61883),(#61884,#61885),(#61886,#61887),
(#61888,#61889),(#61890,#61891),(#61892,#61893),(#61894,#61895),(#61896,
#61897),(#61898,#61899),(#61900,#61901),(#61902,#61903),(#61904,#61905),
(#61906,#61907),(#61908,#61909),(#61910,#61911),(#61912,#61913),(#61914,
#61915),(#61916,#61917),(#61918,#61919),(#61920,#61921),(#61922,#61923),
(#61924,#61925),(#61926,#61927),(#61928,#61929),(#61930,#61931),(#61932,
#61933),(#61934,#61935),(#61936,#61937),(#61938,#61939),(#61940,#61941),
(#61942,#61943),(#61944,#61945),(#61946,#61947),(#61948,#61949),(#61950,
#61951),(#61952,#61953),(#61954,#61955),(#61956,#61957),(#61958,#61959),
(#61960,#61961),(#61962,#61963),(#61964,#61965),(#61966,#61967),(#61968,
#61969),(#61970,#61971),(#61972,#61973),(#61974,#61975),(#61976,#61977),
(#61978,#61979),(#61980,#61981),(#61982,#61983),(#61984,#61985),(#61986,
#61987),(#61988,#61989),(#61990,#61991),(#61992,#61993),(#61994,#61995),
(#61996,#61997),(#61998,#61999),(#62000,#62001),(#62002,#62003),(#62004,
#62005),(#62006,#62007),(#62008,#62009),(#62010,#62011)),.UNSPECIFIED.,
 .F.,.F.,.F.)
B_SPLINE_SURFACE_WITH_KNOTS((6,1,1,1,1,1,1,1,1,1,1,1,1,1,1,1,1,1,1,1,1,
1,1,1,1,1,1,1,1,1,1,1,1,1,1,1,1,1,1,1,1,1,1,1,1,1,1,1,1,1,1,1,1,1,1,1,1,
1,1,1,1,1,1,1,1,6),(2,2),(-1.,-0.984615384615383,-0.969230769230768,-0.953846153846152,
-0.938461538461537,-0.923076923076922,-0.907692307692306,-0.892307692307691,
-0.876923076923076,-0.86153846153846,-0.846153846153845,-0.83076923076923,
-0.815384615384614,-0.799999999999999,-0.784615384615384,-0.769230769230768,
-0.753846153846153,-0.738461538461538,-0.723076923076922,-0.707692307692307,
-0.692307692307692,-0.676923076923076,-0.661538461538461,-0.646153846153846,
-0.63076923076923,-0.615384615384615,-0.6,-0.584615384615384,-0.569230769230769,
-0.553846153846154,-0.538461538461538,-0.523076923076923,-0.507692307692308,
-0.492307692307692,-0.476923076923077,-0.461538461538462,-0.446153846153846,
-0.430769230769231,-0.415384615384615,-0.4,-0.384615384615385,-0.369230769230769,
-0.353846153846154,-0.338461538461538,-0.323076923076923,-0.307692307692308,
-0.292307692307692,-0.276923076923077,-0.261538461538462,-0.246153846153846,
-0.230769230769231,-0.215384615384615,-0.2,-0.184615384615385,-0.169230769230769,
-0.153846153846154,-0.138461538461538,-0.123076923076923,-0.107692307692308,
-0.0923076923076923,-0.0769230769230769,-0.0615384615384615,-0.0461538461538462,
-0.0307692307692308,-0.0153846153846154,0.),(-1.,1.),.UNSPECIFIED.)
GEOMETRIC_REPRESENTATION_ITEM()
RATIONAL_B_SPLINE_SURFACE(((1.,1.),(1.,1.),(1.,1.),(1.,1.),(1.,1.),(1.,
1.),(1.,1.),(1.,1.),(1.,1.),(1.,1.),(1.,1.),(1.,1.),(1.,1.),(1.,1.),(1.,
1.),(1.,1.),(1.,1.),(1.,1.),(1.,1.),(1.,1.),(1.,1.),(1.,1.),(1.,1.),(1.,
1.),(1.,1.),(1.,1.),(1.,1.),(1.,1.),(1.,1.),(1.,1.),(1.,1.),(1.,1.),(1.,
1.),(1.,1.),(1.,1.),(1.,1.),(1.,1.),(1.,1.),(1.,1.),(1.,1.),(1.,1.),(1.,
1.),(1.,1.),(1.,1.),(1.,1.),(1.,1.),(1.,1.),(1.,1.),(1.,1.),(1.,1.),(1.,
1.),(1.,1.),(1.,1.),(1.,1.),(1.,1.),(1.,1.),(1.,1.),(1.,1.),(1.,1.),(1.,
1.),(1.,1.),(1.,1.),(1.,1.),(1.,1.),(1.,1.),(1.,1.),(1.,1.),(1.,1.),(1.,
1.),(1.,1.)))
REPRESENTATION_ITEM('')
SURFACE()
);
#130=(
BOUNDED_SURFACE()
B_SPLINE_SURFACE(5,1,((#62091,#62092),(#62093,#62094),(#62095,#62096),(#62097,
#62098),(#62099,#62100),(#62101,#62102),(#62103,#62104),(#62105,#62106),
(#62107,#62108),(#62109,#62110),(#62111,#62112),(#62113,#62114),(#62115,
#62116),(#62117,#62118),(#62119,#62120),(#62121,#62122),(#62123,#62124),
(#62125,#62126),(#62127,#62128),(#62129,#62130),(#62131,#62132),(#62133,
#62134),(#62135,#62136),(#62137,#62138),(#62139,#62140),(#62141,#62142),
(#62143,#62144),(#62145,#62146),(#62147,#62148),(#62149,#62150),(#62151,
#62152),(#62153,#62154),(#62155,#62156),(#62157,#62158),(#62159,#62160),
(#62161,#62162),(#62163,#62164),(#62165,#62166),(#62167,#62168),(#62169,
#62170),(#62171,#62172),(#62173,#62174),(#62175,#62176),(#62177,#62178),
(#62179,#62180),(#62181,#62182),(#62183,#62184),(#62185,#62186),(#62187,
#62188),(#62189,#62190),(#62191,#62192),(#62193,#62194),(#62195,#62196),
(#62197,#62198),(#62199,#62200),(#62201,#62202),(#62203,#62204),(#62205,
#62206),(#62207,#62208),(#62209,#62210),(#62211,#62212),(#62213,#62214),
(#62215,#62216),(#62217,#62218),(#62219,#62220),(#62221,#62222),(#62223,
#62224),(#62225,#62226),(#62227,#62228),(#62229,#62230)),.UNSPECIFIED.,
 .F.,.F.,.F.)
B_SPLINE_SURFACE_WITH_KNOTS((6,1,1,1,1,1,1,1,1,1,1,1,1,1,1,1,1,1,1,1,1,
1,1,1,1,1,1,1,1,1,1,1,1,1,1,1,1,1,1,1,1,1,1,1,1,1,1,1,1,1,1,1,1,1,1,1,1,
1,1,1,1,1,1,1,1,6),(2,2),(-1.,-0.984615384615383,-0.969230769230768,-0.953846153846152,
-0.938461538461537,-0.923076923076922,-0.907692307692306,-0.892307692307691,
-0.876923076923076,-0.86153846153846,-0.846153846153845,-0.83076923076923,
-0.815384615384614,-0.799999999999999,-0.784615384615384,-0.769230769230768,
-0.753846153846153,-0.738461538461538,-0.723076923076922,-0.707692307692307,
-0.692307692307692,-0.676923076923076,-0.661538461538461,-0.646153846153846,
-0.63076923076923,-0.615384615384615,-0.6,-0.584615384615384,-0.569230769230769,
-0.553846153846154,-0.538461538461538,-0.523076923076923,-0.507692307692308,
-0.492307692307692,-0.476923076923077,-0.461538461538462,-0.446153846153846,
-0.430769230769231,-0.415384615384615,-0.4,-0.384615384615385,-0.369230769230769,
-0.353846153846154,-0.338461538461538,-0.323076923076923,-0.307692307692308,
-0.292307692307692,-0.276923076923077,-0.261538461538462,-0.246153846153846,
-0.230769230769231,-0.215384615384615,-0.2,-0.184615384615385,-0.169230769230769,
-0.153846153846154,-0.138461538461538,-0.123076923076923,-0.107692307692308,
-0.0923076923076923,-0.0769230769230769,-0.0615384615384615,-0.0461538461538462,
-0.0307692307692308,-0.0153846153846154,0.),(-1.,1.),.UNSPECIFIED.)
GEOMETRIC_REPRESENTATION_ITEM()
RATIONAL_B_SPLINE_SURFACE(((1.,1.),(1.,1.),(1.,1.),(1.,1.),(1.,1.),(1.,
1.),(1.,1.),(1.,1.),(1.,1.),(1.,1.),(1.,1.),(1.,1.),(1.,1.),(1.,1.),(1.,
1.),(1.,1.),(1.,1.),(1.,1.),(1.,1.),(1.,1.),(1.,1.),(1.,1.),(1.,1.),(1.,
1.),(1.,1.),(1.,1.),(1.,1.),(1.,1.),(1.,1.),(1.,1.),(1.,1.),(1.,1.),(1.,
1.),(1.,1.),(1.,1.),(1.,1.),(1.,1.),(1.,1.),(1.,1.),(1.,1.),(1.,1.),(1.,
1.),(1.,1.),(1.,1.),(1.,1.),(1.,1.),(1.,1.),(1.,1.),(1.,1.),(1.,1.),(1.,
1.),(1.,1.),(1.,1.),(1.,1.),(1.,1.),(1.,1.),(1.,1.),(1.,1.),(1.,1.),(1.,
1.),(1.,1.),(1.,1.),(1.,1.),(1.,1.),(1.,1.),(1.,1.),(1.,1.),(1.,1.),(1.,
1.),(1.,1.)))
REPRESENTATION_ITEM('')
SURFACE()
);
#131=(
BOUNDED_CURVE()
B_SPLINE_CURVE(5,(#26804,#26805,#26806,#26807,#26808,#26809,#26810,#26811,
#26812,#26813,#26814,#26815,#26816,#26817,#26818,#26819,#26820,#26821,#26822,
#26823,#26824,#26825,#26826,#26827,#26828,#26829,#26830,#26831,#26832,#26833,
#26834,#26835,#26836,#26837,#26838,#26839,#26840,#26841,#26842,#26843,#26844,
#26845,#26846,#26847,#26848,#26849,#26850,#26851,#26852,#26853,#26854,#26855,
#26856,#26857,#26858,#26859,#26860,#26861,#26862,#26863,#26864,#26865,#26866,
#26867,#26868,#26869,#26870,#26871,#26872,#26873),.UNSPECIFIED.,.F.,.F.)
B_SPLINE_CURVE_WITH_KNOTS((6,1,1,1,1,1,1,1,1,1,1,1,1,1,1,1,1,1,1,1,1,1,
1,1,1,1,1,1,1,1,1,1,1,1,1,1,1,1,1,1,1,1,1,1,1,1,1,1,1,1,1,1,1,1,1,1,1,1,
1,1,1,1,1,1,1,6),(0.,0.0153846153846154,0.0307692307692308,0.0461538461538462,
0.0615384615384615,0.0769230769230769,0.0923076923076923,0.107692307692308,
0.123076923076923,0.138461538461538,0.153846153846154,0.169230769230769,
0.184615384615385,0.2,0.215384615384615,0.230769230769231,0.246153846153846,
0.261538461538462,0.276923076923077,0.292307692307692,0.307692307692308,
0.323076923076923,0.338461538461538,0.353846153846154,0.369230769230769,
0.384615384615385,0.4,0.415384615384615,0.430769230769231,0.446153846153846,
0.461538461538462,0.476923076923077,0.492307692307692,0.507692307692308,
0.523076923076923,0.538461538461538,0.553846153846154,0.569230769230769,
0.584615384615384,0.6,0.615384615384615,0.63076923076923,0.646153846153846,
0.661538461538461,0.676923076923076,0.692307692307692,0.707692307692307,
0.723076923076922,0.738461538461538,0.753846153846153,0.769230769230768,
0.784615384615384,0.799999999999999,0.815384615384614,0.83076923076923,
0.846153846153845,0.86153846153846,0.876923076923076,0.892307692307691,
0.907692307692306,0.923076923076922,0.938461538461537,0.953846153846152,
0.969230769230768,0.984615384615383,1.),.UNSPECIFIED.)
CURVE()
GEOMETRIC_REPRESENTATION_ITEM()
RATIONAL_B_SPLINE_CURVE((1.,1.,1.,1.,1.,1.,1.,1.,1.,1.,1.,1.,1.,1.,1.,1.,
1.,1.,1.,1.,1.,1.,1.,1.,1.,1.,1.,1.,1.,1.,1.,1.,1.,1.,1.,1.,1.,1.,1.,1.,
1.,1.,1.,1.,1.,1.,1.,1.,1.,1.,1.,1.,1.,1.,1.,1.,1.,1.,1.,1.,1.,1.,1.,1.,
1.,1.,1.,1.,1.,1.))
REPRESENTATION_ITEM('')
);
#132=(
BOUNDED_CURVE()
B_SPLINE_CURVE(5,(#26877,#26878,#26879,#26880,#26881,#26882,#26883,#26884,
#26885,#26886,#26887,#26888,#26889,#26890,#26891,#26892,#26893,#26894,#26895,
#26896,#26897,#26898,#26899,#26900,#26901,#26902,#26903,#26904,#26905,#26906,
#26907,#26908,#26909,#26910,#26911,#26912,#26913,#26914,#26915,#26916,#26917,
#26918,#26919,#26920,#26921,#26922,#26923,#26924,#26925,#26926,#26927,#26928,
#26929,#26930,#26931,#26932,#26933,#26934,#26935,#26936,#26937,#26938,#26939,
#26940,#26941,#26942,#26943,#26944,#26945,#26946),.UNSPECIFIED.,.F.,.F.)
B_SPLINE_CURVE_WITH_KNOTS((6,1,1,1,1,1,1,1,1,1,1,1,1,1,1,1,1,1,1,1,1,1,
1,1,1,1,1,1,1,1,1,1,1,1,1,1,1,1,1,1,1,1,1,1,1,1,1,1,1,1,1,1,1,1,1,1,1,1,
1,1,1,1,1,1,1,6),(0.,0.0153846153846154,0.0307692307692308,0.0461538461538462,
0.0615384615384615,0.0769230769230769,0.0923076923076923,0.107692307692308,
0.123076923076923,0.138461538461538,0.153846153846154,0.169230769230769,
0.184615384615385,0.2,0.215384615384615,0.230769230769231,0.246153846153846,
0.261538461538462,0.276923076923077,0.292307692307692,0.307692307692308,
0.323076923076923,0.338461538461538,0.353846153846154,0.369230769230769,
0.384615384615385,0.4,0.415384615384615,0.430769230769231,0.446153846153846,
0.461538461538462,0.476923076923077,0.492307692307692,0.507692307692308,
0.523076923076923,0.538461538461538,0.553846153846154,0.569230769230769,
0.584615384615384,0.6,0.615384615384615,0.63076923076923,0.646153846153846,
0.661538461538461,0.676923076923076,0.692307692307692,0.707692307692307,
0.723076923076922,0.738461538461538,0.753846153846153,0.769230769230768,
0.784615384615384,0.799999999999999,0.815384615384614,0.83076923076923,
0.846153846153845,0.86153846153846,0.876923076923076,0.892307692307691,
0.907692307692306,0.923076923076922,0.938461538461537,0.953846153846152,
0.969230769230768,0.984615384615383,1.),.UNSPECIFIED.)
CURVE()
GEOMETRIC_REPRESENTATION_ITEM()
RATIONAL_B_SPLINE_CURVE((1.,1.,1.,1.,1.,1.,1.,1.,1.,1.,1.,1.,1.,1.,1.,1.,
1.,1.,1.,1.,1.,1.,1.,1.,1.,1.,1.,1.,1.,1.,1.,1.,1.,1.,1.,1.,1.,1.,1.,1.,
1.,1.,1.,1.,1.,1.,1.,1.,1.,1.,1.,1.,1.,1.,1.,1.,1.,1.,1.,1.,1.,1.,1.,1.,
1.,1.,1.,1.,1.,1.))
REPRESENTATION_ITEM('')
);
#133=(
BOUNDED_CURVE()
B_SPLINE_CURVE(5,(#26950,#26951,#26952,#26953,#26954,#26955,#26956,#26957,
#26958,#26959,#26960,#26961,#26962,#26963,#26964,#26965,#26966,#26967,#26968,
#26969,#26970,#26971,#26972,#26973,#26974,#26975,#26976,#26977,#26978,#26979,
#26980,#26981,#26982,#26983,#26984,#26985,#26986,#26987,#26988,#26989,#26990,
#26991,#26992,#26993,#26994,#26995,#26996,#26997,#26998,#26999,#27000,#27001,
#27002,#27003,#27004,#27005,#27006,#27007,#27008,#27009,#27010,#27011,#27012,
#27013,#27014,#27015,#27016,#27017,#27018,#27019),.UNSPECIFIED.,.F.,.F.)
B_SPLINE_CURVE_WITH_KNOTS((6,1,1,1,1,1,1,1,1,1,1,1,1,1,1,1,1,1,1,1,1,1,
1,1,1,1,1,1,1,1,1,1,1,1,1,1,1,1,1,1,1,1,1,1,1,1,1,1,1,1,1,1,1,1,1,1,1,1,
1,1,1,1,1,1,1,6),(0.,0.0153846153846154,0.0307692307692308,0.0461538461538462,
0.0615384615384615,0.0769230769230769,0.0923076923076923,0.107692307692308,
0.123076923076923,0.138461538461538,0.153846153846154,0.169230769230769,
0.184615384615385,0.2,0.215384615384615,0.230769230769231,0.246153846153846,
0.261538461538462,0.276923076923077,0.292307692307692,0.307692307692308,
0.323076923076923,0.338461538461538,0.353846153846154,0.369230769230769,
0.384615384615385,0.4,0.415384615384615,0.430769230769231,0.446153846153846,
0.461538461538462,0.476923076923077,0.492307692307692,0.507692307692308,
0.523076923076923,0.538461538461538,0.553846153846154,0.569230769230769,
0.584615384615384,0.6,0.615384615384615,0.63076923076923,0.646153846153846,
0.661538461538461,0.676923076923076,0.692307692307692,0.707692307692307,
0.723076923076922,0.738461538461538,0.753846153846153,0.769230769230768,
0.784615384615384,0.799999999999999,0.815384615384614,0.83076923076923,
0.846153846153845,0.86153846153846,0.876923076923076,0.892307692307691,
0.907692307692306,0.923076923076922,0.938461538461537,0.953846153846152,
0.969230769230768,0.984615384615383,1.),.UNSPECIFIED.)
CURVE()
GEOMETRIC_REPRESENTATION_ITEM()
RATIONAL_B_SPLINE_CURVE((1.,1.,1.,1.,1.,1.,1.,1.,1.,1.,1.,1.,1.,1.,1.,1.,
1.,1.,1.,1.,1.,1.,1.,1.,1.,1.,1.,1.,1.,1.,1.,1.,1.,1.,1.,1.,1.,1.,1.,1.,
1.,1.,1.,1.,1.,1.,1.,1.,1.,1.,1.,1.,1.,1.,1.,1.,1.,1.,1.,1.,1.,1.,1.,1.,
1.,1.,1.,1.,1.,1.))
REPRESENTATION_ITEM('')
);
#134=(
BOUNDED_CURVE()
B_SPLINE_CURVE(5,(#27023,#27024,#27025,#27026,#27027,#27028,#27029,#27030,
#27031,#27032,#27033,#27034,#27035,#27036,#27037,#27038,#27039,#27040,#27041,
#27042,#27043,#27044,#27045,#27046,#27047,#27048,#27049,#27050,#27051,#27052,
#27053,#27054,#27055,#27056,#27057,#27058,#27059,#27060,#27061,#27062,#27063,
#27064,#27065,#27066,#27067,#27068,#27069,#27070,#27071,#27072,#27073,#27074,
#27075,#27076,#27077,#27078,#27079,#27080,#27081,#27082,#27083,#27084,#27085,
#27086,#27087,#27088,#27089,#27090,#27091,#27092),.UNSPECIFIED.,.F.,.F.)
B_SPLINE_CURVE_WITH_KNOTS((6,1,1,1,1,1,1,1,1,1,1,1,1,1,1,1,1,1,1,1,1,1,
1,1,1,1,1,1,1,1,1,1,1,1,1,1,1,1,1,1,1,1,1,1,1,1,1,1,1,1,1,1,1,1,1,1,1,1,
1,1,1,1,1,1,1,6),(0.,0.0153846153846154,0.0307692307692308,0.0461538461538462,
0.0615384615384615,0.0769230769230769,0.0923076923076923,0.107692307692308,
0.123076923076923,0.138461538461538,0.153846153846154,0.169230769230769,
0.184615384615385,0.2,0.215384615384615,0.230769230769231,0.246153846153846,
0.261538461538462,0.276923076923077,0.292307692307692,0.307692307692308,
0.323076923076923,0.338461538461538,0.353846153846154,0.369230769230769,
0.384615384615385,0.4,0.415384615384615,0.430769230769231,0.446153846153846,
0.461538461538462,0.476923076923077,0.492307692307692,0.507692307692308,
0.523076923076923,0.538461538461538,0.553846153846154,0.569230769230769,
0.584615384615384,0.6,0.615384615384615,0.63076923076923,0.646153846153846,
0.661538461538461,0.676923076923076,0.692307692307692,0.707692307692307,
0.723076923076922,0.738461538461538,0.753846153846153,0.769230769230768,
0.784615384615384,0.799999999999999,0.815384615384614,0.83076923076923,
0.846153846153845,0.86153846153846,0.876923076923076,0.892307692307691,
0.907692307692306,0.923076923076922,0.938461538461537,0.953846153846152,
0.969230769230768,0.984615384615383,1.),.UNSPECIFIED.)
CURVE()
GEOMETRIC_REPRESENTATION_ITEM()
RATIONAL_B_SPLINE_CURVE((1.,1.,1.,1.,1.,1.,1.,1.,1.,1.,1.,1.,1.,1.,1.,1.,
1.,1.,1.,1.,1.,1.,1.,1.,1.,1.,1.,1.,1.,1.,1.,1.,1.,1.,1.,1.,1.,1.,1.,1.,
1.,1.,1.,1.,1.,1.,1.,1.,1.,1.,1.,1.,1.,1.,1.,1.,1.,1.,1.,1.,1.,1.,1.,1.,
1.,1.,1.,1.,1.,1.))
REPRESENTATION_ITEM('')
);
#135=(
BOUNDED_CURVE()
B_SPLINE_CURVE(5,(#27096,#27097,#27098,#27099,#27100,#27101,#27102,#27103,
#27104,#27105,#27106,#27107,#27108,#27109,#27110,#27111,#27112,#27113,#27114,
#27115,#27116,#27117,#27118,#27119,#27120,#27121,#27122,#27123,#27124,#27125,
#27126,#27127,#27128,#27129,#27130,#27131,#27132,#27133,#27134,#27135,#27136,
#27137,#27138,#27139,#27140,#27141,#27142,#27143,#27144,#27145,#27146,#27147,
#27148,#27149,#27150,#27151,#27152,#27153,#27154,#27155,#27156,#27157,#27158,
#27159,#27160,#27161,#27162,#27163,#27164,#27165),.UNSPECIFIED.,.F.,.F.)
B_SPLINE_CURVE_WITH_KNOTS((6,1,1,1,1,1,1,1,1,1,1,1,1,1,1,1,1,1,1,1,1,1,
1,1,1,1,1,1,1,1,1,1,1,1,1,1,1,1,1,1,1,1,1,1,1,1,1,1,1,1,1,1,1,1,1,1,1,1,
1,1,1,1,1,1,1,6),(0.,0.0153846153846154,0.0307692307692308,0.0461538461538462,
0.0615384615384615,0.0769230769230769,0.0923076923076923,0.107692307692308,
0.123076923076923,0.138461538461538,0.153846153846154,0.169230769230769,
0.184615384615385,0.2,0.215384615384615,0.230769230769231,0.246153846153846,
0.261538461538462,0.276923076923077,0.292307692307692,0.307692307692308,
0.323076923076923,0.338461538461538,0.353846153846154,0.369230769230769,
0.384615384615385,0.4,0.415384615384615,0.430769230769231,0.446153846153846,
0.461538461538462,0.476923076923077,0.492307692307692,0.507692307692308,
0.523076923076923,0.538461538461538,0.553846153846154,0.569230769230769,
0.584615384615384,0.6,0.615384615384615,0.63076923076923,0.646153846153846,
0.661538461538461,0.676923076923076,0.692307692307692,0.707692307692307,
0.723076923076922,0.738461538461538,0.753846153846153,0.769230769230768,
0.784615384615384,0.799999999999999,0.815384615384614,0.83076923076923,
0.846153846153845,0.86153846153846,0.876923076923076,0.892307692307691,
0.907692307692306,0.923076923076922,0.938461538461537,0.953846153846152,
0.969230769230768,0.984615384615383,1.),.UNSPECIFIED.)
CURVE()
GEOMETRIC_REPRESENTATION_ITEM()
RATIONAL_B_SPLINE_CURVE((1.,1.,1.,1.,1.,1.,1.,1.,1.,1.,1.,1.,1.,1.,1.,1.,
1.,1.,1.,1.,1.,1.,1.,1.,1.,1.,1.,1.,1.,1.,1.,1.,1.,1.,1.,1.,1.,1.,1.,1.,
1.,1.,1.,1.,1.,1.,1.,1.,1.,1.,1.,1.,1.,1.,1.,1.,1.,1.,1.,1.,1.,1.,1.,1.,
1.,1.,1.,1.,1.,1.))
REPRESENTATION_ITEM('')
);
#136=(
BOUNDED_CURVE()
B_SPLINE_CURVE(5,(#27169,#27170,#27171,#27172,#27173,#27174,#27175,#27176,
#27177,#27178,#27179,#27180,#27181,#27182,#27183,#27184,#27185,#27186,#27187,
#27188,#27189,#27190,#27191,#27192,#27193,#27194,#27195,#27196,#27197,#27198,
#27199,#27200,#27201,#27202,#27203,#27204,#27205,#27206,#27207,#27208,#27209,
#27210,#27211,#27212,#27213,#27214,#27215,#27216,#27217,#27218,#27219,#27220,
#27221,#27222,#27223,#27224,#27225,#27226,#27227,#27228,#27229,#27230,#27231,
#27232,#27233,#27234,#27235,#27236,#27237,#27238),.UNSPECIFIED.,.F.,.F.)
B_SPLINE_CURVE_WITH_KNOTS((6,1,1,1,1,1,1,1,1,1,1,1,1,1,1,1,1,1,1,1,1,1,
1,1,1,1,1,1,1,1,1,1,1,1,1,1,1,1,1,1,1,1,1,1,1,1,1,1,1,1,1,1,1,1,1,1,1,1,
1,1,1,1,1,1,1,6),(0.,0.0153846153846154,0.0307692307692308,0.0461538461538462,
0.0615384615384615,0.0769230769230769,0.0923076923076923,0.107692307692308,
0.123076923076923,0.138461538461538,0.153846153846154,0.169230769230769,
0.184615384615385,0.2,0.215384615384615,0.230769230769231,0.246153846153846,
0.261538461538462,0.276923076923077,0.292307692307692,0.307692307692308,
0.323076923076923,0.338461538461538,0.353846153846154,0.369230769230769,
0.384615384615385,0.4,0.415384615384615,0.430769230769231,0.446153846153846,
0.461538461538462,0.476923076923077,0.492307692307692,0.507692307692308,
0.523076923076923,0.538461538461538,0.553846153846154,0.569230769230769,
0.584615384615384,0.6,0.615384615384615,0.63076923076923,0.646153846153846,
0.661538461538461,0.676923076923076,0.692307692307692,0.707692307692307,
0.723076923076922,0.738461538461538,0.753846153846153,0.769230769230768,
0.784615384615384,0.799999999999999,0.815384615384614,0.83076923076923,
0.846153846153845,0.86153846153846,0.876923076923076,0.892307692307691,
0.907692307692306,0.923076923076922,0.938461538461537,0.953846153846152,
0.969230769230768,0.984615384615383,1.),.UNSPECIFIED.)
CURVE()
GEOMETRIC_REPRESENTATION_ITEM()
RATIONAL_B_SPLINE_CURVE((1.,1.,1.,1.,1.,1.,1.,1.,1.,1.,1.,1.,1.,1.,1.,1.,
1.,1.,1.,1.,1.,1.,1.,1.,1.,1.,1.,1.,1.,1.,1.,1.,1.,1.,1.,1.,1.,1.,1.,1.,
1.,1.,1.,1.,1.,1.,1.,1.,1.,1.,1.,1.,1.,1.,1.,1.,1.,1.,1.,1.,1.,1.,1.,1.,
1.,1.,1.,1.,1.,1.))
REPRESENTATION_ITEM('')
);
#137=(
BOUNDED_CURVE()
B_SPLINE_CURVE(5,(#27242,#27243,#27244,#27245,#27246,#27247,#27248,#27249,
#27250,#27251,#27252,#27253,#27254,#27255,#27256,#27257,#27258,#27259,#27260,
#27261,#27262,#27263,#27264,#27265,#27266,#27267,#27268,#27269,#27270,#27271,
#27272,#27273,#27274,#27275,#27276,#27277,#27278,#27279,#27280,#27281,#27282,
#27283,#27284,#27285,#27286,#27287,#27288,#27289,#27290,#27291,#27292,#27293,
#27294,#27295,#27296,#27297,#27298,#27299,#27300,#27301,#27302,#27303,#27304,
#27305,#27306,#27307,#27308,#27309,#27310,#27311),.UNSPECIFIED.,.F.,.F.)
B_SPLINE_CURVE_WITH_KNOTS((6,1,1,1,1,1,1,1,1,1,1,1,1,1,1,1,1,1,1,1,1,1,
1,1,1,1,1,1,1,1,1,1,1,1,1,1,1,1,1,1,1,1,1,1,1,1,1,1,1,1,1,1,1,1,1,1,1,1,
1,1,1,1,1,1,1,6),(0.,0.0153846153846154,0.0307692307692308,0.0461538461538462,
0.0615384615384615,0.0769230769230769,0.0923076923076923,0.107692307692308,
0.123076923076923,0.138461538461538,0.153846153846154,0.169230769230769,
0.184615384615385,0.2,0.215384615384615,0.230769230769231,0.246153846153846,
0.261538461538462,0.276923076923077,0.292307692307692,0.307692307692308,
0.323076923076923,0.338461538461538,0.353846153846154,0.369230769230769,
0.384615384615385,0.4,0.415384615384615,0.430769230769231,0.446153846153846,
0.461538461538462,0.476923076923077,0.492307692307692,0.507692307692308,
0.523076923076923,0.538461538461538,0.553846153846154,0.569230769230769,
0.584615384615384,0.6,0.615384615384615,0.63076923076923,0.646153846153846,
0.661538461538461,0.676923076923076,0.692307692307692,0.707692307692307,
0.723076923076922,0.738461538461538,0.753846153846153,0.769230769230768,
0.784615384615384,0.799999999999999,0.815384615384614,0.83076923076923,
0.846153846153845,0.86153846153846,0.876923076923076,0.892307692307691,
0.907692307692306,0.923076923076922,0.938461538461537,0.953846153846152,
0.969230769230768,0.984615384615383,1.),.UNSPECIFIED.)
CURVE()
GEOMETRIC_REPRESENTATION_ITEM()
RATIONAL_B_SPLINE_CURVE((1.,1.,1.,1.,1.,1.,1.,1.,1.,1.,1.,1.,1.,1.,1.,1.,
1.,1.,1.,1.,1.,1.,1.,1.,1.,1.,1.,1.,1.,1.,1.,1.,1.,1.,1.,1.,1.,1.,1.,1.,
1.,1.,1.,1.,1.,1.,1.,1.,1.,1.,1.,1.,1.,1.,1.,1.,1.,1.,1.,1.,1.,1.,1.,1.,
1.,1.,1.,1.,1.,1.))
REPRESENTATION_ITEM('')
);
#138=(
BOUNDED_CURVE()
B_SPLINE_CURVE(5,(#27315,#27316,#27317,#27318,#27319,#27320,#27321,#27322,
#27323,#27324,#27325,#27326,#27327,#27328,#27329,#27330,#27331,#27332,#27333,
#27334,#27335,#27336,#27337,#27338,#27339,#27340,#27341,#27342,#27343,#27344,
#27345,#27346,#27347,#27348,#27349,#27350,#27351,#27352,#27353,#27354,#27355,
#27356,#27357,#27358,#27359,#27360,#27361,#27362,#27363,#27364,#27365,#27366,
#27367,#27368,#27369,#27370,#27371,#27372,#27373,#27374,#27375,#27376,#27377,
#27378,#27379,#27380,#27381,#27382,#27383,#27384),.UNSPECIFIED.,.F.,.F.)
B_SPLINE_CURVE_WITH_KNOTS((6,1,1,1,1,1,1,1,1,1,1,1,1,1,1,1,1,1,1,1,1,1,
1,1,1,1,1,1,1,1,1,1,1,1,1,1,1,1,1,1,1,1,1,1,1,1,1,1,1,1,1,1,1,1,1,1,1,1,
1,1,1,1,1,1,1,6),(0.,0.0153846153846154,0.0307692307692308,0.0461538461538462,
0.0615384615384615,0.0769230769230769,0.0923076923076923,0.107692307692308,
0.123076923076923,0.138461538461538,0.153846153846154,0.169230769230769,
0.184615384615385,0.2,0.215384615384615,0.230769230769231,0.246153846153846,
0.261538461538462,0.276923076923077,0.292307692307692,0.307692307692308,
0.323076923076923,0.338461538461538,0.353846153846154,0.369230769230769,
0.384615384615385,0.4,0.415384615384615,0.430769230769231,0.446153846153846,
0.461538461538462,0.476923076923077,0.492307692307692,0.507692307692308,
0.523076923076923,0.538461538461538,0.553846153846154,0.569230769230769,
0.584615384615384,0.6,0.615384615384615,0.63076923076923,0.646153846153846,
0.661538461538461,0.676923076923076,0.692307692307692,0.707692307692307,
0.723076923076922,0.738461538461538,0.753846153846153,0.769230769230768,
0.784615384615384,0.799999999999999,0.815384615384614,0.83076923076923,
0.846153846153845,0.86153846153846,0.876923076923076,0.892307692307691,
0.907692307692306,0.923076923076922,0.938461538461537,0.953846153846152,
0.969230769230768,0.984615384615383,1.),.UNSPECIFIED.)
CURVE()
GEOMETRIC_REPRESENTATION_ITEM()
RATIONAL_B_SPLINE_CURVE((1.,1.,1.,1.,1.,1.,1.,1.,1.,1.,1.,1.,1.,1.,1.,1.,
1.,1.,1.,1.,1.,1.,1.,1.,1.,1.,1.,1.,1.,1.,1.,1.,1.,1.,1.,1.,1.,1.,1.,1.,
1.,1.,1.,1.,1.,1.,1.,1.,1.,1.,1.,1.,1.,1.,1.,1.,1.,1.,1.,1.,1.,1.,1.,1.,
1.,1.,1.,1.,1.,1.))
REPRESENTATION_ITEM('')
);
#139=(
BOUNDED_CURVE()
B_SPLINE_CURVE(5,(#27388,#27389,#27390,#27391,#27392,#27393,#27394,#27395,
#27396,#27397,#27398,#27399,#27400,#27401,#27402,#27403,#27404,#27405,#27406,
#27407,#27408,#27409,#27410,#27411,#27412,#27413,#27414,#27415,#27416,#27417,
#27418,#27419,#27420,#27421,#27422,#27423,#27424,#27425,#27426,#27427,#27428,
#27429,#27430,#27431,#27432,#27433,#27434,#27435,#27436,#27437,#27438,#27439,
#27440,#27441,#27442,#27443,#27444,#27445,#27446,#27447,#27448,#27449,#27450,
#27451,#27452,#27453,#27454,#27455,#27456,#27457),.UNSPECIFIED.,.F.,.F.)
B_SPLINE_CURVE_WITH_KNOTS((6,1,1,1,1,1,1,1,1,1,1,1,1,1,1,1,1,1,1,1,1,1,
1,1,1,1,1,1,1,1,1,1,1,1,1,1,1,1,1,1,1,1,1,1,1,1,1,1,1,1,1,1,1,1,1,1,1,1,
1,1,1,1,1,1,1,6),(0.,0.0153846153846154,0.0307692307692308,0.0461538461538462,
0.0615384615384615,0.0769230769230769,0.0923076923076923,0.107692307692308,
0.123076923076923,0.138461538461538,0.153846153846154,0.169230769230769,
0.184615384615385,0.2,0.215384615384615,0.230769230769231,0.246153846153846,
0.261538461538462,0.276923076923077,0.292307692307692,0.307692307692308,
0.323076923076923,0.338461538461538,0.353846153846154,0.369230769230769,
0.384615384615385,0.4,0.415384615384615,0.430769230769231,0.446153846153846,
0.461538461538462,0.476923076923077,0.492307692307692,0.507692307692308,
0.523076923076923,0.538461538461538,0.553846153846154,0.569230769230769,
0.584615384615384,0.6,0.615384615384615,0.63076923076923,0.646153846153846,
0.661538461538461,0.676923076923076,0.692307692307692,0.707692307692307,
0.723076923076922,0.738461538461538,0.753846153846153,0.769230769230768,
0.784615384615384,0.799999999999999,0.815384615384614,0.83076923076923,
0.846153846153845,0.86153846153846,0.876923076923076,0.892307692307691,
0.907692307692306,0.923076923076922,0.938461538461537,0.953846153846152,
0.969230769230768,0.984615384615383,1.),.UNSPECIFIED.)
CURVE()
GEOMETRIC_REPRESENTATION_ITEM()
RATIONAL_B_SPLINE_CURVE((1.,1.,1.,1.,1.,1.,1.,1.,1.,1.,1.,1.,1.,1.,1.,1.,
1.,1.,1.,1.,1.,1.,1.,1.,1.,1.,1.,1.,1.,1.,1.,1.,1.,1.,1.,1.,1.,1.,1.,1.,
1.,1.,1.,1.,1.,1.,1.,1.,1.,1.,1.,1.,1.,1.,1.,1.,1.,1.,1.,1.,1.,1.,1.,1.,
1.,1.,1.,1.,1.,1.))
REPRESENTATION_ITEM('')
);
#140=(
BOUNDED_CURVE()
B_SPLINE_CURVE(5,(#27461,#27462,#27463,#27464,#27465,#27466,#27467,#27468,
#27469,#27470,#27471,#27472,#27473,#27474,#27475,#27476,#27477,#27478,#27479,
#27480,#27481,#27482,#27483,#27484,#27485,#27486,#27487,#27488,#27489,#27490,
#27491,#27492,#27493,#27494,#27495,#27496,#27497,#27498,#27499,#27500,#27501,
#27502,#27503,#27504,#27505,#27506,#27507,#27508,#27509,#27510,#27511,#27512,
#27513,#27514,#27515,#27516,#27517,#27518,#27519,#27520,#27521,#27522,#27523,
#27524,#27525,#27526,#27527,#27528,#27529,#27530),.UNSPECIFIED.,.F.,.F.)
B_SPLINE_CURVE_WITH_KNOTS((6,1,1,1,1,1,1,1,1,1,1,1,1,1,1,1,1,1,1,1,1,1,
1,1,1,1,1,1,1,1,1,1,1,1,1,1,1,1,1,1,1,1,1,1,1,1,1,1,1,1,1,1,1,1,1,1,1,1,
1,1,1,1,1,1,1,6),(0.,0.0153846153846154,0.0307692307692308,0.0461538461538462,
0.0615384615384615,0.0769230769230769,0.0923076923076923,0.107692307692308,
0.123076923076923,0.138461538461538,0.153846153846154,0.169230769230769,
0.184615384615385,0.2,0.215384615384615,0.230769230769231,0.246153846153846,
0.261538461538462,0.276923076923077,0.292307692307692,0.307692307692308,
0.323076923076923,0.338461538461538,0.353846153846154,0.369230769230769,
0.384615384615385,0.4,0.415384615384615,0.430769230769231,0.446153846153846,
0.461538461538462,0.476923076923077,0.492307692307692,0.507692307692308,
0.523076923076923,0.538461538461538,0.553846153846154,0.569230769230769,
0.584615384615384,0.6,0.615384615384615,0.63076923076923,0.646153846153846,
0.661538461538461,0.676923076923076,0.692307692307692,0.707692307692307,
0.723076923076922,0.738461538461538,0.753846153846153,0.769230769230768,
0.784615384615384,0.799999999999999,0.815384615384614,0.83076923076923,
0.846153846153845,0.86153846153846,0.876923076923076,0.892307692307691,
0.907692307692306,0.923076923076922,0.938461538461537,0.953846153846152,
0.969230769230768,0.984615384615383,1.),.UNSPECIFIED.)
CURVE()
GEOMETRIC_REPRESENTATION_ITEM()
RATIONAL_B_SPLINE_CURVE((1.,1.,1.,1.,1.,1.,1.,1.,1.,1.,1.,1.,1.,1.,1.,1.,
1.,1.,1.,1.,1.,1.,1.,1.,1.,1.,1.,1.,1.,1.,1.,1.,1.,1.,1.,1.,1.,1.,1.,1.,
1.,1.,1.,1.,1.,1.,1.,1.,1.,1.,1.,1.,1.,1.,1.,1.,1.,1.,1.,1.,1.,1.,1.,1.,
1.,1.,1.,1.,1.,1.))
REPRESENTATION_ITEM('')
);
#141=(
BOUNDED_CURVE()
B_SPLINE_CURVE(5,(#27534,#27535,#27536,#27537,#27538,#27539,#27540,#27541,
#27542,#27543,#27544,#27545,#27546,#27547,#27548,#27549,#27550,#27551,#27552,
#27553,#27554,#27555,#27556,#27557,#27558,#27559,#27560,#27561,#27562,#27563,
#27564,#27565,#27566,#27567,#27568,#27569,#27570,#27571,#27572,#27573,#27574,
#27575,#27576,#27577,#27578,#27579,#27580,#27581,#27582,#27583,#27584,#27585,
#27586,#27587,#27588,#27589,#27590,#27591,#27592,#27593,#27594,#27595,#27596,
#27597,#27598,#27599,#27600,#27601,#27602,#27603),.UNSPECIFIED.,.F.,.F.)
B_SPLINE_CURVE_WITH_KNOTS((6,1,1,1,1,1,1,1,1,1,1,1,1,1,1,1,1,1,1,1,1,1,
1,1,1,1,1,1,1,1,1,1,1,1,1,1,1,1,1,1,1,1,1,1,1,1,1,1,1,1,1,1,1,1,1,1,1,1,
1,1,1,1,1,1,1,6),(0.,0.0153846153846154,0.0307692307692308,0.0461538461538462,
0.0615384615384615,0.0769230769230769,0.0923076923076923,0.107692307692308,
0.123076923076923,0.138461538461538,0.153846153846154,0.169230769230769,
0.184615384615385,0.2,0.215384615384615,0.230769230769231,0.246153846153846,
0.261538461538462,0.276923076923077,0.292307692307692,0.307692307692308,
0.323076923076923,0.338461538461538,0.353846153846154,0.369230769230769,
0.384615384615385,0.4,0.415384615384615,0.430769230769231,0.446153846153846,
0.461538461538462,0.476923076923077,0.492307692307692,0.507692307692308,
0.523076923076923,0.538461538461538,0.553846153846154,0.569230769230769,
0.584615384615384,0.6,0.615384615384615,0.63076923076923,0.646153846153846,
0.661538461538461,0.676923076923076,0.692307692307692,0.707692307692307,
0.723076923076922,0.738461538461538,0.753846153846153,0.769230769230768,
0.784615384615384,0.799999999999999,0.815384615384614,0.83076923076923,
0.846153846153845,0.86153846153846,0.876923076923076,0.892307692307691,
0.907692307692306,0.923076923076922,0.938461538461537,0.953846153846152,
0.969230769230768,0.984615384615383,1.),.UNSPECIFIED.)
CURVE()
GEOMETRIC_REPRESENTATION_ITEM()
RATIONAL_B_SPLINE_CURVE((1.,1.,1.,1.,1.,1.,1.,1.,1.,1.,1.,1.,1.,1.,1.,1.,
1.,1.,1.,1.,1.,1.,1.,1.,1.,1.,1.,1.,1.,1.,1.,1.,1.,1.,1.,1.,1.,1.,1.,1.,
1.,1.,1.,1.,1.,1.,1.,1.,1.,1.,1.,1.,1.,1.,1.,1.,1.,1.,1.,1.,1.,1.,1.,1.,
1.,1.,1.,1.,1.,1.))
REPRESENTATION_ITEM('')
);
#142=(
BOUNDED_CURVE()
B_SPLINE_CURVE(5,(#27607,#27608,#27609,#27610,#27611,#27612,#27613,#27614,
#27615,#27616,#27617,#27618,#27619,#27620,#27621,#27622,#27623,#27624,#27625,
#27626,#27627,#27628,#27629,#27630,#27631,#27632,#27633,#27634,#27635,#27636,
#27637,#27638,#27639,#27640,#27641,#27642,#27643,#27644,#27645,#27646,#27647,
#27648,#27649,#27650,#27651,#27652,#27653,#27654,#27655,#27656,#27657,#27658,
#27659,#27660,#27661,#27662,#27663,#27664,#27665,#27666,#27667,#27668,#27669,
#27670,#27671,#27672,#27673,#27674,#27675,#27676),.UNSPECIFIED.,.F.,.F.)
B_SPLINE_CURVE_WITH_KNOTS((6,1,1,1,1,1,1,1,1,1,1,1,1,1,1,1,1,1,1,1,1,1,
1,1,1,1,1,1,1,1,1,1,1,1,1,1,1,1,1,1,1,1,1,1,1,1,1,1,1,1,1,1,1,1,1,1,1,1,
1,1,1,1,1,1,1,6),(0.,0.0153846153846154,0.0307692307692308,0.0461538461538462,
0.0615384615384615,0.0769230769230769,0.0923076923076923,0.107692307692308,
0.123076923076923,0.138461538461538,0.153846153846154,0.169230769230769,
0.184615384615385,0.2,0.215384615384615,0.230769230769231,0.246153846153846,
0.261538461538462,0.276923076923077,0.292307692307692,0.307692307692308,
0.323076923076923,0.338461538461538,0.353846153846154,0.369230769230769,
0.384615384615385,0.4,0.415384615384615,0.430769230769231,0.446153846153846,
0.461538461538462,0.476923076923077,0.492307692307692,0.507692307692308,
0.523076923076923,0.538461538461538,0.553846153846154,0.569230769230769,
0.584615384615384,0.6,0.615384615384615,0.63076923076923,0.646153846153846,
0.661538461538461,0.676923076923076,0.692307692307692,0.707692307692307,
0.723076923076922,0.738461538461538,0.753846153846153,0.769230769230768,
0.784615384615384,0.799999999999999,0.815384615384614,0.83076923076923,
0.846153846153845,0.86153846153846,0.876923076923076,0.892307692307691,
0.907692307692306,0.923076923076922,0.938461538461537,0.953846153846152,
0.969230769230768,0.984615384615383,1.),.UNSPECIFIED.)
CURVE()
GEOMETRIC_REPRESENTATION_ITEM()
RATIONAL_B_SPLINE_CURVE((1.,1.,1.,1.,1.,1.,1.,1.,1.,1.,1.,1.,1.,1.,1.,1.,
1.,1.,1.,1.,1.,1.,1.,1.,1.,1.,1.,1.,1.,1.,1.,1.,1.,1.,1.,1.,1.,1.,1.,1.,
1.,1.,1.,1.,1.,1.,1.,1.,1.,1.,1.,1.,1.,1.,1.,1.,1.,1.,1.,1.,1.,1.,1.,1.,
1.,1.,1.,1.,1.,1.))
REPRESENTATION_ITEM('')
);
#143=(
BOUNDED_CURVE()
B_SPLINE_CURVE(5,(#27680,#27681,#27682,#27683,#27684,#27685,#27686,#27687,
#27688,#27689,#27690,#27691,#27692,#27693,#27694,#27695,#27696,#27697,#27698,
#27699,#27700,#27701,#27702,#27703,#27704,#27705,#27706,#27707,#27708,#27709,
#27710,#27711,#27712,#27713,#27714,#27715,#27716,#27717,#27718,#27719,#27720,
#27721,#27722,#27723,#27724,#27725,#27726,#27727,#27728,#27729,#27730,#27731,
#27732,#27733,#27734,#27735,#27736,#27737,#27738,#27739,#27740,#27741,#27742,
#27743,#27744,#27745,#27746,#27747,#27748,#27749),.UNSPECIFIED.,.F.,.F.)
B_SPLINE_CURVE_WITH_KNOTS((6,1,1,1,1,1,1,1,1,1,1,1,1,1,1,1,1,1,1,1,1,1,
1,1,1,1,1,1,1,1,1,1,1,1,1,1,1,1,1,1,1,1,1,1,1,1,1,1,1,1,1,1,1,1,1,1,1,1,
1,1,1,1,1,1,1,6),(0.,0.0153846153846154,0.0307692307692308,0.0461538461538462,
0.0615384615384615,0.0769230769230769,0.0923076923076923,0.107692307692308,
0.123076923076923,0.138461538461538,0.153846153846154,0.169230769230769,
0.184615384615385,0.2,0.215384615384615,0.230769230769231,0.246153846153846,
0.261538461538462,0.276923076923077,0.292307692307692,0.307692307692308,
0.323076923076923,0.338461538461538,0.353846153846154,0.369230769230769,
0.384615384615385,0.4,0.415384615384615,0.430769230769231,0.446153846153846,
0.461538461538462,0.476923076923077,0.492307692307692,0.507692307692308,
0.523076923076923,0.538461538461538,0.553846153846154,0.569230769230769,
0.584615384615384,0.6,0.615384615384615,0.63076923076923,0.646153846153846,
0.661538461538461,0.676923076923076,0.692307692307692,0.707692307692307,
0.723076923076922,0.738461538461538,0.753846153846153,0.769230769230768,
0.784615384615384,0.799999999999999,0.815384615384614,0.83076923076923,
0.846153846153845,0.86153846153846,0.876923076923076,0.892307692307691,
0.907692307692306,0.923076923076922,0.938461538461537,0.953846153846152,
0.969230769230768,0.984615384615383,1.),.UNSPECIFIED.)
CURVE()
GEOMETRIC_REPRESENTATION_ITEM()
RATIONAL_B_SPLINE_CURVE((1.,1.,1.,1.,1.,1.,1.,1.,1.,1.,1.,1.,1.,1.,1.,1.,
1.,1.,1.,1.,1.,1.,1.,1.,1.,1.,1.,1.,1.,1.,1.,1.,1.,1.,1.,1.,1.,1.,1.,1.,
1.,1.,1.,1.,1.,1.,1.,1.,1.,1.,1.,1.,1.,1.,1.,1.,1.,1.,1.,1.,1.,1.,1.,1.,
1.,1.,1.,1.,1.,1.))
REPRESENTATION_ITEM('')
);
#144=(
BOUNDED_CURVE()
B_SPLINE_CURVE(5,(#27753,#27754,#27755,#27756,#27757,#27758,#27759,#27760,
#27761,#27762,#27763,#27764,#27765,#27766,#27767,#27768,#27769,#27770,#27771,
#27772,#27773,#27774,#27775,#27776,#27777,#27778,#27779,#27780,#27781,#27782,
#27783,#27784,#27785,#27786,#27787,#27788,#27789,#27790,#27791,#27792,#27793,
#27794,#27795,#27796,#27797,#27798,#27799,#27800,#27801,#27802,#27803,#27804,
#27805,#27806,#27807,#27808,#27809,#27810,#27811,#27812,#27813,#27814,#27815,
#27816,#27817,#27818,#27819,#27820,#27821,#27822),.UNSPECIFIED.,.F.,.F.)
B_SPLINE_CURVE_WITH_KNOTS((6,1,1,1,1,1,1,1,1,1,1,1,1,1,1,1,1,1,1,1,1,1,
1,1,1,1,1,1,1,1,1,1,1,1,1,1,1,1,1,1,1,1,1,1,1,1,1,1,1,1,1,1,1,1,1,1,1,1,
1,1,1,1,1,1,1,6),(0.,0.0153846153846154,0.0307692307692308,0.0461538461538462,
0.0615384615384615,0.0769230769230769,0.0923076923076923,0.107692307692308,
0.123076923076923,0.138461538461538,0.153846153846154,0.169230769230769,
0.184615384615385,0.2,0.215384615384615,0.230769230769231,0.246153846153846,
0.261538461538462,0.276923076923077,0.292307692307692,0.307692307692308,
0.323076923076923,0.338461538461538,0.353846153846154,0.369230769230769,
0.384615384615385,0.4,0.415384615384615,0.430769230769231,0.446153846153846,
0.461538461538462,0.476923076923077,0.492307692307692,0.507692307692308,
0.523076923076923,0.538461538461538,0.553846153846154,0.569230769230769,
0.584615384615384,0.6,0.615384615384615,0.63076923076923,0.646153846153846,
0.661538461538461,0.676923076923076,0.692307692307692,0.707692307692307,
0.723076923076922,0.738461538461538,0.753846153846153,0.769230769230768,
0.784615384615384,0.799999999999999,0.815384615384614,0.83076923076923,
0.846153846153845,0.86153846153846,0.876923076923076,0.892307692307691,
0.907692307692306,0.923076923076922,0.938461538461537,0.953846153846152,
0.969230769230768,0.984615384615383,1.),.UNSPECIFIED.)
CURVE()
GEOMETRIC_REPRESENTATION_ITEM()
RATIONAL_B_SPLINE_CURVE((1.,1.,1.,1.,1.,1.,1.,1.,1.,1.,1.,1.,1.,1.,1.,1.,
1.,1.,1.,1.,1.,1.,1.,1.,1.,1.,1.,1.,1.,1.,1.,1.,1.,1.,1.,1.,1.,1.,1.,1.,
1.,1.,1.,1.,1.,1.,1.,1.,1.,1.,1.,1.,1.,1.,1.,1.,1.,1.,1.,1.,1.,1.,1.,1.,
1.,1.,1.,1.,1.,1.))
REPRESENTATION_ITEM('')
);
#145=(
BOUNDED_CURVE()
B_SPLINE_CURVE(5,(#27826,#27827,#27828,#27829,#27830,#27831,#27832,#27833,
#27834,#27835,#27836,#27837,#27838,#27839,#27840,#27841,#27842,#27843,#27844,
#27845,#27846,#27847,#27848,#27849,#27850,#27851,#27852,#27853,#27854,#27855,
#27856,#27857,#27858,#27859,#27860,#27861,#27862,#27863,#27864,#27865,#27866,
#27867,#27868,#27869,#27870,#27871,#27872,#27873,#27874,#27875,#27876,#27877,
#27878,#27879,#27880,#27881,#27882,#27883,#27884,#27885,#27886,#27887,#27888,
#27889,#27890,#27891,#27892,#27893,#27894,#27895),.UNSPECIFIED.,.F.,.F.)
B_SPLINE_CURVE_WITH_KNOTS((6,1,1,1,1,1,1,1,1,1,1,1,1,1,1,1,1,1,1,1,1,1,
1,1,1,1,1,1,1,1,1,1,1,1,1,1,1,1,1,1,1,1,1,1,1,1,1,1,1,1,1,1,1,1,1,1,1,1,
1,1,1,1,1,1,1,6),(0.,0.0153846153846154,0.0307692307692308,0.0461538461538462,
0.0615384615384615,0.0769230769230769,0.0923076923076923,0.107692307692308,
0.123076923076923,0.138461538461538,0.153846153846154,0.169230769230769,
0.184615384615385,0.2,0.215384615384615,0.230769230769231,0.246153846153846,
0.261538461538462,0.276923076923077,0.292307692307692,0.307692307692308,
0.323076923076923,0.338461538461538,0.353846153846154,0.369230769230769,
0.384615384615385,0.4,0.415384615384615,0.430769230769231,0.446153846153846,
0.461538461538462,0.476923076923077,0.492307692307692,0.507692307692308,
0.523076923076923,0.538461538461538,0.553846153846154,0.569230769230769,
0.584615384615384,0.6,0.615384615384615,0.63076923076923,0.646153846153846,
0.661538461538461,0.676923076923076,0.692307692307692,0.707692307692307,
0.723076923076922,0.738461538461538,0.753846153846153,0.769230769230768,
0.784615384615384,0.799999999999999,0.815384615384614,0.83076923076923,
0.846153846153845,0.86153846153846,0.876923076923076,0.892307692307691,
0.907692307692306,0.923076923076922,0.938461538461537,0.953846153846152,
0.969230769230768,0.984615384615383,1.),.UNSPECIFIED.)
CURVE()
GEOMETRIC_REPRESENTATION_ITEM()
RATIONAL_B_SPLINE_CURVE((1.,1.,1.,1.,1.,1.,1.,1.,1.,1.,1.,1.,1.,1.,1.,1.,
1.,1.,1.,1.,1.,1.,1.,1.,1.,1.,1.,1.,1.,1.,1.,1.,1.,1.,1.,1.,1.,1.,1.,1.,
1.,1.,1.,1.,1.,1.,1.,1.,1.,1.,1.,1.,1.,1.,1.,1.,1.,1.,1.,1.,1.,1.,1.,1.,
1.,1.,1.,1.,1.,1.))
REPRESENTATION_ITEM('')
);
#146=(
BOUNDED_CURVE()
B_SPLINE_CURVE(5,(#27899,#27900,#27901,#27902,#27903,#27904,#27905,#27906,
#27907,#27908,#27909,#27910,#27911,#27912,#27913,#27914,#27915,#27916,#27917,
#27918,#27919,#27920,#27921,#27922,#27923,#27924,#27925,#27926,#27927,#27928,
#27929,#27930,#27931,#27932,#27933,#27934,#27935,#27936,#27937,#27938,#27939,
#27940,#27941,#27942,#27943,#27944,#27945,#27946,#27947,#27948,#27949,#27950,
#27951,#27952,#27953,#27954,#27955,#27956,#27957,#27958,#27959,#27960,#27961,
#27962,#27963,#27964,#27965,#27966,#27967,#27968),.UNSPECIFIED.,.F.,.F.)
B_SPLINE_CURVE_WITH_KNOTS((6,1,1,1,1,1,1,1,1,1,1,1,1,1,1,1,1,1,1,1,1,1,
1,1,1,1,1,1,1,1,1,1,1,1,1,1,1,1,1,1,1,1,1,1,1,1,1,1,1,1,1,1,1,1,1,1,1,1,
1,1,1,1,1,1,1,6),(0.,0.0153846153846154,0.0307692307692308,0.0461538461538462,
0.0615384615384615,0.0769230769230769,0.0923076923076923,0.107692307692308,
0.123076923076923,0.138461538461538,0.153846153846154,0.169230769230769,
0.184615384615385,0.2,0.215384615384615,0.230769230769231,0.246153846153846,
0.261538461538462,0.276923076923077,0.292307692307692,0.307692307692308,
0.323076923076923,0.338461538461538,0.353846153846154,0.369230769230769,
0.384615384615385,0.4,0.415384615384615,0.430769230769231,0.446153846153846,
0.461538461538462,0.476923076923077,0.492307692307692,0.507692307692308,
0.523076923076923,0.538461538461538,0.553846153846154,0.569230769230769,
0.584615384615384,0.6,0.615384615384615,0.63076923076923,0.646153846153846,
0.661538461538461,0.676923076923076,0.692307692307692,0.707692307692307,
0.723076923076922,0.738461538461538,0.753846153846153,0.769230769230768,
0.784615384615384,0.799999999999999,0.815384615384614,0.83076923076923,
0.846153846153845,0.86153846153846,0.876923076923076,0.892307692307691,
0.907692307692306,0.923076923076922,0.938461538461537,0.953846153846152,
0.969230769230768,0.984615384615383,1.),.UNSPECIFIED.)
CURVE()
GEOMETRIC_REPRESENTATION_ITEM()
RATIONAL_B_SPLINE_CURVE((1.,1.,1.,1.,1.,1.,1.,1.,1.,1.,1.,1.,1.,1.,1.,1.,
1.,1.,1.,1.,1.,1.,1.,1.,1.,1.,1.,1.,1.,1.,1.,1.,1.,1.,1.,1.,1.,1.,1.,1.,
1.,1.,1.,1.,1.,1.,1.,1.,1.,1.,1.,1.,1.,1.,1.,1.,1.,1.,1.,1.,1.,1.,1.,1.,
1.,1.,1.,1.,1.,1.))
REPRESENTATION_ITEM('')
);
#147=(
BOUNDED_CURVE()
B_SPLINE_CURVE(5,(#27972,#27973,#27974,#27975,#27976,#27977,#27978,#27979,
#27980,#27981,#27982,#27983,#27984,#27985,#27986,#27987,#27988,#27989,#27990,
#27991,#27992,#27993,#27994,#27995,#27996,#27997,#27998,#27999,#28000,#28001,
#28002,#28003,#28004,#28005,#28006,#28007,#28008,#28009,#28010,#28011,#28012,
#28013,#28014,#28015,#28016,#28017,#28018,#28019,#28020,#28021,#28022,#28023,
#28024,#28025,#28026,#28027,#28028,#28029,#28030,#28031,#28032,#28033,#28034,
#28035,#28036,#28037,#28038,#28039,#28040,#28041),.UNSPECIFIED.,.F.,.F.)
B_SPLINE_CURVE_WITH_KNOTS((6,1,1,1,1,1,1,1,1,1,1,1,1,1,1,1,1,1,1,1,1,1,
1,1,1,1,1,1,1,1,1,1,1,1,1,1,1,1,1,1,1,1,1,1,1,1,1,1,1,1,1,1,1,1,1,1,1,1,
1,1,1,1,1,1,1,6),(0.,0.0153846153846154,0.0307692307692308,0.0461538461538462,
0.0615384615384615,0.0769230769230769,0.0923076923076923,0.107692307692308,
0.123076923076923,0.138461538461538,0.153846153846154,0.169230769230769,
0.184615384615385,0.2,0.215384615384615,0.230769230769231,0.246153846153846,
0.261538461538462,0.276923076923077,0.292307692307692,0.307692307692308,
0.323076923076923,0.338461538461538,0.353846153846154,0.369230769230769,
0.384615384615385,0.4,0.415384615384615,0.430769230769231,0.446153846153846,
0.461538461538462,0.476923076923077,0.492307692307692,0.507692307692308,
0.523076923076923,0.538461538461538,0.553846153846154,0.569230769230769,
0.584615384615384,0.6,0.615384615384615,0.63076923076923,0.646153846153846,
0.661538461538461,0.676923076923076,0.692307692307692,0.707692307692307,
0.723076923076922,0.738461538461538,0.753846153846153,0.769230769230768,
0.784615384615384,0.799999999999999,0.815384615384614,0.83076923076923,
0.846153846153845,0.86153846153846,0.876923076923076,0.892307692307691,
0.907692307692306,0.923076923076922,0.938461538461537,0.953846153846152,
0.969230769230768,0.984615384615383,1.),.UNSPECIFIED.)
CURVE()
GEOMETRIC_REPRESENTATION_ITEM()
RATIONAL_B_SPLINE_CURVE((1.,1.,1.,1.,1.,1.,1.,1.,1.,1.,1.,1.,1.,1.,1.,1.,
1.,1.,1.,1.,1.,1.,1.,1.,1.,1.,1.,1.,1.,1.,1.,1.,1.,1.,1.,1.,1.,1.,1.,1.,
1.,1.,1.,1.,1.,1.,1.,1.,1.,1.,1.,1.,1.,1.,1.,1.,1.,1.,1.,1.,1.,1.,1.,1.,
1.,1.,1.,1.,1.,1.))
REPRESENTATION_ITEM('')
);
#148=(
BOUNDED_CURVE()
B_SPLINE_CURVE(5,(#28045,#28046,#28047,#28048,#28049,#28050,#28051,#28052,
#28053,#28054,#28055,#28056,#28057,#28058,#28059,#28060,#28061,#28062,#28063,
#28064,#28065,#28066,#28067,#28068,#28069,#28070,#28071,#28072,#28073,#28074,
#28075,#28076,#28077,#28078,#28079,#28080,#28081,#28082,#28083,#28084,#28085,
#28086,#28087,#28088,#28089,#28090,#28091,#28092,#28093,#28094,#28095,#28096,
#28097,#28098,#28099,#28100,#28101,#28102,#28103,#28104,#28105,#28106,#28107,
#28108,#28109,#28110,#28111,#28112,#28113,#28114),.UNSPECIFIED.,.F.,.F.)
B_SPLINE_CURVE_WITH_KNOTS((6,1,1,1,1,1,1,1,1,1,1,1,1,1,1,1,1,1,1,1,1,1,
1,1,1,1,1,1,1,1,1,1,1,1,1,1,1,1,1,1,1,1,1,1,1,1,1,1,1,1,1,1,1,1,1,1,1,1,
1,1,1,1,1,1,1,6),(0.,0.0153846153846154,0.0307692307692308,0.0461538461538462,
0.0615384615384615,0.0769230769230769,0.0923076923076923,0.107692307692308,
0.123076923076923,0.138461538461538,0.153846153846154,0.169230769230769,
0.184615384615385,0.2,0.215384615384615,0.230769230769231,0.246153846153846,
0.261538461538462,0.276923076923077,0.292307692307692,0.307692307692308,
0.323076923076923,0.338461538461538,0.353846153846154,0.369230769230769,
0.384615384615385,0.4,0.415384615384615,0.430769230769231,0.446153846153846,
0.461538461538462,0.476923076923077,0.492307692307692,0.507692307692308,
0.523076923076923,0.538461538461538,0.553846153846154,0.569230769230769,
0.584615384615384,0.6,0.615384615384615,0.63076923076923,0.646153846153846,
0.661538461538461,0.676923076923076,0.692307692307692,0.707692307692307,
0.723076923076922,0.738461538461538,0.753846153846153,0.769230769230768,
0.784615384615384,0.799999999999999,0.815384615384614,0.83076923076923,
0.846153846153845,0.86153846153846,0.876923076923076,0.892307692307691,
0.907692307692306,0.923076923076922,0.938461538461537,0.953846153846152,
0.969230769230768,0.984615384615383,1.),.UNSPECIFIED.)
CURVE()
GEOMETRIC_REPRESENTATION_ITEM()
RATIONAL_B_SPLINE_CURVE((1.,1.,1.,1.,1.,1.,1.,1.,1.,1.,1.,1.,1.,1.,1.,1.,
1.,1.,1.,1.,1.,1.,1.,1.,1.,1.,1.,1.,1.,1.,1.,1.,1.,1.,1.,1.,1.,1.,1.,1.,
1.,1.,1.,1.,1.,1.,1.,1.,1.,1.,1.,1.,1.,1.,1.,1.,1.,1.,1.,1.,1.,1.,1.,1.,
1.,1.,1.,1.,1.,1.))
REPRESENTATION_ITEM('')
);
#149=(
BOUNDED_CURVE()
B_SPLINE_CURVE(5,(#28118,#28119,#28120,#28121,#28122,#28123,#28124,#28125,
#28126,#28127,#28128,#28129,#28130,#28131,#28132,#28133,#28134,#28135,#28136,
#28137,#28138,#28139,#28140,#28141,#28142,#28143,#28144,#28145,#28146,#28147,
#28148,#28149,#28150,#28151,#28152,#28153,#28154,#28155,#28156,#28157,#28158,
#28159,#28160,#28161,#28162,#28163,#28164,#28165,#28166,#28167,#28168,#28169,
#28170,#28171,#28172,#28173,#28174,#28175,#28176,#28177,#28178,#28179,#28180,
#28181,#28182,#28183,#28184,#28185,#28186,#28187),.UNSPECIFIED.,.F.,.F.)
B_SPLINE_CURVE_WITH_KNOTS((6,1,1,1,1,1,1,1,1,1,1,1,1,1,1,1,1,1,1,1,1,1,
1,1,1,1,1,1,1,1,1,1,1,1,1,1,1,1,1,1,1,1,1,1,1,1,1,1,1,1,1,1,1,1,1,1,1,1,
1,1,1,1,1,1,1,6),(0.,0.0153846153846154,0.0307692307692308,0.0461538461538462,
0.0615384615384615,0.0769230769230769,0.0923076923076923,0.107692307692308,
0.123076923076923,0.138461538461538,0.153846153846154,0.169230769230769,
0.184615384615385,0.2,0.215384615384615,0.230769230769231,0.246153846153846,
0.261538461538462,0.276923076923077,0.292307692307692,0.307692307692308,
0.323076923076923,0.338461538461538,0.353846153846154,0.369230769230769,
0.384615384615385,0.4,0.415384615384615,0.430769230769231,0.446153846153846,
0.461538461538462,0.476923076923077,0.492307692307692,0.507692307692308,
0.523076923076923,0.538461538461538,0.553846153846154,0.569230769230769,
0.584615384615384,0.6,0.615384615384615,0.63076923076923,0.646153846153846,
0.661538461538461,0.676923076923076,0.692307692307692,0.707692307692307,
0.723076923076922,0.738461538461538,0.753846153846153,0.769230769230768,
0.784615384615384,0.799999999999999,0.815384615384614,0.83076923076923,
0.846153846153845,0.86153846153846,0.876923076923076,0.892307692307691,
0.907692307692306,0.923076923076922,0.938461538461537,0.953846153846152,
0.969230769230768,0.984615384615383,1.),.UNSPECIFIED.)
CURVE()
GEOMETRIC_REPRESENTATION_ITEM()
RATIONAL_B_SPLINE_CURVE((1.,1.,1.,1.,1.,1.,1.,1.,1.,1.,1.,1.,1.,1.,1.,1.,
1.,1.,1.,1.,1.,1.,1.,1.,1.,1.,1.,1.,1.,1.,1.,1.,1.,1.,1.,1.,1.,1.,1.,1.,
1.,1.,1.,1.,1.,1.,1.,1.,1.,1.,1.,1.,1.,1.,1.,1.,1.,1.,1.,1.,1.,1.,1.,1.,
1.,1.,1.,1.,1.,1.))
REPRESENTATION_ITEM('')
);
#150=(
BOUNDED_CURVE()
B_SPLINE_CURVE(5,(#28191,#28192,#28193,#28194,#28195,#28196,#28197,#28198,
#28199,#28200,#28201,#28202,#28203,#28204,#28205,#28206,#28207,#28208,#28209,
#28210,#28211,#28212,#28213,#28214,#28215,#28216,#28217,#28218,#28219,#28220,
#28221,#28222,#28223,#28224,#28225,#28226,#28227,#28228,#28229,#28230,#28231,
#28232,#28233,#28234,#28235,#28236,#28237,#28238,#28239,#28240,#28241,#28242,
#28243,#28244,#28245,#28246,#28247,#28248,#28249,#28250,#28251,#28252,#28253,
#28254,#28255,#28256,#28257,#28258,#28259,#28260),.UNSPECIFIED.,.F.,.F.)
B_SPLINE_CURVE_WITH_KNOTS((6,1,1,1,1,1,1,1,1,1,1,1,1,1,1,1,1,1,1,1,1,1,
1,1,1,1,1,1,1,1,1,1,1,1,1,1,1,1,1,1,1,1,1,1,1,1,1,1,1,1,1,1,1,1,1,1,1,1,
1,1,1,1,1,1,1,6),(0.,0.0153846153846154,0.0307692307692308,0.0461538461538462,
0.0615384615384615,0.0769230769230769,0.0923076923076923,0.107692307692308,
0.123076923076923,0.138461538461538,0.153846153846154,0.169230769230769,
0.184615384615385,0.2,0.215384615384615,0.230769230769231,0.246153846153846,
0.261538461538462,0.276923076923077,0.292307692307692,0.307692307692308,
0.323076923076923,0.338461538461538,0.353846153846154,0.369230769230769,
0.384615384615385,0.4,0.415384615384615,0.430769230769231,0.446153846153846,
0.461538461538462,0.476923076923077,0.492307692307692,0.507692307692308,
0.523076923076923,0.538461538461538,0.553846153846154,0.569230769230769,
0.584615384615384,0.6,0.615384615384615,0.63076923076923,0.646153846153846,
0.661538461538461,0.676923076923076,0.692307692307692,0.707692307692307,
0.723076923076922,0.738461538461538,0.753846153846153,0.769230769230768,
0.784615384615384,0.799999999999999,0.815384615384614,0.83076923076923,
0.846153846153845,0.86153846153846,0.876923076923076,0.892307692307691,
0.907692307692306,0.923076923076922,0.938461538461537,0.953846153846152,
0.969230769230768,0.984615384615383,1.),.UNSPECIFIED.)
CURVE()
GEOMETRIC_REPRESENTATION_ITEM()
RATIONAL_B_SPLINE_CURVE((1.,1.,1.,1.,1.,1.,1.,1.,1.,1.,1.,1.,1.,1.,1.,1.,
1.,1.,1.,1.,1.,1.,1.,1.,1.,1.,1.,1.,1.,1.,1.,1.,1.,1.,1.,1.,1.,1.,1.,1.,
1.,1.,1.,1.,1.,1.,1.,1.,1.,1.,1.,1.,1.,1.,1.,1.,1.,1.,1.,1.,1.,1.,1.,1.,
1.,1.,1.,1.,1.,1.))
REPRESENTATION_ITEM('')
);
#151=(
BOUNDED_CURVE()
B_SPLINE_CURVE(5,(#28264,#28265,#28266,#28267,#28268,#28269,#28270,#28271,
#28272,#28273,#28274,#28275,#28276,#28277,#28278,#28279,#28280,#28281,#28282,
#28283,#28284,#28285,#28286,#28287,#28288,#28289,#28290,#28291,#28292,#28293,
#28294,#28295,#28296,#28297,#28298,#28299,#28300,#28301,#28302,#28303,#28304,
#28305,#28306,#28307,#28308,#28309,#28310,#28311,#28312,#28313,#28314,#28315,
#28316,#28317,#28318,#28319,#28320,#28321,#28322,#28323,#28324,#28325,#28326,
#28327,#28328,#28329,#28330,#28331,#28332,#28333),.UNSPECIFIED.,.F.,.F.)
B_SPLINE_CURVE_WITH_KNOTS((6,1,1,1,1,1,1,1,1,1,1,1,1,1,1,1,1,1,1,1,1,1,
1,1,1,1,1,1,1,1,1,1,1,1,1,1,1,1,1,1,1,1,1,1,1,1,1,1,1,1,1,1,1,1,1,1,1,1,
1,1,1,1,1,1,1,6),(0.,0.0153846153846154,0.0307692307692308,0.0461538461538462,
0.0615384615384615,0.0769230769230769,0.0923076923076923,0.107692307692308,
0.123076923076923,0.138461538461538,0.153846153846154,0.169230769230769,
0.184615384615385,0.2,0.215384615384615,0.230769230769231,0.246153846153846,
0.261538461538462,0.276923076923077,0.292307692307692,0.307692307692308,
0.323076923076923,0.338461538461538,0.353846153846154,0.369230769230769,
0.384615384615385,0.4,0.415384615384615,0.430769230769231,0.446153846153846,
0.461538461538462,0.476923076923077,0.492307692307692,0.507692307692308,
0.523076923076923,0.538461538461538,0.553846153846154,0.569230769230769,
0.584615384615384,0.6,0.615384615384615,0.63076923076923,0.646153846153846,
0.661538461538461,0.676923076923076,0.692307692307692,0.707692307692307,
0.723076923076922,0.738461538461538,0.753846153846153,0.769230769230768,
0.784615384615384,0.799999999999999,0.815384615384614,0.83076923076923,
0.846153846153845,0.86153846153846,0.876923076923076,0.892307692307691,
0.907692307692306,0.923076923076922,0.938461538461537,0.953846153846152,
0.969230769230768,0.984615384615383,1.),.UNSPECIFIED.)
CURVE()
GEOMETRIC_REPRESENTATION_ITEM()
RATIONAL_B_SPLINE_CURVE((1.,1.,1.,1.,1.,1.,1.,1.,1.,1.,1.,1.,1.,1.,1.,1.,
1.,1.,1.,1.,1.,1.,1.,1.,1.,1.,1.,1.,1.,1.,1.,1.,1.,1.,1.,1.,1.,1.,1.,1.,
1.,1.,1.,1.,1.,1.,1.,1.,1.,1.,1.,1.,1.,1.,1.,1.,1.,1.,1.,1.,1.,1.,1.,1.,
1.,1.,1.,1.,1.,1.))
REPRESENTATION_ITEM('')
);
#152=(
BOUNDED_CURVE()
B_SPLINE_CURVE(5,(#28337,#28338,#28339,#28340,#28341,#28342,#28343,#28344,
#28345,#28346,#28347,#28348,#28349,#28350,#28351,#28352,#28353,#28354,#28355,
#28356,#28357,#28358,#28359,#28360,#28361,#28362,#28363,#28364,#28365,#28366,
#28367,#28368,#28369,#28370,#28371,#28372,#28373,#28374,#28375,#28376,#28377,
#28378,#28379,#28380,#28381,#28382,#28383,#28384,#28385,#28386,#28387,#28388,
#28389,#28390,#28391,#28392,#28393,#28394,#28395,#28396,#28397,#28398,#28399,
#28400,#28401,#28402,#28403,#28404,#28405,#28406),.UNSPECIFIED.,.F.,.F.)
B_SPLINE_CURVE_WITH_KNOTS((6,1,1,1,1,1,1,1,1,1,1,1,1,1,1,1,1,1,1,1,1,1,
1,1,1,1,1,1,1,1,1,1,1,1,1,1,1,1,1,1,1,1,1,1,1,1,1,1,1,1,1,1,1,1,1,1,1,1,
1,1,1,1,1,1,1,6),(0.,0.0153846153846154,0.0307692307692308,0.0461538461538462,
0.0615384615384615,0.0769230769230769,0.0923076923076923,0.107692307692308,
0.123076923076923,0.138461538461538,0.153846153846154,0.169230769230769,
0.184615384615385,0.2,0.215384615384615,0.230769230769231,0.246153846153846,
0.261538461538462,0.276923076923077,0.292307692307692,0.307692307692308,
0.323076923076923,0.338461538461538,0.353846153846154,0.369230769230769,
0.384615384615385,0.4,0.415384615384615,0.430769230769231,0.446153846153846,
0.461538461538462,0.476923076923077,0.492307692307692,0.507692307692308,
0.523076923076923,0.538461538461538,0.553846153846154,0.569230769230769,
0.584615384615384,0.6,0.615384615384615,0.63076923076923,0.646153846153846,
0.661538461538461,0.676923076923076,0.692307692307692,0.707692307692307,
0.723076923076922,0.738461538461538,0.753846153846153,0.769230769230768,
0.784615384615384,0.799999999999999,0.815384615384614,0.83076923076923,
0.846153846153845,0.86153846153846,0.876923076923076,0.892307692307691,
0.907692307692306,0.923076923076922,0.938461538461537,0.953846153846152,
0.969230769230768,0.984615384615383,1.),.UNSPECIFIED.)
CURVE()
GEOMETRIC_REPRESENTATION_ITEM()
RATIONAL_B_SPLINE_CURVE((1.,1.,1.,1.,1.,1.,1.,1.,1.,1.,1.,1.,1.,1.,1.,1.,
1.,1.,1.,1.,1.,1.,1.,1.,1.,1.,1.,1.,1.,1.,1.,1.,1.,1.,1.,1.,1.,1.,1.,1.,
1.,1.,1.,1.,1.,1.,1.,1.,1.,1.,1.,1.,1.,1.,1.,1.,1.,1.,1.,1.,1.,1.,1.,1.,
1.,1.,1.,1.,1.,1.))
REPRESENTATION_ITEM('')
);
#153=(
BOUNDED_CURVE()
B_SPLINE_CURVE(5,(#28410,#28411,#28412,#28413,#28414,#28415,#28416,#28417,
#28418,#28419,#28420,#28421,#28422,#28423,#28424,#28425,#28426,#28427,#28428,
#28429,#28430,#28431,#28432,#28433,#28434,#28435,#28436,#28437,#28438,#28439,
#28440,#28441,#28442,#28443,#28444,#28445,#28446,#28447,#28448,#28449,#28450,
#28451,#28452,#28453,#28454,#28455,#28456,#28457,#28458,#28459,#28460,#28461,
#28462,#28463,#28464,#28465,#28466,#28467,#28468,#28469,#28470,#28471,#28472,
#28473,#28474,#28475,#28476,#28477,#28478,#28479),.UNSPECIFIED.,.F.,.F.)
B_SPLINE_CURVE_WITH_KNOTS((6,1,1,1,1,1,1,1,1,1,1,1,1,1,1,1,1,1,1,1,1,1,
1,1,1,1,1,1,1,1,1,1,1,1,1,1,1,1,1,1,1,1,1,1,1,1,1,1,1,1,1,1,1,1,1,1,1,1,
1,1,1,1,1,1,1,6),(0.,0.0153846153846154,0.0307692307692308,0.0461538461538462,
0.0615384615384615,0.0769230769230769,0.0923076923076923,0.107692307692308,
0.123076923076923,0.138461538461538,0.153846153846154,0.169230769230769,
0.184615384615385,0.2,0.215384615384615,0.230769230769231,0.246153846153846,
0.261538461538462,0.276923076923077,0.292307692307692,0.307692307692308,
0.323076923076923,0.338461538461538,0.353846153846154,0.369230769230769,
0.384615384615385,0.4,0.415384615384615,0.430769230769231,0.446153846153846,
0.461538461538462,0.476923076923077,0.492307692307692,0.507692307692308,
0.523076923076923,0.538461538461538,0.553846153846154,0.569230769230769,
0.584615384615384,0.6,0.615384615384615,0.63076923076923,0.646153846153846,
0.661538461538461,0.676923076923076,0.692307692307692,0.707692307692307,
0.723076923076922,0.738461538461538,0.753846153846153,0.769230769230768,
0.784615384615384,0.799999999999999,0.815384615384614,0.83076923076923,
0.846153846153845,0.86153846153846,0.876923076923076,0.892307692307691,
0.907692307692306,0.923076923076922,0.938461538461537,0.953846153846152,
0.969230769230768,0.984615384615383,1.),.UNSPECIFIED.)
CURVE()
GEOMETRIC_REPRESENTATION_ITEM()
RATIONAL_B_SPLINE_CURVE((1.,1.,1.,1.,1.,1.,1.,1.,1.,1.,1.,1.,1.,1.,1.,1.,
1.,1.,1.,1.,1.,1.,1.,1.,1.,1.,1.,1.,1.,1.,1.,1.,1.,1.,1.,1.,1.,1.,1.,1.,
1.,1.,1.,1.,1.,1.,1.,1.,1.,1.,1.,1.,1.,1.,1.,1.,1.,1.,1.,1.,1.,1.,1.,1.,
1.,1.,1.,1.,1.,1.))
REPRESENTATION_ITEM('')
);
#154=(
BOUNDED_CURVE()
B_SPLINE_CURVE(5,(#28483,#28484,#28485,#28486,#28487,#28488,#28489,#28490,
#28491,#28492,#28493,#28494,#28495,#28496,#28497,#28498,#28499,#28500,#28501,
#28502,#28503,#28504,#28505,#28506,#28507,#28508,#28509,#28510,#28511,#28512,
#28513,#28514,#28515,#28516,#28517,#28518,#28519,#28520,#28521,#28522,#28523,
#28524,#28525,#28526,#28527,#28528,#28529,#28530,#28531,#28532,#28533,#28534,
#28535,#28536,#28537,#28538,#28539,#28540,#28541,#28542,#28543,#28544,#28545,
#28546,#28547,#28548,#28549,#28550,#28551,#28552),.UNSPECIFIED.,.F.,.F.)
B_SPLINE_CURVE_WITH_KNOTS((6,1,1,1,1,1,1,1,1,1,1,1,1,1,1,1,1,1,1,1,1,1,
1,1,1,1,1,1,1,1,1,1,1,1,1,1,1,1,1,1,1,1,1,1,1,1,1,1,1,1,1,1,1,1,1,1,1,1,
1,1,1,1,1,1,1,6),(0.,0.0153846153846154,0.0307692307692308,0.0461538461538462,
0.0615384615384615,0.0769230769230769,0.0923076923076923,0.107692307692308,
0.123076923076923,0.138461538461538,0.153846153846154,0.169230769230769,
0.184615384615385,0.2,0.215384615384615,0.230769230769231,0.246153846153846,
0.261538461538462,0.276923076923077,0.292307692307692,0.307692307692308,
0.323076923076923,0.338461538461538,0.353846153846154,0.369230769230769,
0.384615384615385,0.4,0.415384615384615,0.430769230769231,0.446153846153846,
0.461538461538462,0.476923076923077,0.492307692307692,0.507692307692308,
0.523076923076923,0.538461538461538,0.553846153846154,0.569230769230769,
0.584615384615384,0.6,0.615384615384615,0.63076923076923,0.646153846153846,
0.661538461538461,0.676923076923076,0.692307692307692,0.707692307692307,
0.723076923076922,0.738461538461538,0.753846153846153,0.769230769230768,
0.784615384615384,0.799999999999999,0.815384615384614,0.83076923076923,
0.846153846153845,0.86153846153846,0.876923076923076,0.892307692307691,
0.907692307692306,0.923076923076922,0.938461538461537,0.953846153846152,
0.969230769230768,0.984615384615383,1.),.UNSPECIFIED.)
CURVE()
GEOMETRIC_REPRESENTATION_ITEM()
RATIONAL_B_SPLINE_CURVE((1.,1.,1.,1.,1.,1.,1.,1.,1.,1.,1.,1.,1.,1.,1.,1.,
1.,1.,1.,1.,1.,1.,1.,1.,1.,1.,1.,1.,1.,1.,1.,1.,1.,1.,1.,1.,1.,1.,1.,1.,
1.,1.,1.,1.,1.,1.,1.,1.,1.,1.,1.,1.,1.,1.,1.,1.,1.,1.,1.,1.,1.,1.,1.,1.,
1.,1.,1.,1.,1.,1.))
REPRESENTATION_ITEM('')
);
#155=(
BOUNDED_CURVE()
B_SPLINE_CURVE(5,(#28556,#28557,#28558,#28559,#28560,#28561,#28562,#28563,
#28564,#28565,#28566,#28567,#28568,#28569,#28570,#28571,#28572,#28573,#28574,
#28575,#28576,#28577,#28578,#28579,#28580,#28581,#28582,#28583,#28584,#28585,
#28586,#28587,#28588,#28589,#28590,#28591,#28592,#28593,#28594,#28595,#28596,
#28597,#28598,#28599,#28600,#28601,#28602,#28603,#28604,#28605,#28606,#28607,
#28608,#28609,#28610,#28611,#28612,#28613,#28614,#28615,#28616,#28617,#28618,
#28619,#28620,#28621,#28622,#28623,#28624,#28625),.UNSPECIFIED.,.F.,.F.)
B_SPLINE_CURVE_WITH_KNOTS((6,1,1,1,1,1,1,1,1,1,1,1,1,1,1,1,1,1,1,1,1,1,
1,1,1,1,1,1,1,1,1,1,1,1,1,1,1,1,1,1,1,1,1,1,1,1,1,1,1,1,1,1,1,1,1,1,1,1,
1,1,1,1,1,1,1,6),(0.,0.0153846153846154,0.0307692307692308,0.0461538461538462,
0.0615384615384615,0.0769230769230769,0.0923076923076923,0.107692307692308,
0.123076923076923,0.138461538461538,0.153846153846154,0.169230769230769,
0.184615384615385,0.2,0.215384615384615,0.230769230769231,0.246153846153846,
0.261538461538462,0.276923076923077,0.292307692307692,0.307692307692308,
0.323076923076923,0.338461538461538,0.353846153846154,0.369230769230769,
0.384615384615385,0.4,0.415384615384615,0.430769230769231,0.446153846153846,
0.461538461538462,0.476923076923077,0.492307692307692,0.507692307692308,
0.523076923076923,0.538461538461538,0.553846153846154,0.569230769230769,
0.584615384615384,0.6,0.615384615384615,0.63076923076923,0.646153846153846,
0.661538461538461,0.676923076923076,0.692307692307692,0.707692307692307,
0.723076923076922,0.738461538461538,0.753846153846153,0.769230769230768,
0.784615384615384,0.799999999999999,0.815384615384614,0.83076923076923,
0.846153846153845,0.86153846153846,0.876923076923076,0.892307692307691,
0.907692307692306,0.923076923076922,0.938461538461537,0.953846153846152,
0.969230769230768,0.984615384615383,1.),.UNSPECIFIED.)
CURVE()
GEOMETRIC_REPRESENTATION_ITEM()
RATIONAL_B_SPLINE_CURVE((1.,1.,1.,1.,1.,1.,1.,1.,1.,1.,1.,1.,1.,1.,1.,1.,
1.,1.,1.,1.,1.,1.,1.,1.,1.,1.,1.,1.,1.,1.,1.,1.,1.,1.,1.,1.,1.,1.,1.,1.,
1.,1.,1.,1.,1.,1.,1.,1.,1.,1.,1.,1.,1.,1.,1.,1.,1.,1.,1.,1.,1.,1.,1.,1.,
1.,1.,1.,1.,1.,1.))
REPRESENTATION_ITEM('')
);
#156=(
BOUNDED_CURVE()
B_SPLINE_CURVE(5,(#28629,#28630,#28631,#28632,#28633,#28634,#28635,#28636,
#28637,#28638,#28639,#28640,#28641,#28642,#28643,#28644,#28645,#28646,#28647,
#28648,#28649,#28650,#28651,#28652,#28653,#28654,#28655,#28656,#28657,#28658,
#28659,#28660,#28661,#28662,#28663,#28664,#28665,#28666,#28667,#28668,#28669,
#28670,#28671,#28672,#28673,#28674,#28675,#28676,#28677,#28678,#28679,#28680,
#28681,#28682,#28683,#28684,#28685,#28686,#28687,#28688,#28689,#28690,#28691,
#28692,#28693,#28694,#28695,#28696,#28697,#28698),.UNSPECIFIED.,.F.,.F.)
B_SPLINE_CURVE_WITH_KNOTS((6,1,1,1,1,1,1,1,1,1,1,1,1,1,1,1,1,1,1,1,1,1,
1,1,1,1,1,1,1,1,1,1,1,1,1,1,1,1,1,1,1,1,1,1,1,1,1,1,1,1,1,1,1,1,1,1,1,1,
1,1,1,1,1,1,1,6),(0.,0.0153846153846154,0.0307692307692308,0.0461538461538462,
0.0615384615384615,0.0769230769230769,0.0923076923076923,0.107692307692308,
0.123076923076923,0.138461538461538,0.153846153846154,0.169230769230769,
0.184615384615385,0.2,0.215384615384615,0.230769230769231,0.246153846153846,
0.261538461538462,0.276923076923077,0.292307692307692,0.307692307692308,
0.323076923076923,0.338461538461538,0.353846153846154,0.369230769230769,
0.384615384615385,0.4,0.415384615384615,0.430769230769231,0.446153846153846,
0.461538461538462,0.476923076923077,0.492307692307692,0.507692307692308,
0.523076923076923,0.538461538461538,0.553846153846154,0.569230769230769,
0.584615384615384,0.6,0.615384615384615,0.63076923076923,0.646153846153846,
0.661538461538461,0.676923076923076,0.692307692307692,0.707692307692307,
0.723076923076922,0.738461538461538,0.753846153846153,0.769230769230768,
0.784615384615384,0.799999999999999,0.815384615384614,0.83076923076923,
0.846153846153845,0.86153846153846,0.876923076923076,0.892307692307691,
0.907692307692306,0.923076923076922,0.938461538461537,0.953846153846152,
0.969230769230768,0.984615384615383,1.),.UNSPECIFIED.)
CURVE()
GEOMETRIC_REPRESENTATION_ITEM()
RATIONAL_B_SPLINE_CURVE((1.,1.,1.,1.,1.,1.,1.,1.,1.,1.,1.,1.,1.,1.,1.,1.,
1.,1.,1.,1.,1.,1.,1.,1.,1.,1.,1.,1.,1.,1.,1.,1.,1.,1.,1.,1.,1.,1.,1.,1.,
1.,1.,1.,1.,1.,1.,1.,1.,1.,1.,1.,1.,1.,1.,1.,1.,1.,1.,1.,1.,1.,1.,1.,1.,
1.,1.,1.,1.,1.,1.))
REPRESENTATION_ITEM('')
);
#157=(
BOUNDED_CURVE()
B_SPLINE_CURVE(5,(#28702,#28703,#28704,#28705,#28706,#28707,#28708,#28709,
#28710,#28711,#28712,#28713,#28714,#28715,#28716,#28717,#28718,#28719,#28720,
#28721,#28722,#28723,#28724,#28725,#28726,#28727,#28728,#28729,#28730,#28731,
#28732,#28733,#28734,#28735,#28736,#28737,#28738,#28739,#28740,#28741,#28742,
#28743,#28744,#28745,#28746,#28747,#28748,#28749,#28750,#28751,#28752,#28753,
#28754,#28755,#28756,#28757,#28758,#28759,#28760,#28761,#28762,#28763,#28764,
#28765,#28766,#28767,#28768,#28769,#28770,#28771),.UNSPECIFIED.,.F.,.F.)
B_SPLINE_CURVE_WITH_KNOTS((6,1,1,1,1,1,1,1,1,1,1,1,1,1,1,1,1,1,1,1,1,1,
1,1,1,1,1,1,1,1,1,1,1,1,1,1,1,1,1,1,1,1,1,1,1,1,1,1,1,1,1,1,1,1,1,1,1,1,
1,1,1,1,1,1,1,6),(0.,0.0153846153846154,0.0307692307692308,0.0461538461538462,
0.0615384615384615,0.0769230769230769,0.0923076923076923,0.107692307692308,
0.123076923076923,0.138461538461538,0.153846153846154,0.169230769230769,
0.184615384615385,0.2,0.215384615384615,0.230769230769231,0.246153846153846,
0.261538461538462,0.276923076923077,0.292307692307692,0.307692307692308,
0.323076923076923,0.338461538461538,0.353846153846154,0.369230769230769,
0.384615384615385,0.4,0.415384615384615,0.430769230769231,0.446153846153846,
0.461538461538462,0.476923076923077,0.492307692307692,0.507692307692308,
0.523076923076923,0.538461538461538,0.553846153846154,0.569230769230769,
0.584615384615384,0.6,0.615384615384615,0.63076923076923,0.646153846153846,
0.661538461538461,0.676923076923076,0.692307692307692,0.707692307692307,
0.723076923076922,0.738461538461538,0.753846153846153,0.769230769230768,
0.784615384615384,0.799999999999999,0.815384615384614,0.83076923076923,
0.846153846153845,0.86153846153846,0.876923076923076,0.892307692307691,
0.907692307692306,0.923076923076922,0.938461538461537,0.953846153846152,
0.969230769230768,0.984615384615383,1.),.UNSPECIFIED.)
CURVE()
GEOMETRIC_REPRESENTATION_ITEM()
RATIONAL_B_SPLINE_CURVE((1.,1.,1.,1.,1.,1.,1.,1.,1.,1.,1.,1.,1.,1.,1.,1.,
1.,1.,1.,1.,1.,1.,1.,1.,1.,1.,1.,1.,1.,1.,1.,1.,1.,1.,1.,1.,1.,1.,1.,1.,
1.,1.,1.,1.,1.,1.,1.,1.,1.,1.,1.,1.,1.,1.,1.,1.,1.,1.,1.,1.,1.,1.,1.,1.,
1.,1.,1.,1.,1.,1.))
REPRESENTATION_ITEM('')
);
#158=(
BOUNDED_CURVE()
B_SPLINE_CURVE(5,(#28775,#28776,#28777,#28778,#28779,#28780,#28781,#28782,
#28783,#28784,#28785,#28786,#28787,#28788,#28789,#28790,#28791,#28792,#28793,
#28794,#28795,#28796,#28797,#28798,#28799,#28800,#28801,#28802,#28803,#28804,
#28805,#28806,#28807,#28808,#28809,#28810,#28811,#28812,#28813,#28814,#28815,
#28816,#28817,#28818,#28819,#28820,#28821,#28822,#28823,#28824,#28825,#28826,
#28827,#28828,#28829,#28830,#28831,#28832,#28833,#28834,#28835,#28836,#28837,
#28838,#28839,#28840,#28841,#28842,#28843,#28844),.UNSPECIFIED.,.F.,.F.)
B_SPLINE_CURVE_WITH_KNOTS((6,1,1,1,1,1,1,1,1,1,1,1,1,1,1,1,1,1,1,1,1,1,
1,1,1,1,1,1,1,1,1,1,1,1,1,1,1,1,1,1,1,1,1,1,1,1,1,1,1,1,1,1,1,1,1,1,1,1,
1,1,1,1,1,1,1,6),(0.,0.0153846153846154,0.0307692307692308,0.0461538461538462,
0.0615384615384615,0.0769230769230769,0.0923076923076923,0.107692307692308,
0.123076923076923,0.138461538461538,0.153846153846154,0.169230769230769,
0.184615384615385,0.2,0.215384615384615,0.230769230769231,0.246153846153846,
0.261538461538462,0.276923076923077,0.292307692307692,0.307692307692308,
0.323076923076923,0.338461538461538,0.353846153846154,0.369230769230769,
0.384615384615385,0.4,0.415384615384615,0.430769230769231,0.446153846153846,
0.461538461538462,0.476923076923077,0.492307692307692,0.507692307692308,
0.523076923076923,0.538461538461538,0.553846153846154,0.569230769230769,
0.584615384615384,0.6,0.615384615384615,0.63076923076923,0.646153846153846,
0.661538461538461,0.676923076923076,0.692307692307692,0.707692307692307,
0.723076923076922,0.738461538461538,0.753846153846153,0.769230769230768,
0.784615384615384,0.799999999999999,0.815384615384614,0.83076923076923,
0.846153846153845,0.86153846153846,0.876923076923076,0.892307692307691,
0.907692307692306,0.923076923076922,0.938461538461537,0.953846153846152,
0.969230769230768,0.984615384615383,1.),.UNSPECIFIED.)
CURVE()
GEOMETRIC_REPRESENTATION_ITEM()
RATIONAL_B_SPLINE_CURVE((1.,1.,1.,1.,1.,1.,1.,1.,1.,1.,1.,1.,1.,1.,1.,1.,
1.,1.,1.,1.,1.,1.,1.,1.,1.,1.,1.,1.,1.,1.,1.,1.,1.,1.,1.,1.,1.,1.,1.,1.,
1.,1.,1.,1.,1.,1.,1.,1.,1.,1.,1.,1.,1.,1.,1.,1.,1.,1.,1.,1.,1.,1.,1.,1.,
1.,1.,1.,1.,1.,1.))
REPRESENTATION_ITEM('')
);
#159=(
BOUNDED_CURVE()
B_SPLINE_CURVE(5,(#28848,#28849,#28850,#28851,#28852,#28853,#28854,#28855,
#28856,#28857,#28858,#28859,#28860,#28861,#28862,#28863,#28864,#28865,#28866,
#28867,#28868,#28869,#28870,#28871,#28872,#28873,#28874,#28875,#28876,#28877,
#28878,#28879,#28880,#28881,#28882,#28883,#28884,#28885,#28886,#28887,#28888,
#28889,#28890,#28891,#28892,#28893,#28894,#28895,#28896,#28897,#28898,#28899,
#28900,#28901,#28902,#28903,#28904,#28905,#28906,#28907,#28908,#28909,#28910,
#28911,#28912,#28913,#28914,#28915,#28916,#28917),.UNSPECIFIED.,.F.,.F.)
B_SPLINE_CURVE_WITH_KNOTS((6,1,1,1,1,1,1,1,1,1,1,1,1,1,1,1,1,1,1,1,1,1,
1,1,1,1,1,1,1,1,1,1,1,1,1,1,1,1,1,1,1,1,1,1,1,1,1,1,1,1,1,1,1,1,1,1,1,1,
1,1,1,1,1,1,1,6),(0.,0.0153846153846154,0.0307692307692308,0.0461538461538462,
0.0615384615384615,0.0769230769230769,0.0923076923076923,0.107692307692308,
0.123076923076923,0.138461538461538,0.153846153846154,0.169230769230769,
0.184615384615385,0.2,0.215384615384615,0.230769230769231,0.246153846153846,
0.261538461538462,0.276923076923077,0.292307692307692,0.307692307692308,
0.323076923076923,0.338461538461538,0.353846153846154,0.369230769230769,
0.384615384615385,0.4,0.415384615384615,0.430769230769231,0.446153846153846,
0.461538461538462,0.476923076923077,0.492307692307692,0.507692307692308,
0.523076923076923,0.538461538461538,0.553846153846154,0.569230769230769,
0.584615384615384,0.6,0.615384615384615,0.63076923076923,0.646153846153846,
0.661538461538461,0.676923076923076,0.692307692307692,0.707692307692307,
0.723076923076922,0.738461538461538,0.753846153846153,0.769230769230768,
0.784615384615384,0.799999999999999,0.815384615384614,0.83076923076923,
0.846153846153845,0.86153846153846,0.876923076923076,0.892307692307691,
0.907692307692306,0.923076923076922,0.938461538461537,0.953846153846152,
0.969230769230768,0.984615384615383,1.),.UNSPECIFIED.)
CURVE()
GEOMETRIC_REPRESENTATION_ITEM()
RATIONAL_B_SPLINE_CURVE((1.,1.,1.,1.,1.,1.,1.,1.,1.,1.,1.,1.,1.,1.,1.,1.,
1.,1.,1.,1.,1.,1.,1.,1.,1.,1.,1.,1.,1.,1.,1.,1.,1.,1.,1.,1.,1.,1.,1.,1.,
1.,1.,1.,1.,1.,1.,1.,1.,1.,1.,1.,1.,1.,1.,1.,1.,1.,1.,1.,1.,1.,1.,1.,1.,
1.,1.,1.,1.,1.,1.))
REPRESENTATION_ITEM('')
);
#160=(
BOUNDED_CURVE()
B_SPLINE_CURVE(5,(#28921,#28922,#28923,#28924,#28925,#28926,#28927,#28928,
#28929,#28930,#28931,#28932,#28933,#28934,#28935,#28936,#28937,#28938,#28939,
#28940,#28941,#28942,#28943,#28944,#28945,#28946,#28947,#28948,#28949,#28950,
#28951,#28952,#28953,#28954,#28955,#28956,#28957,#28958,#28959,#28960,#28961,
#28962,#28963,#28964,#28965,#28966,#28967,#28968,#28969,#28970,#28971,#28972,
#28973,#28974,#28975,#28976,#28977,#28978,#28979,#28980,#28981,#28982,#28983,
#28984,#28985,#28986,#28987,#28988,#28989,#28990),.UNSPECIFIED.,.F.,.F.)
B_SPLINE_CURVE_WITH_KNOTS((6,1,1,1,1,1,1,1,1,1,1,1,1,1,1,1,1,1,1,1,1,1,
1,1,1,1,1,1,1,1,1,1,1,1,1,1,1,1,1,1,1,1,1,1,1,1,1,1,1,1,1,1,1,1,1,1,1,1,
1,1,1,1,1,1,1,6),(0.,0.0153846153846154,0.0307692307692308,0.0461538461538462,
0.0615384615384615,0.0769230769230769,0.0923076923076923,0.107692307692308,
0.123076923076923,0.138461538461538,0.153846153846154,0.169230769230769,
0.184615384615385,0.2,0.215384615384615,0.230769230769231,0.246153846153846,
0.261538461538462,0.276923076923077,0.292307692307692,0.307692307692308,
0.323076923076923,0.338461538461538,0.353846153846154,0.369230769230769,
0.384615384615385,0.4,0.415384615384615,0.430769230769231,0.446153846153846,
0.461538461538462,0.476923076923077,0.492307692307692,0.507692307692308,
0.523076923076923,0.538461538461538,0.553846153846154,0.569230769230769,
0.584615384615384,0.6,0.615384615384615,0.63076923076923,0.646153846153846,
0.661538461538461,0.676923076923076,0.692307692307692,0.707692307692307,
0.723076923076922,0.738461538461538,0.753846153846153,0.769230769230768,
0.784615384615384,0.799999999999999,0.815384615384614,0.83076923076923,
0.846153846153845,0.86153846153846,0.876923076923076,0.892307692307691,
0.907692307692306,0.923076923076922,0.938461538461537,0.953846153846152,
0.969230769230768,0.984615384615383,1.),.UNSPECIFIED.)
CURVE()
GEOMETRIC_REPRESENTATION_ITEM()
RATIONAL_B_SPLINE_CURVE((1.,1.,1.,1.,1.,1.,1.,1.,1.,1.,1.,1.,1.,1.,1.,1.,
1.,1.,1.,1.,1.,1.,1.,1.,1.,1.,1.,1.,1.,1.,1.,1.,1.,1.,1.,1.,1.,1.,1.,1.,
1.,1.,1.,1.,1.,1.,1.,1.,1.,1.,1.,1.,1.,1.,1.,1.,1.,1.,1.,1.,1.,1.,1.,1.,
1.,1.,1.,1.,1.,1.))
REPRESENTATION_ITEM('')
);
#161=(
BOUNDED_CURVE()
B_SPLINE_CURVE(5,(#28994,#28995,#28996,#28997,#28998,#28999,#29000,#29001,
#29002,#29003,#29004,#29005,#29006,#29007,#29008,#29009,#29010,#29011,#29012,
#29013,#29014,#29015,#29016,#29017,#29018,#29019,#29020,#29021,#29022,#29023,
#29024,#29025,#29026,#29027,#29028,#29029,#29030,#29031,#29032,#29033,#29034,
#29035,#29036,#29037,#29038,#29039,#29040,#29041,#29042,#29043,#29044,#29045,
#29046,#29047,#29048,#29049,#29050,#29051,#29052,#29053,#29054,#29055,#29056,
#29057,#29058,#29059,#29060,#29061,#29062,#29063),.UNSPECIFIED.,.F.,.F.)
B_SPLINE_CURVE_WITH_KNOTS((6,1,1,1,1,1,1,1,1,1,1,1,1,1,1,1,1,1,1,1,1,1,
1,1,1,1,1,1,1,1,1,1,1,1,1,1,1,1,1,1,1,1,1,1,1,1,1,1,1,1,1,1,1,1,1,1,1,1,
1,1,1,1,1,1,1,6),(0.,0.0153846153846154,0.0307692307692308,0.0461538461538462,
0.0615384615384615,0.0769230769230769,0.0923076923076923,0.107692307692308,
0.123076923076923,0.138461538461538,0.153846153846154,0.169230769230769,
0.184615384615385,0.2,0.215384615384615,0.230769230769231,0.246153846153846,
0.261538461538462,0.276923076923077,0.292307692307692,0.307692307692308,
0.323076923076923,0.338461538461538,0.353846153846154,0.369230769230769,
0.384615384615385,0.4,0.415384615384615,0.430769230769231,0.446153846153846,
0.461538461538462,0.476923076923077,0.492307692307692,0.507692307692308,
0.523076923076923,0.538461538461538,0.553846153846154,0.569230769230769,
0.584615384615384,0.6,0.615384615384615,0.63076923076923,0.646153846153846,
0.661538461538461,0.676923076923076,0.692307692307692,0.707692307692307,
0.723076923076922,0.738461538461538,0.753846153846153,0.769230769230768,
0.784615384615384,0.799999999999999,0.815384615384614,0.83076923076923,
0.846153846153845,0.86153846153846,0.876923076923076,0.892307692307691,
0.907692307692306,0.923076923076922,0.938461538461537,0.953846153846152,
0.969230769230768,0.984615384615383,1.),.UNSPECIFIED.)
CURVE()
GEOMETRIC_REPRESENTATION_ITEM()
RATIONAL_B_SPLINE_CURVE((1.,1.,1.,1.,1.,1.,1.,1.,1.,1.,1.,1.,1.,1.,1.,1.,
1.,1.,1.,1.,1.,1.,1.,1.,1.,1.,1.,1.,1.,1.,1.,1.,1.,1.,1.,1.,1.,1.,1.,1.,
1.,1.,1.,1.,1.,1.,1.,1.,1.,1.,1.,1.,1.,1.,1.,1.,1.,1.,1.,1.,1.,1.,1.,1.,
1.,1.,1.,1.,1.,1.))
REPRESENTATION_ITEM('')
);
#162=(
BOUNDED_CURVE()
B_SPLINE_CURVE(5,(#29067,#29068,#29069,#29070,#29071,#29072,#29073,#29074,
#29075,#29076,#29077,#29078,#29079,#29080,#29081,#29082,#29083,#29084,#29085,
#29086,#29087,#29088,#29089,#29090,#29091,#29092,#29093,#29094,#29095,#29096,
#29097,#29098,#29099,#29100,#29101,#29102,#29103,#29104,#29105,#29106,#29107,
#29108,#29109,#29110,#29111,#29112,#29113,#29114,#29115,#29116,#29117,#29118,
#29119,#29120,#29121,#29122,#29123,#29124,#29125,#29126,#29127,#29128,#29129,
#29130,#29131,#29132,#29133,#29134,#29135,#29136),.UNSPECIFIED.,.F.,.F.)
B_SPLINE_CURVE_WITH_KNOTS((6,1,1,1,1,1,1,1,1,1,1,1,1,1,1,1,1,1,1,1,1,1,
1,1,1,1,1,1,1,1,1,1,1,1,1,1,1,1,1,1,1,1,1,1,1,1,1,1,1,1,1,1,1,1,1,1,1,1,
1,1,1,1,1,1,1,6),(0.,0.0153846153846154,0.0307692307692308,0.0461538461538462,
0.0615384615384615,0.0769230769230769,0.0923076923076923,0.107692307692308,
0.123076923076923,0.138461538461538,0.153846153846154,0.169230769230769,
0.184615384615385,0.2,0.215384615384615,0.230769230769231,0.246153846153846,
0.261538461538462,0.276923076923077,0.292307692307692,0.307692307692308,
0.323076923076923,0.338461538461538,0.353846153846154,0.369230769230769,
0.384615384615385,0.4,0.415384615384615,0.430769230769231,0.446153846153846,
0.461538461538462,0.476923076923077,0.492307692307692,0.507692307692308,
0.523076923076923,0.538461538461538,0.553846153846154,0.569230769230769,
0.584615384615384,0.6,0.615384615384615,0.63076923076923,0.646153846153846,
0.661538461538461,0.676923076923076,0.692307692307692,0.707692307692307,
0.723076923076922,0.738461538461538,0.753846153846153,0.769230769230768,
0.784615384615384,0.799999999999999,0.815384615384614,0.83076923076923,
0.846153846153845,0.86153846153846,0.876923076923076,0.892307692307691,
0.907692307692306,0.923076923076922,0.938461538461537,0.953846153846152,
0.969230769230768,0.984615384615383,1.),.UNSPECIFIED.)
CURVE()
GEOMETRIC_REPRESENTATION_ITEM()
RATIONAL_B_SPLINE_CURVE((1.,1.,1.,1.,1.,1.,1.,1.,1.,1.,1.,1.,1.,1.,1.,1.,
1.,1.,1.,1.,1.,1.,1.,1.,1.,1.,1.,1.,1.,1.,1.,1.,1.,1.,1.,1.,1.,1.,1.,1.,
1.,1.,1.,1.,1.,1.,1.,1.,1.,1.,1.,1.,1.,1.,1.,1.,1.,1.,1.,1.,1.,1.,1.,1.,
1.,1.,1.,1.,1.,1.))
REPRESENTATION_ITEM('')
);
#163=(
BOUNDED_CURVE()
B_SPLINE_CURVE(5,(#29140,#29141,#29142,#29143,#29144,#29145,#29146,#29147,
#29148,#29149,#29150,#29151,#29152,#29153,#29154,#29155,#29156,#29157,#29158,
#29159,#29160,#29161,#29162,#29163,#29164,#29165,#29166,#29167,#29168,#29169,
#29170,#29171,#29172,#29173,#29174,#29175,#29176,#29177,#29178,#29179,#29180,
#29181,#29182,#29183,#29184,#29185,#29186,#29187,#29188,#29189,#29190,#29191,
#29192,#29193,#29194,#29195,#29196,#29197,#29198,#29199,#29200,#29201,#29202,
#29203,#29204,#29205,#29206,#29207,#29208,#29209),.UNSPECIFIED.,.F.,.F.)
B_SPLINE_CURVE_WITH_KNOTS((6,1,1,1,1,1,1,1,1,1,1,1,1,1,1,1,1,1,1,1,1,1,
1,1,1,1,1,1,1,1,1,1,1,1,1,1,1,1,1,1,1,1,1,1,1,1,1,1,1,1,1,1,1,1,1,1,1,1,
1,1,1,1,1,1,1,6),(0.,0.0153846153846154,0.0307692307692308,0.0461538461538462,
0.0615384615384615,0.0769230769230769,0.0923076923076923,0.107692307692308,
0.123076923076923,0.138461538461538,0.153846153846154,0.169230769230769,
0.184615384615385,0.2,0.215384615384615,0.230769230769231,0.246153846153846,
0.261538461538462,0.276923076923077,0.292307692307692,0.307692307692308,
0.323076923076923,0.338461538461538,0.353846153846154,0.369230769230769,
0.384615384615385,0.4,0.415384615384615,0.430769230769231,0.446153846153846,
0.461538461538462,0.476923076923077,0.492307692307692,0.507692307692308,
0.523076923076923,0.538461538461538,0.553846153846154,0.569230769230769,
0.584615384615384,0.6,0.615384615384615,0.63076923076923,0.646153846153846,
0.661538461538461,0.676923076923076,0.692307692307692,0.707692307692307,
0.723076923076922,0.738461538461538,0.753846153846153,0.769230769230768,
0.784615384615384,0.799999999999999,0.815384615384614,0.83076923076923,
0.846153846153845,0.86153846153846,0.876923076923076,0.892307692307691,
0.907692307692306,0.923076923076922,0.938461538461537,0.953846153846152,
0.969230769230768,0.984615384615383,1.),.UNSPECIFIED.)
CURVE()
GEOMETRIC_REPRESENTATION_ITEM()
RATIONAL_B_SPLINE_CURVE((1.,1.,1.,1.,1.,1.,1.,1.,1.,1.,1.,1.,1.,1.,1.,1.,
1.,1.,1.,1.,1.,1.,1.,1.,1.,1.,1.,1.,1.,1.,1.,1.,1.,1.,1.,1.,1.,1.,1.,1.,
1.,1.,1.,1.,1.,1.,1.,1.,1.,1.,1.,1.,1.,1.,1.,1.,1.,1.,1.,1.,1.,1.,1.,1.,
1.,1.,1.,1.,1.,1.))
REPRESENTATION_ITEM('')
);
#164=(
BOUNDED_CURVE()
B_SPLINE_CURVE(5,(#29213,#29214,#29215,#29216,#29217,#29218,#29219,#29220,
#29221,#29222,#29223,#29224,#29225,#29226,#29227,#29228,#29229,#29230,#29231,
#29232,#29233,#29234,#29235,#29236,#29237,#29238,#29239,#29240,#29241,#29242,
#29243,#29244,#29245,#29246,#29247,#29248,#29249,#29250,#29251,#29252,#29253,
#29254,#29255,#29256,#29257,#29258,#29259,#29260,#29261,#29262,#29263,#29264,
#29265,#29266,#29267,#29268,#29269,#29270,#29271,#29272,#29273,#29274,#29275,
#29276,#29277,#29278,#29279,#29280,#29281,#29282),.UNSPECIFIED.,.F.,.F.)
B_SPLINE_CURVE_WITH_KNOTS((6,1,1,1,1,1,1,1,1,1,1,1,1,1,1,1,1,1,1,1,1,1,
1,1,1,1,1,1,1,1,1,1,1,1,1,1,1,1,1,1,1,1,1,1,1,1,1,1,1,1,1,1,1,1,1,1,1,1,
1,1,1,1,1,1,1,6),(0.,0.0153846153846154,0.0307692307692308,0.0461538461538462,
0.0615384615384615,0.0769230769230769,0.0923076923076923,0.107692307692308,
0.123076923076923,0.138461538461538,0.153846153846154,0.169230769230769,
0.184615384615385,0.2,0.215384615384615,0.230769230769231,0.246153846153846,
0.261538461538462,0.276923076923077,0.292307692307692,0.307692307692308,
0.323076923076923,0.338461538461538,0.353846153846154,0.369230769230769,
0.384615384615385,0.4,0.415384615384615,0.430769230769231,0.446153846153846,
0.461538461538462,0.476923076923077,0.492307692307692,0.507692307692308,
0.523076923076923,0.538461538461538,0.553846153846154,0.569230769230769,
0.584615384615384,0.6,0.615384615384615,0.63076923076923,0.646153846153846,
0.661538461538461,0.676923076923076,0.692307692307692,0.707692307692307,
0.723076923076922,0.738461538461538,0.753846153846153,0.769230769230768,
0.784615384615384,0.799999999999999,0.815384615384614,0.83076923076923,
0.846153846153845,0.86153846153846,0.876923076923076,0.892307692307691,
0.907692307692306,0.923076923076922,0.938461538461537,0.953846153846152,
0.969230769230768,0.984615384615383,1.),.UNSPECIFIED.)
CURVE()
GEOMETRIC_REPRESENTATION_ITEM()
RATIONAL_B_SPLINE_CURVE((1.,1.,1.,1.,1.,1.,1.,1.,1.,1.,1.,1.,1.,1.,1.,1.,
1.,1.,1.,1.,1.,1.,1.,1.,1.,1.,1.,1.,1.,1.,1.,1.,1.,1.,1.,1.,1.,1.,1.,1.,
1.,1.,1.,1.,1.,1.,1.,1.,1.,1.,1.,1.,1.,1.,1.,1.,1.,1.,1.,1.,1.,1.,1.,1.,
1.,1.,1.,1.,1.,1.))
REPRESENTATION_ITEM('')
);
#165=(
BOUNDED_CURVE()
B_SPLINE_CURVE(5,(#29286,#29287,#29288,#29289,#29290,#29291,#29292,#29293,
#29294,#29295,#29296,#29297,#29298,#29299,#29300,#29301,#29302,#29303,#29304,
#29305,#29306,#29307,#29308,#29309,#29310,#29311,#29312,#29313,#29314,#29315,
#29316,#29317,#29318,#29319,#29320,#29321,#29322,#29323,#29324,#29325,#29326,
#29327,#29328,#29329,#29330,#29331,#29332,#29333,#29334,#29335,#29336,#29337,
#29338,#29339,#29340,#29341,#29342,#29343,#29344,#29345,#29346,#29347,#29348,
#29349,#29350,#29351,#29352,#29353,#29354,#29355),.UNSPECIFIED.,.F.,.F.)
B_SPLINE_CURVE_WITH_KNOTS((6,1,1,1,1,1,1,1,1,1,1,1,1,1,1,1,1,1,1,1,1,1,
1,1,1,1,1,1,1,1,1,1,1,1,1,1,1,1,1,1,1,1,1,1,1,1,1,1,1,1,1,1,1,1,1,1,1,1,
1,1,1,1,1,1,1,6),(0.,0.0153846153846154,0.0307692307692308,0.0461538461538462,
0.0615384615384615,0.0769230769230769,0.0923076923076923,0.107692307692308,
0.123076923076923,0.138461538461538,0.153846153846154,0.169230769230769,
0.184615384615385,0.2,0.215384615384615,0.230769230769231,0.246153846153846,
0.261538461538462,0.276923076923077,0.292307692307692,0.307692307692308,
0.323076923076923,0.338461538461538,0.353846153846154,0.369230769230769,
0.384615384615385,0.4,0.415384615384615,0.430769230769231,0.446153846153846,
0.461538461538462,0.476923076923077,0.492307692307692,0.507692307692308,
0.523076923076923,0.538461538461538,0.553846153846154,0.569230769230769,
0.584615384615384,0.6,0.615384615384615,0.63076923076923,0.646153846153846,
0.661538461538461,0.676923076923076,0.692307692307692,0.707692307692307,
0.723076923076922,0.738461538461538,0.753846153846153,0.769230769230768,
0.784615384615384,0.799999999999999,0.815384615384614,0.83076923076923,
0.846153846153845,0.86153846153846,0.876923076923076,0.892307692307691,
0.907692307692306,0.923076923076922,0.938461538461537,0.953846153846152,
0.969230769230768,0.984615384615383,1.),.UNSPECIFIED.)
CURVE()
GEOMETRIC_REPRESENTATION_ITEM()
RATIONAL_B_SPLINE_CURVE((1.,1.,1.,1.,1.,1.,1.,1.,1.,1.,1.,1.,1.,1.,1.,1.,
1.,1.,1.,1.,1.,1.,1.,1.,1.,1.,1.,1.,1.,1.,1.,1.,1.,1.,1.,1.,1.,1.,1.,1.,
1.,1.,1.,1.,1.,1.,1.,1.,1.,1.,1.,1.,1.,1.,1.,1.,1.,1.,1.,1.,1.,1.,1.,1.,
1.,1.,1.,1.,1.,1.))
REPRESENTATION_ITEM('')
);
#166=(
BOUNDED_CURVE()
B_SPLINE_CURVE(5,(#29359,#29360,#29361,#29362,#29363,#29364,#29365,#29366,
#29367,#29368,#29369,#29370,#29371,#29372,#29373,#29374,#29375,#29376,#29377,
#29378,#29379,#29380,#29381,#29382,#29383,#29384,#29385,#29386,#29387,#29388,
#29389,#29390,#29391,#29392,#29393,#29394,#29395,#29396,#29397,#29398,#29399,
#29400,#29401,#29402,#29403,#29404,#29405,#29406,#29407,#29408,#29409,#29410,
#29411,#29412,#29413,#29414,#29415,#29416,#29417,#29418,#29419,#29420,#29421,
#29422,#29423,#29424,#29425,#29426,#29427,#29428),.UNSPECIFIED.,.F.,.F.)
B_SPLINE_CURVE_WITH_KNOTS((6,1,1,1,1,1,1,1,1,1,1,1,1,1,1,1,1,1,1,1,1,1,
1,1,1,1,1,1,1,1,1,1,1,1,1,1,1,1,1,1,1,1,1,1,1,1,1,1,1,1,1,1,1,1,1,1,1,1,
1,1,1,1,1,1,1,6),(0.,0.0153846153846154,0.0307692307692308,0.0461538461538462,
0.0615384615384615,0.0769230769230769,0.0923076923076923,0.107692307692308,
0.123076923076923,0.138461538461538,0.153846153846154,0.169230769230769,
0.184615384615385,0.2,0.215384615384615,0.230769230769231,0.246153846153846,
0.261538461538462,0.276923076923077,0.292307692307692,0.307692307692308,
0.323076923076923,0.338461538461538,0.353846153846154,0.369230769230769,
0.384615384615385,0.4,0.415384615384615,0.430769230769231,0.446153846153846,
0.461538461538462,0.476923076923077,0.492307692307692,0.507692307692308,
0.523076923076923,0.538461538461538,0.553846153846154,0.569230769230769,
0.584615384615384,0.6,0.615384615384615,0.63076923076923,0.646153846153846,
0.661538461538461,0.676923076923076,0.692307692307692,0.707692307692307,
0.723076923076922,0.738461538461538,0.753846153846153,0.769230769230768,
0.784615384615384,0.799999999999999,0.815384615384614,0.83076923076923,
0.846153846153845,0.86153846153846,0.876923076923076,0.892307692307691,
0.907692307692306,0.923076923076922,0.938461538461537,0.953846153846152,
0.969230769230768,0.984615384615383,1.),.UNSPECIFIED.)
CURVE()
GEOMETRIC_REPRESENTATION_ITEM()
RATIONAL_B_SPLINE_CURVE((1.,1.,1.,1.,1.,1.,1.,1.,1.,1.,1.,1.,1.,1.,1.,1.,
1.,1.,1.,1.,1.,1.,1.,1.,1.,1.,1.,1.,1.,1.,1.,1.,1.,1.,1.,1.,1.,1.,1.,1.,
1.,1.,1.,1.,1.,1.,1.,1.,1.,1.,1.,1.,1.,1.,1.,1.,1.,1.,1.,1.,1.,1.,1.,1.,
1.,1.,1.,1.,1.,1.))
REPRESENTATION_ITEM('')
);
#167=(
BOUNDED_CURVE()
B_SPLINE_CURVE(5,(#29432,#29433,#29434,#29435,#29436,#29437,#29438,#29439,
#29440,#29441,#29442,#29443,#29444,#29445,#29446,#29447,#29448,#29449,#29450,
#29451,#29452,#29453,#29454,#29455,#29456,#29457,#29458,#29459,#29460,#29461,
#29462,#29463,#29464,#29465,#29466,#29467,#29468,#29469,#29470,#29471,#29472,
#29473,#29474,#29475,#29476,#29477,#29478,#29479,#29480,#29481,#29482,#29483,
#29484,#29485,#29486,#29487,#29488,#29489,#29490,#29491,#29492,#29493,#29494,
#29495,#29496,#29497,#29498,#29499,#29500,#29501),.UNSPECIFIED.,.F.,.F.)
B_SPLINE_CURVE_WITH_KNOTS((6,1,1,1,1,1,1,1,1,1,1,1,1,1,1,1,1,1,1,1,1,1,
1,1,1,1,1,1,1,1,1,1,1,1,1,1,1,1,1,1,1,1,1,1,1,1,1,1,1,1,1,1,1,1,1,1,1,1,
1,1,1,1,1,1,1,6),(0.,0.0153846153846154,0.0307692307692308,0.0461538461538462,
0.0615384615384615,0.0769230769230769,0.0923076923076923,0.107692307692308,
0.123076923076923,0.138461538461538,0.153846153846154,0.169230769230769,
0.184615384615385,0.2,0.215384615384615,0.230769230769231,0.246153846153846,
0.261538461538462,0.276923076923077,0.292307692307692,0.307692307692308,
0.323076923076923,0.338461538461538,0.353846153846154,0.369230769230769,
0.384615384615385,0.4,0.415384615384615,0.430769230769231,0.446153846153846,
0.461538461538462,0.476923076923077,0.492307692307692,0.507692307692308,
0.523076923076923,0.538461538461538,0.553846153846154,0.569230769230769,
0.584615384615384,0.6,0.615384615384615,0.63076923076923,0.646153846153846,
0.661538461538461,0.676923076923076,0.692307692307692,0.707692307692307,
0.723076923076922,0.738461538461538,0.753846153846153,0.769230769230768,
0.784615384615384,0.799999999999999,0.815384615384614,0.83076923076923,
0.846153846153845,0.86153846153846,0.876923076923076,0.892307692307691,
0.907692307692306,0.923076923076922,0.938461538461537,0.953846153846152,
0.969230769230768,0.984615384615383,1.),.UNSPECIFIED.)
CURVE()
GEOMETRIC_REPRESENTATION_ITEM()
RATIONAL_B_SPLINE_CURVE((1.,1.,1.,1.,1.,1.,1.,1.,1.,1.,1.,1.,1.,1.,1.,1.,
1.,1.,1.,1.,1.,1.,1.,1.,1.,1.,1.,1.,1.,1.,1.,1.,1.,1.,1.,1.,1.,1.,1.,1.,
1.,1.,1.,1.,1.,1.,1.,1.,1.,1.,1.,1.,1.,1.,1.,1.,1.,1.,1.,1.,1.,1.,1.,1.,
1.,1.,1.,1.,1.,1.))
REPRESENTATION_ITEM('')
);
#168=(
BOUNDED_CURVE()
B_SPLINE_CURVE(5,(#29505,#29506,#29507,#29508,#29509,#29510,#29511,#29512,
#29513,#29514,#29515,#29516,#29517,#29518,#29519,#29520,#29521,#29522,#29523,
#29524,#29525,#29526,#29527,#29528,#29529,#29530,#29531,#29532,#29533,#29534,
#29535,#29536,#29537,#29538,#29539,#29540,#29541,#29542,#29543,#29544,#29545,
#29546,#29547,#29548,#29549,#29550,#29551,#29552,#29553,#29554,#29555,#29556,
#29557,#29558,#29559,#29560,#29561,#29562,#29563,#29564,#29565,#29566,#29567,
#29568,#29569,#29570,#29571,#29572,#29573,#29574),.UNSPECIFIED.,.F.,.F.)
B_SPLINE_CURVE_WITH_KNOTS((6,1,1,1,1,1,1,1,1,1,1,1,1,1,1,1,1,1,1,1,1,1,
1,1,1,1,1,1,1,1,1,1,1,1,1,1,1,1,1,1,1,1,1,1,1,1,1,1,1,1,1,1,1,1,1,1,1,1,
1,1,1,1,1,1,1,6),(0.,0.0153846153846154,0.0307692307692308,0.0461538461538462,
0.0615384615384615,0.0769230769230769,0.0923076923076923,0.107692307692308,
0.123076923076923,0.138461538461538,0.153846153846154,0.169230769230769,
0.184615384615385,0.2,0.215384615384615,0.230769230769231,0.246153846153846,
0.261538461538462,0.276923076923077,0.292307692307692,0.307692307692308,
0.323076923076923,0.338461538461538,0.353846153846154,0.369230769230769,
0.384615384615385,0.4,0.415384615384615,0.430769230769231,0.446153846153846,
0.461538461538462,0.476923076923077,0.492307692307692,0.507692307692308,
0.523076923076923,0.538461538461538,0.553846153846154,0.569230769230769,
0.584615384615384,0.6,0.615384615384615,0.63076923076923,0.646153846153846,
0.661538461538461,0.676923076923076,0.692307692307692,0.707692307692307,
0.723076923076922,0.738461538461538,0.753846153846153,0.769230769230768,
0.784615384615384,0.799999999999999,0.815384615384614,0.83076923076923,
0.846153846153845,0.86153846153846,0.876923076923076,0.892307692307691,
0.907692307692306,0.923076923076922,0.938461538461537,0.953846153846152,
0.969230769230768,0.984615384615383,1.),.UNSPECIFIED.)
CURVE()
GEOMETRIC_REPRESENTATION_ITEM()
RATIONAL_B_SPLINE_CURVE((1.,1.,1.,1.,1.,1.,1.,1.,1.,1.,1.,1.,1.,1.,1.,1.,
1.,1.,1.,1.,1.,1.,1.,1.,1.,1.,1.,1.,1.,1.,1.,1.,1.,1.,1.,1.,1.,1.,1.,1.,
1.,1.,1.,1.,1.,1.,1.,1.,1.,1.,1.,1.,1.,1.,1.,1.,1.,1.,1.,1.,1.,1.,1.,1.,
1.,1.,1.,1.,1.,1.))
REPRESENTATION_ITEM('')
);
#169=(
BOUNDED_CURVE()
B_SPLINE_CURVE(5,(#29578,#29579,#29580,#29581,#29582,#29583,#29584,#29585,
#29586,#29587,#29588,#29589,#29590,#29591,#29592,#29593,#29594,#29595,#29596,
#29597,#29598,#29599,#29600,#29601,#29602,#29603,#29604,#29605,#29606,#29607,
#29608,#29609,#29610,#29611,#29612,#29613,#29614,#29615,#29616,#29617,#29618,
#29619,#29620,#29621,#29622,#29623,#29624,#29625,#29626,#29627,#29628,#29629,
#29630,#29631,#29632,#29633,#29634,#29635,#29636,#29637,#29638,#29639,#29640,
#29641,#29642,#29643,#29644,#29645,#29646,#29647),.UNSPECIFIED.,.F.,.F.)
B_SPLINE_CURVE_WITH_KNOTS((6,1,1,1,1,1,1,1,1,1,1,1,1,1,1,1,1,1,1,1,1,1,
1,1,1,1,1,1,1,1,1,1,1,1,1,1,1,1,1,1,1,1,1,1,1,1,1,1,1,1,1,1,1,1,1,1,1,1,
1,1,1,1,1,1,1,6),(0.,0.0153846153846154,0.0307692307692308,0.0461538461538462,
0.0615384615384615,0.0769230769230769,0.0923076923076923,0.107692307692308,
0.123076923076923,0.138461538461538,0.153846153846154,0.169230769230769,
0.184615384615385,0.2,0.215384615384615,0.230769230769231,0.246153846153846,
0.261538461538462,0.276923076923077,0.292307692307692,0.307692307692308,
0.323076923076923,0.338461538461538,0.353846153846154,0.369230769230769,
0.384615384615385,0.4,0.415384615384615,0.430769230769231,0.446153846153846,
0.461538461538462,0.476923076923077,0.492307692307692,0.507692307692308,
0.523076923076923,0.538461538461538,0.553846153846154,0.569230769230769,
0.584615384615384,0.6,0.615384615384615,0.63076923076923,0.646153846153846,
0.661538461538461,0.676923076923076,0.692307692307692,0.707692307692307,
0.723076923076922,0.738461538461538,0.753846153846153,0.769230769230768,
0.784615384615384,0.799999999999999,0.815384615384614,0.83076923076923,
0.846153846153845,0.86153846153846,0.876923076923076,0.892307692307691,
0.907692307692306,0.923076923076922,0.938461538461537,0.953846153846152,
0.969230769230768,0.984615384615383,1.),.UNSPECIFIED.)
CURVE()
GEOMETRIC_REPRESENTATION_ITEM()
RATIONAL_B_SPLINE_CURVE((1.,1.,1.,1.,1.,1.,1.,1.,1.,1.,1.,1.,1.,1.,1.,1.,
1.,1.,1.,1.,1.,1.,1.,1.,1.,1.,1.,1.,1.,1.,1.,1.,1.,1.,1.,1.,1.,1.,1.,1.,
1.,1.,1.,1.,1.,1.,1.,1.,1.,1.,1.,1.,1.,1.,1.,1.,1.,1.,1.,1.,1.,1.,1.,1.,
1.,1.,1.,1.,1.,1.))
REPRESENTATION_ITEM('')
);
#170=(
BOUNDED_CURVE()
B_SPLINE_CURVE(5,(#29650,#29651,#29652,#29653,#29654,#29655,#29656,#29657,
#29658,#29659,#29660,#29661,#29662,#29663,#29664,#29665,#29666,#29667,#29668,
#29669,#29670,#29671,#29672,#29673,#29674,#29675,#29676,#29677,#29678,#29679,
#29680,#29681,#29682,#29683,#29684,#29685,#29686,#29687,#29688,#29689,#29690,
#29691,#29692,#29693,#29694,#29695,#29696,#29697,#29698,#29699,#29700,#29701,
#29702,#29703,#29704,#29705,#29706,#29707,#29708,#29709,#29710,#29711,#29712,
#29713,#29714,#29715,#29716,#29717,#29718,#29719),.UNSPECIFIED.,.F.,.F.)
B_SPLINE_CURVE_WITH_KNOTS((6,1,1,1,1,1,1,1,1,1,1,1,1,1,1,1,1,1,1,1,1,1,
1,1,1,1,1,1,1,1,1,1,1,1,1,1,1,1,1,1,1,1,1,1,1,1,1,1,1,1,1,1,1,1,1,1,1,1,
1,1,1,1,1,1,1,6),(0.,0.0153846153846154,0.0307692307692308,0.0461538461538462,
0.0615384615384615,0.0769230769230769,0.0923076923076923,0.107692307692308,
0.123076923076923,0.138461538461538,0.153846153846154,0.169230769230769,
0.184615384615385,0.2,0.215384615384615,0.230769230769231,0.246153846153846,
0.261538461538462,0.276923076923077,0.292307692307692,0.307692307692308,
0.323076923076923,0.338461538461538,0.353846153846154,0.369230769230769,
0.384615384615385,0.4,0.415384615384615,0.430769230769231,0.446153846153846,
0.461538461538462,0.476923076923077,0.492307692307692,0.507692307692308,
0.523076923076923,0.538461538461538,0.553846153846154,0.569230769230769,
0.584615384615384,0.6,0.615384615384615,0.63076923076923,0.646153846153846,
0.661538461538461,0.676923076923076,0.692307692307692,0.707692307692307,
0.723076923076922,0.738461538461538,0.753846153846153,0.769230769230768,
0.784615384615384,0.799999999999999,0.815384615384614,0.83076923076923,
0.846153846153845,0.86153846153846,0.876923076923076,0.892307692307691,
0.907692307692306,0.923076923076922,0.938461538461537,0.953846153846152,
0.969230769230768,0.984615384615383,1.),.UNSPECIFIED.)
CURVE()
GEOMETRIC_REPRESENTATION_ITEM()
RATIONAL_B_SPLINE_CURVE((1.,1.,1.,1.,1.,1.,1.,1.,1.,1.,1.,1.,1.,1.,1.,1.,
1.,1.,1.,1.,1.,1.,1.,1.,1.,1.,1.,1.,1.,1.,1.,1.,1.,1.,1.,1.,1.,1.,1.,1.,
1.,1.,1.,1.,1.,1.,1.,1.,1.,1.,1.,1.,1.,1.,1.,1.,1.,1.,1.,1.,1.,1.,1.,1.,
1.,1.,1.,1.,1.,1.))
REPRESENTATION_ITEM('')
);
#171=(
BOUNDED_CURVE()
B_SPLINE_CURVE(5,(#29873,#29874,#29875,#29876,#29877,#29878,#29879,#29880,
#29881,#29882,#29883,#29884,#29885,#29886,#29887,#29888,#29889,#29890,#29891,
#29892,#29893,#29894,#29895,#29896,#29897,#29898,#29899,#29900,#29901,#29902,
#29903,#29904,#29905,#29906,#29907,#29908,#29909,#29910,#29911,#29912,#29913,
#29914,#29915,#29916,#29917,#29918,#29919,#29920,#29921,#29922,#29923,#29924,
#29925,#29926,#29927,#29928,#29929,#29930,#29931,#29932,#29933,#29934,#29935,
#29936,#29937,#29938,#29939,#29940,#29941,#29942),.UNSPECIFIED.,.F.,.F.)
B_SPLINE_CURVE_WITH_KNOTS((6,1,1,1,1,1,1,1,1,1,1,1,1,1,1,1,1,1,1,1,1,1,
1,1,1,1,1,1,1,1,1,1,1,1,1,1,1,1,1,1,1,1,1,1,1,1,1,1,1,1,1,1,1,1,1,1,1,1,
1,1,1,1,1,1,1,6),(-1.,-0.984615384615383,-0.969230769230768,-0.953846153846152,
-0.938461538461537,-0.923076923076922,-0.907692307692306,-0.892307692307691,
-0.876923076923076,-0.86153846153846,-0.846153846153845,-0.83076923076923,
-0.815384615384614,-0.799999999999999,-0.784615384615384,-0.769230769230768,
-0.753846153846153,-0.738461538461538,-0.723076923076922,-0.707692307692307,
-0.692307692307692,-0.676923076923076,-0.661538461538461,-0.646153846153846,
-0.63076923076923,-0.615384615384615,-0.6,-0.584615384615384,-0.569230769230769,
-0.553846153846154,-0.538461538461538,-0.523076923076923,-0.507692307692308,
-0.492307692307692,-0.476923076923077,-0.461538461538462,-0.446153846153846,
-0.430769230769231,-0.415384615384615,-0.4,-0.384615384615385,-0.369230769230769,
-0.353846153846154,-0.338461538461538,-0.323076923076923,-0.307692307692308,
-0.292307692307692,-0.276923076923077,-0.261538461538462,-0.246153846153846,
-0.230769230769231,-0.215384615384615,-0.2,-0.184615384615385,-0.169230769230769,
-0.153846153846154,-0.138461538461538,-0.123076923076923,-0.107692307692308,
-0.0923076923076923,-0.0769230769230769,-0.0615384615384615,-0.0461538461538462,
-0.0307692307692308,-0.0153846153846154,0.),.UNSPECIFIED.)
CURVE()
GEOMETRIC_REPRESENTATION_ITEM()
RATIONAL_B_SPLINE_CURVE((1.,1.,1.,1.,1.,1.,1.,1.,1.,1.,1.,1.,1.,1.,1.,1.,
1.,1.,1.,1.,1.,1.,1.,1.,1.,1.,1.,1.,1.,1.,1.,1.,1.,1.,1.,1.,1.,1.,1.,1.,
1.,1.,1.,1.,1.,1.,1.,1.,1.,1.,1.,1.,1.,1.,1.,1.,1.,1.,1.,1.,1.,1.,1.,1.,
1.,1.,1.,1.,1.,1.))
REPRESENTATION_ITEM('')
);
#172=(
BOUNDED_CURVE()
B_SPLINE_CURVE(5,(#30089,#30090,#30091,#30092,#30093,#30094,#30095,#30096,
#30097,#30098,#30099,#30100,#30101,#30102,#30103,#30104,#30105,#30106,#30107,
#30108,#30109,#30110,#30111,#30112,#30113,#30114,#30115,#30116,#30117,#30118,
#30119,#30120,#30121,#30122,#30123,#30124,#30125,#30126,#30127,#30128,#30129,
#30130,#30131,#30132,#30133,#30134,#30135,#30136,#30137,#30138,#30139,#30140,
#30141,#30142,#30143,#30144,#30145,#30146,#30147,#30148,#30149,#30150,#30151,
#30152,#30153,#30154,#30155,#30156,#30157,#30158),.UNSPECIFIED.,.F.,.F.)
B_SPLINE_CURVE_WITH_KNOTS((6,1,1,1,1,1,1,1,1,1,1,1,1,1,1,1,1,1,1,1,1,1,
1,1,1,1,1,1,1,1,1,1,1,1,1,1,1,1,1,1,1,1,1,1,1,1,1,1,1,1,1,1,1,1,1,1,1,1,
1,1,1,1,1,1,1,6),(-1.,-0.984615384615383,-0.969230769230768,-0.953846153846152,
-0.938461538461537,-0.923076923076922,-0.907692307692306,-0.892307692307691,
-0.876923076923076,-0.86153846153846,-0.846153846153845,-0.83076923076923,
-0.815384615384614,-0.799999999999999,-0.784615384615384,-0.769230769230768,
-0.753846153846153,-0.738461538461538,-0.723076923076922,-0.707692307692307,
-0.692307692307692,-0.676923076923076,-0.661538461538461,-0.646153846153846,
-0.63076923076923,-0.615384615384615,-0.6,-0.584615384615384,-0.569230769230769,
-0.553846153846154,-0.538461538461538,-0.523076923076923,-0.507692307692308,
-0.492307692307692,-0.476923076923077,-0.461538461538462,-0.446153846153846,
-0.430769230769231,-0.415384615384615,-0.4,-0.384615384615385,-0.369230769230769,
-0.353846153846154,-0.338461538461538,-0.323076923076923,-0.307692307692308,
-0.292307692307692,-0.276923076923077,-0.261538461538462,-0.246153846153846,
-0.230769230769231,-0.215384615384615,-0.2,-0.184615384615385,-0.169230769230769,
-0.153846153846154,-0.138461538461538,-0.123076923076923,-0.107692307692308,
-0.0923076923076923,-0.0769230769230769,-0.0615384615384615,-0.0461538461538462,
-0.0307692307692308,-0.0153846153846154,0.),.UNSPECIFIED.)
CURVE()
GEOMETRIC_REPRESENTATION_ITEM()
RATIONAL_B_SPLINE_CURVE((1.,1.,1.,1.,1.,1.,1.,1.,1.,1.,1.,1.,1.,1.,1.,1.,
1.,1.,1.,1.,1.,1.,1.,1.,1.,1.,1.,1.,1.,1.,1.,1.,1.,1.,1.,1.,1.,1.,1.,1.,
1.,1.,1.,1.,1.,1.,1.,1.,1.,1.,1.,1.,1.,1.,1.,1.,1.,1.,1.,1.,1.,1.,1.,1.,
1.,1.,1.,1.,1.,1.))
REPRESENTATION_ITEM('')
);
#173=(
BOUNDED_CURVE()
B_SPLINE_CURVE(5,(#30305,#30306,#30307,#30308,#30309,#30310,#30311,#30312,
#30313,#30314,#30315,#30316,#30317,#30318,#30319,#30320,#30321,#30322,#30323,
#30324,#30325,#30326,#30327,#30328,#30329,#30330,#30331,#30332,#30333,#30334,
#30335,#30336,#30337,#30338,#30339,#30340,#30341,#30342,#30343,#30344,#30345,
#30346,#30347,#30348,#30349,#30350,#30351,#30352,#30353,#30354,#30355,#30356,
#30357,#30358,#30359,#30360,#30361,#30362,#30363,#30364,#30365,#30366,#30367,
#30368,#30369,#30370,#30371,#30372,#30373,#30374),.UNSPECIFIED.,.F.,.F.)
B_SPLINE_CURVE_WITH_KNOTS((6,1,1,1,1,1,1,1,1,1,1,1,1,1,1,1,1,1,1,1,1,1,
1,1,1,1,1,1,1,1,1,1,1,1,1,1,1,1,1,1,1,1,1,1,1,1,1,1,1,1,1,1,1,1,1,1,1,1,
1,1,1,1,1,1,1,6),(-1.,-0.984615384615383,-0.969230769230768,-0.953846153846152,
-0.938461538461537,-0.923076923076922,-0.907692307692306,-0.892307692307691,
-0.876923076923076,-0.86153846153846,-0.846153846153845,-0.83076923076923,
-0.815384615384614,-0.799999999999999,-0.784615384615384,-0.769230769230768,
-0.753846153846153,-0.738461538461538,-0.723076923076922,-0.707692307692307,
-0.692307692307692,-0.676923076923076,-0.661538461538461,-0.646153846153846,
-0.63076923076923,-0.615384615384615,-0.6,-0.584615384615384,-0.569230769230769,
-0.553846153846154,-0.538461538461538,-0.523076923076923,-0.507692307692308,
-0.492307692307692,-0.476923076923077,-0.461538461538462,-0.446153846153846,
-0.430769230769231,-0.415384615384615,-0.4,-0.384615384615385,-0.369230769230769,
-0.353846153846154,-0.338461538461538,-0.323076923076923,-0.307692307692308,
-0.292307692307692,-0.276923076923077,-0.261538461538462,-0.246153846153846,
-0.230769230769231,-0.215384615384615,-0.2,-0.184615384615385,-0.169230769230769,
-0.153846153846154,-0.138461538461538,-0.123076923076923,-0.107692307692308,
-0.0923076923076923,-0.0769230769230769,-0.0615384615384615,-0.0461538461538462,
-0.0307692307692308,-0.0153846153846154,0.),.UNSPECIFIED.)
CURVE()
GEOMETRIC_REPRESENTATION_ITEM()
RATIONAL_B_SPLINE_CURVE((1.,1.,1.,1.,1.,1.,1.,1.,1.,1.,1.,1.,1.,1.,1.,1.,
1.,1.,1.,1.,1.,1.,1.,1.,1.,1.,1.,1.,1.,1.,1.,1.,1.,1.,1.,1.,1.,1.,1.,1.,
1.,1.,1.,1.,1.,1.,1.,1.,1.,1.,1.,1.,1.,1.,1.,1.,1.,1.,1.,1.,1.,1.,1.,1.,
1.,1.,1.,1.,1.,1.))
REPRESENTATION_ITEM('')
);
#174=(
BOUNDED_CURVE()
B_SPLINE_CURVE(5,(#30521,#30522,#30523,#30524,#30525,#30526,#30527,#30528,
#30529,#30530,#30531,#30532,#30533,#30534,#30535,#30536,#30537,#30538,#30539,
#30540,#30541,#30542,#30543,#30544,#30545,#30546,#30547,#30548,#30549,#30550,
#30551,#30552,#30553,#30554,#30555,#30556,#30557,#30558,#30559,#30560,#30561,
#30562,#30563,#30564,#30565,#30566,#30567,#30568,#30569,#30570,#30571,#30572,
#30573,#30574,#30575,#30576,#30577,#30578,#30579,#30580,#30581,#30582,#30583,
#30584,#30585,#30586,#30587,#30588,#30589,#30590),.UNSPECIFIED.,.F.,.F.)
B_SPLINE_CURVE_WITH_KNOTS((6,1,1,1,1,1,1,1,1,1,1,1,1,1,1,1,1,1,1,1,1,1,
1,1,1,1,1,1,1,1,1,1,1,1,1,1,1,1,1,1,1,1,1,1,1,1,1,1,1,1,1,1,1,1,1,1,1,1,
1,1,1,1,1,1,1,6),(-1.,-0.984615384615383,-0.969230769230768,-0.953846153846152,
-0.938461538461537,-0.923076923076922,-0.907692307692306,-0.892307692307691,
-0.876923076923076,-0.86153846153846,-0.846153846153845,-0.83076923076923,
-0.815384615384614,-0.799999999999999,-0.784615384615384,-0.769230769230768,
-0.753846153846153,-0.738461538461538,-0.723076923076922,-0.707692307692307,
-0.692307692307692,-0.676923076923076,-0.661538461538461,-0.646153846153846,
-0.63076923076923,-0.615384615384615,-0.6,-0.584615384615384,-0.569230769230769,
-0.553846153846154,-0.538461538461538,-0.523076923076923,-0.507692307692308,
-0.492307692307692,-0.476923076923077,-0.461538461538462,-0.446153846153846,
-0.430769230769231,-0.415384615384615,-0.4,-0.384615384615385,-0.369230769230769,
-0.353846153846154,-0.338461538461538,-0.323076923076923,-0.307692307692308,
-0.292307692307692,-0.276923076923077,-0.261538461538462,-0.246153846153846,
-0.230769230769231,-0.215384615384615,-0.2,-0.184615384615385,-0.169230769230769,
-0.153846153846154,-0.138461538461538,-0.123076923076923,-0.107692307692308,
-0.0923076923076923,-0.0769230769230769,-0.0615384615384615,-0.0461538461538462,
-0.0307692307692308,-0.0153846153846154,0.),.UNSPECIFIED.)
CURVE()
GEOMETRIC_REPRESENTATION_ITEM()
RATIONAL_B_SPLINE_CURVE((1.,1.,1.,1.,1.,1.,1.,1.,1.,1.,1.,1.,1.,1.,1.,1.,
1.,1.,1.,1.,1.,1.,1.,1.,1.,1.,1.,1.,1.,1.,1.,1.,1.,1.,1.,1.,1.,1.,1.,1.,
1.,1.,1.,1.,1.,1.,1.,1.,1.,1.,1.,1.,1.,1.,1.,1.,1.,1.,1.,1.,1.,1.,1.,1.,
1.,1.,1.,1.,1.,1.))
REPRESENTATION_ITEM('')
);
#175=(
BOUNDED_CURVE()
B_SPLINE_CURVE(5,(#30737,#30738,#30739,#30740,#30741,#30742,#30743,#30744,
#30745,#30746,#30747,#30748,#30749,#30750,#30751,#30752,#30753,#30754,#30755,
#30756,#30757,#30758,#30759,#30760,#30761,#30762,#30763,#30764,#30765,#30766,
#30767,#30768,#30769,#30770,#30771,#30772,#30773,#30774,#30775,#30776,#30777,
#30778,#30779,#30780,#30781,#30782,#30783,#30784,#30785,#30786,#30787,#30788,
#30789,#30790,#30791,#30792,#30793,#30794,#30795,#30796,#30797,#30798,#30799,
#30800,#30801,#30802,#30803,#30804,#30805,#30806),.UNSPECIFIED.,.F.,.F.)
B_SPLINE_CURVE_WITH_KNOTS((6,1,1,1,1,1,1,1,1,1,1,1,1,1,1,1,1,1,1,1,1,1,
1,1,1,1,1,1,1,1,1,1,1,1,1,1,1,1,1,1,1,1,1,1,1,1,1,1,1,1,1,1,1,1,1,1,1,1,
1,1,1,1,1,1,1,6),(-1.,-0.984615384615383,-0.969230769230768,-0.953846153846152,
-0.938461538461537,-0.923076923076922,-0.907692307692306,-0.892307692307691,
-0.876923076923076,-0.86153846153846,-0.846153846153845,-0.83076923076923,
-0.815384615384614,-0.799999999999999,-0.784615384615384,-0.769230769230768,
-0.753846153846153,-0.738461538461538,-0.723076923076922,-0.707692307692307,
-0.692307692307692,-0.676923076923076,-0.661538461538461,-0.646153846153846,
-0.63076923076923,-0.615384615384615,-0.6,-0.584615384615384,-0.569230769230769,
-0.553846153846154,-0.538461538461538,-0.523076923076923,-0.507692307692308,
-0.492307692307692,-0.476923076923077,-0.461538461538462,-0.446153846153846,
-0.430769230769231,-0.415384615384615,-0.4,-0.384615384615385,-0.369230769230769,
-0.353846153846154,-0.338461538461538,-0.323076923076923,-0.307692307692308,
-0.292307692307692,-0.276923076923077,-0.261538461538462,-0.246153846153846,
-0.230769230769231,-0.215384615384615,-0.2,-0.184615384615385,-0.169230769230769,
-0.153846153846154,-0.138461538461538,-0.123076923076923,-0.107692307692308,
-0.0923076923076923,-0.0769230769230769,-0.0615384615384615,-0.0461538461538462,
-0.0307692307692308,-0.0153846153846154,0.),.UNSPECIFIED.)
CURVE()
GEOMETRIC_REPRESENTATION_ITEM()
RATIONAL_B_SPLINE_CURVE((1.,1.,1.,1.,1.,1.,1.,1.,1.,1.,1.,1.,1.,1.,1.,1.,
1.,1.,1.,1.,1.,1.,1.,1.,1.,1.,1.,1.,1.,1.,1.,1.,1.,1.,1.,1.,1.,1.,1.,1.,
1.,1.,1.,1.,1.,1.,1.,1.,1.,1.,1.,1.,1.,1.,1.,1.,1.,1.,1.,1.,1.,1.,1.,1.,
1.,1.,1.,1.,1.,1.))
REPRESENTATION_ITEM('')
);
#176=(
BOUNDED_CURVE()
B_SPLINE_CURVE(5,(#30953,#30954,#30955,#30956,#30957,#30958,#30959,#30960,
#30961,#30962,#30963,#30964,#30965,#30966,#30967,#30968,#30969,#30970,#30971,
#30972,#30973,#30974,#30975,#30976,#30977,#30978,#30979,#30980,#30981,#30982,
#30983,#30984,#30985,#30986,#30987,#30988,#30989,#30990,#30991,#30992,#30993,
#30994,#30995,#30996,#30997,#30998,#30999,#31000,#31001,#31002,#31003,#31004,
#31005,#31006,#31007,#31008,#31009,#31010,#31011,#31012,#31013,#31014,#31015,
#31016,#31017,#31018,#31019,#31020,#31021,#31022),.UNSPECIFIED.,.F.,.F.)
B_SPLINE_CURVE_WITH_KNOTS((6,1,1,1,1,1,1,1,1,1,1,1,1,1,1,1,1,1,1,1,1,1,
1,1,1,1,1,1,1,1,1,1,1,1,1,1,1,1,1,1,1,1,1,1,1,1,1,1,1,1,1,1,1,1,1,1,1,1,
1,1,1,1,1,1,1,6),(-1.,-0.984615384615383,-0.969230769230768,-0.953846153846152,
-0.938461538461537,-0.923076923076922,-0.907692307692306,-0.892307692307691,
-0.876923076923076,-0.86153846153846,-0.846153846153845,-0.83076923076923,
-0.815384615384614,-0.799999999999999,-0.784615384615384,-0.769230769230768,
-0.753846153846153,-0.738461538461538,-0.723076923076922,-0.707692307692307,
-0.692307692307692,-0.676923076923076,-0.661538461538461,-0.646153846153846,
-0.63076923076923,-0.615384615384615,-0.6,-0.584615384615384,-0.569230769230769,
-0.553846153846154,-0.538461538461538,-0.523076923076923,-0.507692307692308,
-0.492307692307692,-0.476923076923077,-0.461538461538462,-0.446153846153846,
-0.430769230769231,-0.415384615384615,-0.4,-0.384615384615385,-0.369230769230769,
-0.353846153846154,-0.338461538461538,-0.323076923076923,-0.307692307692308,
-0.292307692307692,-0.276923076923077,-0.261538461538462,-0.246153846153846,
-0.230769230769231,-0.215384615384615,-0.2,-0.184615384615385,-0.169230769230769,
-0.153846153846154,-0.138461538461538,-0.123076923076923,-0.107692307692308,
-0.0923076923076923,-0.0769230769230769,-0.0615384615384615,-0.0461538461538462,
-0.0307692307692308,-0.0153846153846154,0.),.UNSPECIFIED.)
CURVE()
GEOMETRIC_REPRESENTATION_ITEM()
RATIONAL_B_SPLINE_CURVE((1.,1.,1.,1.,1.,1.,1.,1.,1.,1.,1.,1.,1.,1.,1.,1.,
1.,1.,1.,1.,1.,1.,1.,1.,1.,1.,1.,1.,1.,1.,1.,1.,1.,1.,1.,1.,1.,1.,1.,1.,
1.,1.,1.,1.,1.,1.,1.,1.,1.,1.,1.,1.,1.,1.,1.,1.,1.,1.,1.,1.,1.,1.,1.,1.,
1.,1.,1.,1.,1.,1.))
REPRESENTATION_ITEM('')
);
#177=(
BOUNDED_CURVE()
B_SPLINE_CURVE(5,(#31169,#31170,#31171,#31172,#31173,#31174,#31175,#31176,
#31177,#31178,#31179,#31180,#31181,#31182,#31183,#31184,#31185,#31186,#31187,
#31188,#31189,#31190,#31191,#31192,#31193,#31194,#31195,#31196,#31197,#31198,
#31199,#31200,#31201,#31202,#31203,#31204,#31205,#31206,#31207,#31208,#31209,
#31210,#31211,#31212,#31213,#31214,#31215,#31216,#31217,#31218,#31219,#31220,
#31221,#31222,#31223,#31224,#31225,#31226,#31227,#31228,#31229,#31230,#31231,
#31232,#31233,#31234,#31235,#31236,#31237,#31238),.UNSPECIFIED.,.F.,.F.)
B_SPLINE_CURVE_WITH_KNOTS((6,1,1,1,1,1,1,1,1,1,1,1,1,1,1,1,1,1,1,1,1,1,
1,1,1,1,1,1,1,1,1,1,1,1,1,1,1,1,1,1,1,1,1,1,1,1,1,1,1,1,1,1,1,1,1,1,1,1,
1,1,1,1,1,1,1,6),(-1.,-0.984615384615383,-0.969230769230768,-0.953846153846152,
-0.938461538461537,-0.923076923076922,-0.907692307692306,-0.892307692307691,
-0.876923076923076,-0.86153846153846,-0.846153846153845,-0.83076923076923,
-0.815384615384614,-0.799999999999999,-0.784615384615384,-0.769230769230768,
-0.753846153846153,-0.738461538461538,-0.723076923076922,-0.707692307692307,
-0.692307692307692,-0.676923076923076,-0.661538461538461,-0.646153846153846,
-0.63076923076923,-0.615384615384615,-0.6,-0.584615384615384,-0.569230769230769,
-0.553846153846154,-0.538461538461538,-0.523076923076923,-0.507692307692308,
-0.492307692307692,-0.476923076923077,-0.461538461538462,-0.446153846153846,
-0.430769230769231,-0.415384615384615,-0.4,-0.384615384615385,-0.369230769230769,
-0.353846153846154,-0.338461538461538,-0.323076923076923,-0.307692307692308,
-0.292307692307692,-0.276923076923077,-0.261538461538462,-0.246153846153846,
-0.230769230769231,-0.215384615384615,-0.2,-0.184615384615385,-0.169230769230769,
-0.153846153846154,-0.138461538461538,-0.123076923076923,-0.107692307692308,
-0.0923076923076923,-0.0769230769230769,-0.0615384615384615,-0.0461538461538462,
-0.0307692307692308,-0.0153846153846154,0.),.UNSPECIFIED.)
CURVE()
GEOMETRIC_REPRESENTATION_ITEM()
RATIONAL_B_SPLINE_CURVE((1.,1.,1.,1.,1.,1.,1.,1.,1.,1.,1.,1.,1.,1.,1.,1.,
1.,1.,1.,1.,1.,1.,1.,1.,1.,1.,1.,1.,1.,1.,1.,1.,1.,1.,1.,1.,1.,1.,1.,1.,
1.,1.,1.,1.,1.,1.,1.,1.,1.,1.,1.,1.,1.,1.,1.,1.,1.,1.,1.,1.,1.,1.,1.,1.,
1.,1.,1.,1.,1.,1.))
REPRESENTATION_ITEM('')
);
#178=(
BOUNDED_CURVE()
B_SPLINE_CURVE(5,(#31385,#31386,#31387,#31388,#31389,#31390,#31391,#31392,
#31393,#31394,#31395,#31396,#31397,#31398,#31399,#31400,#31401,#31402,#31403,
#31404,#31405,#31406,#31407,#31408,#31409,#31410,#31411,#31412,#31413,#31414,
#31415,#31416,#31417,#31418,#31419,#31420,#31421,#31422,#31423,#31424,#31425,
#31426,#31427,#31428,#31429,#31430,#31431,#31432,#31433,#31434,#31435,#31436,
#31437,#31438,#31439,#31440,#31441,#31442,#31443,#31444,#31445,#31446,#31447,
#31448,#31449,#31450,#31451,#31452,#31453,#31454),.UNSPECIFIED.,.F.,.F.)
B_SPLINE_CURVE_WITH_KNOTS((6,1,1,1,1,1,1,1,1,1,1,1,1,1,1,1,1,1,1,1,1,1,
1,1,1,1,1,1,1,1,1,1,1,1,1,1,1,1,1,1,1,1,1,1,1,1,1,1,1,1,1,1,1,1,1,1,1,1,
1,1,1,1,1,1,1,6),(-1.,-0.984615384615383,-0.969230769230768,-0.953846153846152,
-0.938461538461537,-0.923076923076922,-0.907692307692306,-0.892307692307691,
-0.876923076923076,-0.86153846153846,-0.846153846153845,-0.83076923076923,
-0.815384615384614,-0.799999999999999,-0.784615384615384,-0.769230769230768,
-0.753846153846153,-0.738461538461538,-0.723076923076922,-0.707692307692307,
-0.692307692307692,-0.676923076923076,-0.661538461538461,-0.646153846153846,
-0.63076923076923,-0.615384615384615,-0.6,-0.584615384615384,-0.569230769230769,
-0.553846153846154,-0.538461538461538,-0.523076923076923,-0.507692307692308,
-0.492307692307692,-0.476923076923077,-0.461538461538462,-0.446153846153846,
-0.430769230769231,-0.415384615384615,-0.4,-0.384615384615385,-0.369230769230769,
-0.353846153846154,-0.338461538461538,-0.323076923076923,-0.307692307692308,
-0.292307692307692,-0.276923076923077,-0.261538461538462,-0.246153846153846,
-0.230769230769231,-0.215384615384615,-0.2,-0.184615384615385,-0.169230769230769,
-0.153846153846154,-0.138461538461538,-0.123076923076923,-0.107692307692308,
-0.0923076923076923,-0.0769230769230769,-0.0615384615384615,-0.0461538461538462,
-0.0307692307692308,-0.0153846153846154,0.),.UNSPECIFIED.)
CURVE()
GEOMETRIC_REPRESENTATION_ITEM()
RATIONAL_B_SPLINE_CURVE((1.,1.,1.,1.,1.,1.,1.,1.,1.,1.,1.,1.,1.,1.,1.,1.,
1.,1.,1.,1.,1.,1.,1.,1.,1.,1.,1.,1.,1.,1.,1.,1.,1.,1.,1.,1.,1.,1.,1.,1.,
1.,1.,1.,1.,1.,1.,1.,1.,1.,1.,1.,1.,1.,1.,1.,1.,1.,1.,1.,1.,1.,1.,1.,1.,
1.,1.,1.,1.,1.,1.))
REPRESENTATION_ITEM('')
);
#179=(
BOUNDED_CURVE()
B_SPLINE_CURVE(5,(#31601,#31602,#31603,#31604,#31605,#31606,#31607,#31608,
#31609,#31610,#31611,#31612,#31613,#31614,#31615,#31616,#31617,#31618,#31619,
#31620,#31621,#31622,#31623,#31624,#31625,#31626,#31627,#31628,#31629,#31630,
#31631,#31632,#31633,#31634,#31635,#31636,#31637,#31638,#31639,#31640,#31641,
#31642,#31643,#31644,#31645,#31646,#31647,#31648,#31649,#31650,#31651,#31652,
#31653,#31654,#31655,#31656,#31657,#31658,#31659,#31660,#31661,#31662,#31663,
#31664,#31665,#31666,#31667,#31668,#31669,#31670),.UNSPECIFIED.,.F.,.F.)
B_SPLINE_CURVE_WITH_KNOTS((6,1,1,1,1,1,1,1,1,1,1,1,1,1,1,1,1,1,1,1,1,1,
1,1,1,1,1,1,1,1,1,1,1,1,1,1,1,1,1,1,1,1,1,1,1,1,1,1,1,1,1,1,1,1,1,1,1,1,
1,1,1,1,1,1,1,6),(-1.,-0.984615384615383,-0.969230769230768,-0.953846153846152,
-0.938461538461537,-0.923076923076922,-0.907692307692306,-0.892307692307691,
-0.876923076923076,-0.86153846153846,-0.846153846153845,-0.83076923076923,
-0.815384615384614,-0.799999999999999,-0.784615384615384,-0.769230769230768,
-0.753846153846153,-0.738461538461538,-0.723076923076922,-0.707692307692307,
-0.692307692307692,-0.676923076923076,-0.661538461538461,-0.646153846153846,
-0.63076923076923,-0.615384615384615,-0.6,-0.584615384615384,-0.569230769230769,
-0.553846153846154,-0.538461538461538,-0.523076923076923,-0.507692307692308,
-0.492307692307692,-0.476923076923077,-0.461538461538462,-0.446153846153846,
-0.430769230769231,-0.415384615384615,-0.4,-0.384615384615385,-0.369230769230769,
-0.353846153846154,-0.338461538461538,-0.323076923076923,-0.307692307692308,
-0.292307692307692,-0.276923076923077,-0.261538461538462,-0.246153846153846,
-0.230769230769231,-0.215384615384615,-0.2,-0.184615384615385,-0.169230769230769,
-0.153846153846154,-0.138461538461538,-0.123076923076923,-0.107692307692308,
-0.0923076923076923,-0.0769230769230769,-0.0615384615384615,-0.0461538461538462,
-0.0307692307692308,-0.0153846153846154,0.),.UNSPECIFIED.)
CURVE()
GEOMETRIC_REPRESENTATION_ITEM()
RATIONAL_B_SPLINE_CURVE((1.,1.,1.,1.,1.,1.,1.,1.,1.,1.,1.,1.,1.,1.,1.,1.,
1.,1.,1.,1.,1.,1.,1.,1.,1.,1.,1.,1.,1.,1.,1.,1.,1.,1.,1.,1.,1.,1.,1.,1.,
1.,1.,1.,1.,1.,1.,1.,1.,1.,1.,1.,1.,1.,1.,1.,1.,1.,1.,1.,1.,1.,1.,1.,1.,
1.,1.,1.,1.,1.,1.))
REPRESENTATION_ITEM('')
);
#180=(
BOUNDED_CURVE()
B_SPLINE_CURVE(5,(#31817,#31818,#31819,#31820,#31821,#31822,#31823,#31824,
#31825,#31826,#31827,#31828,#31829,#31830,#31831,#31832,#31833,#31834,#31835,
#31836,#31837,#31838,#31839,#31840,#31841,#31842,#31843,#31844,#31845,#31846,
#31847,#31848,#31849,#31850,#31851,#31852,#31853,#31854,#31855,#31856,#31857,
#31858,#31859,#31860,#31861,#31862,#31863,#31864,#31865,#31866,#31867,#31868,
#31869,#31870,#31871,#31872,#31873,#31874,#31875,#31876,#31877,#31878,#31879,
#31880,#31881,#31882,#31883,#31884,#31885,#31886),.UNSPECIFIED.,.F.,.F.)
B_SPLINE_CURVE_WITH_KNOTS((6,1,1,1,1,1,1,1,1,1,1,1,1,1,1,1,1,1,1,1,1,1,
1,1,1,1,1,1,1,1,1,1,1,1,1,1,1,1,1,1,1,1,1,1,1,1,1,1,1,1,1,1,1,1,1,1,1,1,
1,1,1,1,1,1,1,6),(-1.,-0.984615384615383,-0.969230769230768,-0.953846153846152,
-0.938461538461537,-0.923076923076922,-0.907692307692306,-0.892307692307691,
-0.876923076923076,-0.86153846153846,-0.846153846153845,-0.83076923076923,
-0.815384615384614,-0.799999999999999,-0.784615384615384,-0.769230769230768,
-0.753846153846153,-0.738461538461538,-0.723076923076922,-0.707692307692307,
-0.692307692307692,-0.676923076923076,-0.661538461538461,-0.646153846153846,
-0.63076923076923,-0.615384615384615,-0.6,-0.584615384615384,-0.569230769230769,
-0.553846153846154,-0.538461538461538,-0.523076923076923,-0.507692307692308,
-0.492307692307692,-0.476923076923077,-0.461538461538462,-0.446153846153846,
-0.430769230769231,-0.415384615384615,-0.4,-0.384615384615385,-0.369230769230769,
-0.353846153846154,-0.338461538461538,-0.323076923076923,-0.307692307692308,
-0.292307692307692,-0.276923076923077,-0.261538461538462,-0.246153846153846,
-0.230769230769231,-0.215384615384615,-0.2,-0.184615384615385,-0.169230769230769,
-0.153846153846154,-0.138461538461538,-0.123076923076923,-0.107692307692308,
-0.0923076923076923,-0.0769230769230769,-0.0615384615384615,-0.0461538461538462,
-0.0307692307692308,-0.0153846153846154,0.),.UNSPECIFIED.)
CURVE()
GEOMETRIC_REPRESENTATION_ITEM()
RATIONAL_B_SPLINE_CURVE((1.,1.,1.,1.,1.,1.,1.,1.,1.,1.,1.,1.,1.,1.,1.,1.,
1.,1.,1.,1.,1.,1.,1.,1.,1.,1.,1.,1.,1.,1.,1.,1.,1.,1.,1.,1.,1.,1.,1.,1.,
1.,1.,1.,1.,1.,1.,1.,1.,1.,1.,1.,1.,1.,1.,1.,1.,1.,1.,1.,1.,1.,1.,1.,1.,
1.,1.,1.,1.,1.,1.))
REPRESENTATION_ITEM('')
);
#181=(
BOUNDED_CURVE()
B_SPLINE_CURVE(5,(#32033,#32034,#32035,#32036,#32037,#32038,#32039,#32040,
#32041,#32042,#32043,#32044,#32045,#32046,#32047,#32048,#32049,#32050,#32051,
#32052,#32053,#32054,#32055,#32056,#32057,#32058,#32059,#32060,#32061,#32062,
#32063,#32064,#32065,#32066,#32067,#32068,#32069,#32070,#32071,#32072,#32073,
#32074,#32075,#32076,#32077,#32078,#32079,#32080,#32081,#32082,#32083,#32084,
#32085,#32086,#32087,#32088,#32089,#32090,#32091,#32092,#32093,#32094,#32095,
#32096,#32097,#32098,#32099,#32100,#32101,#32102),.UNSPECIFIED.,.F.,.F.)
B_SPLINE_CURVE_WITH_KNOTS((6,1,1,1,1,1,1,1,1,1,1,1,1,1,1,1,1,1,1,1,1,1,
1,1,1,1,1,1,1,1,1,1,1,1,1,1,1,1,1,1,1,1,1,1,1,1,1,1,1,1,1,1,1,1,1,1,1,1,
1,1,1,1,1,1,1,6),(-1.,-0.984615384615383,-0.969230769230768,-0.953846153846152,
-0.938461538461537,-0.923076923076922,-0.907692307692306,-0.892307692307691,
-0.876923076923076,-0.86153846153846,-0.846153846153845,-0.83076923076923,
-0.815384615384614,-0.799999999999999,-0.784615384615384,-0.769230769230768,
-0.753846153846153,-0.738461538461538,-0.723076923076922,-0.707692307692307,
-0.692307692307692,-0.676923076923076,-0.661538461538461,-0.646153846153846,
-0.63076923076923,-0.615384615384615,-0.6,-0.584615384615384,-0.569230769230769,
-0.553846153846154,-0.538461538461538,-0.523076923076923,-0.507692307692308,
-0.492307692307692,-0.476923076923077,-0.461538461538462,-0.446153846153846,
-0.430769230769231,-0.415384615384615,-0.4,-0.384615384615385,-0.369230769230769,
-0.353846153846154,-0.338461538461538,-0.323076923076923,-0.307692307692308,
-0.292307692307692,-0.276923076923077,-0.261538461538462,-0.246153846153846,
-0.230769230769231,-0.215384615384615,-0.2,-0.184615384615385,-0.169230769230769,
-0.153846153846154,-0.138461538461538,-0.123076923076923,-0.107692307692308,
-0.0923076923076923,-0.0769230769230769,-0.0615384615384615,-0.0461538461538462,
-0.0307692307692308,-0.0153846153846154,0.),.UNSPECIFIED.)
CURVE()
GEOMETRIC_REPRESENTATION_ITEM()
RATIONAL_B_SPLINE_CURVE((1.,1.,1.,1.,1.,1.,1.,1.,1.,1.,1.,1.,1.,1.,1.,1.,
1.,1.,1.,1.,1.,1.,1.,1.,1.,1.,1.,1.,1.,1.,1.,1.,1.,1.,1.,1.,1.,1.,1.,1.,
1.,1.,1.,1.,1.,1.,1.,1.,1.,1.,1.,1.,1.,1.,1.,1.,1.,1.,1.,1.,1.,1.,1.,1.,
1.,1.,1.,1.,1.,1.))
REPRESENTATION_ITEM('')
);
#182=(
BOUNDED_CURVE()
B_SPLINE_CURVE(5,(#32249,#32250,#32251,#32252,#32253,#32254,#32255,#32256,
#32257,#32258,#32259,#32260,#32261,#32262,#32263,#32264,#32265,#32266,#32267,
#32268,#32269,#32270,#32271,#32272,#32273,#32274,#32275,#32276,#32277,#32278,
#32279,#32280,#32281,#32282,#32283,#32284,#32285,#32286,#32287,#32288,#32289,
#32290,#32291,#32292,#32293,#32294,#32295,#32296,#32297,#32298,#32299,#32300,
#32301,#32302,#32303,#32304,#32305,#32306,#32307,#32308,#32309,#32310,#32311,
#32312,#32313,#32314,#32315,#32316,#32317,#32318),.UNSPECIFIED.,.F.,.F.)
B_SPLINE_CURVE_WITH_KNOTS((6,1,1,1,1,1,1,1,1,1,1,1,1,1,1,1,1,1,1,1,1,1,
1,1,1,1,1,1,1,1,1,1,1,1,1,1,1,1,1,1,1,1,1,1,1,1,1,1,1,1,1,1,1,1,1,1,1,1,
1,1,1,1,1,1,1,6),(-1.,-0.984615384615383,-0.969230769230768,-0.953846153846152,
-0.938461538461537,-0.923076923076922,-0.907692307692306,-0.892307692307691,
-0.876923076923076,-0.86153846153846,-0.846153846153845,-0.83076923076923,
-0.815384615384614,-0.799999999999999,-0.784615384615384,-0.769230769230768,
-0.753846153846153,-0.738461538461538,-0.723076923076922,-0.707692307692307,
-0.692307692307692,-0.676923076923076,-0.661538461538461,-0.646153846153846,
-0.63076923076923,-0.615384615384615,-0.6,-0.584615384615384,-0.569230769230769,
-0.553846153846154,-0.538461538461538,-0.523076923076923,-0.507692307692308,
-0.492307692307692,-0.476923076923077,-0.461538461538462,-0.446153846153846,
-0.430769230769231,-0.415384615384615,-0.4,-0.384615384615385,-0.369230769230769,
-0.353846153846154,-0.338461538461538,-0.323076923076923,-0.307692307692308,
-0.292307692307692,-0.276923076923077,-0.261538461538462,-0.246153846153846,
-0.230769230769231,-0.215384615384615,-0.2,-0.184615384615385,-0.169230769230769,
-0.153846153846154,-0.138461538461538,-0.123076923076923,-0.107692307692308,
-0.0923076923076923,-0.0769230769230769,-0.0615384615384615,-0.0461538461538462,
-0.0307692307692308,-0.0153846153846154,0.),.UNSPECIFIED.)
CURVE()
GEOMETRIC_REPRESENTATION_ITEM()
RATIONAL_B_SPLINE_CURVE((1.,1.,1.,1.,1.,1.,1.,1.,1.,1.,1.,1.,1.,1.,1.,1.,
1.,1.,1.,1.,1.,1.,1.,1.,1.,1.,1.,1.,1.,1.,1.,1.,1.,1.,1.,1.,1.,1.,1.,1.,
1.,1.,1.,1.,1.,1.,1.,1.,1.,1.,1.,1.,1.,1.,1.,1.,1.,1.,1.,1.,1.,1.,1.,1.,
1.,1.,1.,1.,1.,1.))
REPRESENTATION_ITEM('')
);
#183=(
BOUNDED_CURVE()
B_SPLINE_CURVE(5,(#32465,#32466,#32467,#32468,#32469,#32470,#32471,#32472,
#32473,#32474,#32475,#32476,#32477,#32478,#32479,#32480,#32481,#32482,#32483,
#32484,#32485,#32486,#32487,#32488,#32489,#32490,#32491,#32492,#32493,#32494,
#32495,#32496,#32497,#32498,#32499,#32500,#32501,#32502,#32503,#32504,#32505,
#32506,#32507,#32508,#32509,#32510,#32511,#32512,#32513,#32514,#32515,#32516,
#32517,#32518,#32519,#32520,#32521,#32522,#32523,#32524,#32525,#32526,#32527,
#32528,#32529,#32530,#32531,#32532,#32533,#32534),.UNSPECIFIED.,.F.,.F.)
B_SPLINE_CURVE_WITH_KNOTS((6,1,1,1,1,1,1,1,1,1,1,1,1,1,1,1,1,1,1,1,1,1,
1,1,1,1,1,1,1,1,1,1,1,1,1,1,1,1,1,1,1,1,1,1,1,1,1,1,1,1,1,1,1,1,1,1,1,1,
1,1,1,1,1,1,1,6),(-1.,-0.984615384615383,-0.969230769230768,-0.953846153846152,
-0.938461538461537,-0.923076923076922,-0.907692307692306,-0.892307692307691,
-0.876923076923076,-0.86153846153846,-0.846153846153845,-0.83076923076923,
-0.815384615384614,-0.799999999999999,-0.784615384615384,-0.769230769230768,
-0.753846153846153,-0.738461538461538,-0.723076923076922,-0.707692307692307,
-0.692307692307692,-0.676923076923076,-0.661538461538461,-0.646153846153846,
-0.63076923076923,-0.615384615384615,-0.6,-0.584615384615384,-0.569230769230769,
-0.553846153846154,-0.538461538461538,-0.523076923076923,-0.507692307692308,
-0.492307692307692,-0.476923076923077,-0.461538461538462,-0.446153846153846,
-0.430769230769231,-0.415384615384615,-0.4,-0.384615384615385,-0.369230769230769,
-0.353846153846154,-0.338461538461538,-0.323076923076923,-0.307692307692308,
-0.292307692307692,-0.276923076923077,-0.261538461538462,-0.246153846153846,
-0.230769230769231,-0.215384615384615,-0.2,-0.184615384615385,-0.169230769230769,
-0.153846153846154,-0.138461538461538,-0.123076923076923,-0.107692307692308,
-0.0923076923076923,-0.0769230769230769,-0.0615384615384615,-0.0461538461538462,
-0.0307692307692308,-0.0153846153846154,0.),.UNSPECIFIED.)
CURVE()
GEOMETRIC_REPRESENTATION_ITEM()
RATIONAL_B_SPLINE_CURVE((1.,1.,1.,1.,1.,1.,1.,1.,1.,1.,1.,1.,1.,1.,1.,1.,
1.,1.,1.,1.,1.,1.,1.,1.,1.,1.,1.,1.,1.,1.,1.,1.,1.,1.,1.,1.,1.,1.,1.,1.,
1.,1.,1.,1.,1.,1.,1.,1.,1.,1.,1.,1.,1.,1.,1.,1.,1.,1.,1.,1.,1.,1.,1.,1.,
1.,1.,1.,1.,1.,1.))
REPRESENTATION_ITEM('')
);
#184=(
BOUNDED_CURVE()
B_SPLINE_CURVE(5,(#32681,#32682,#32683,#32684,#32685,#32686,#32687,#32688,
#32689,#32690,#32691,#32692,#32693,#32694,#32695,#32696,#32697,#32698,#32699,
#32700,#32701,#32702,#32703,#32704,#32705,#32706,#32707,#32708,#32709,#32710,
#32711,#32712,#32713,#32714,#32715,#32716,#32717,#32718,#32719,#32720,#32721,
#32722,#32723,#32724,#32725,#32726,#32727,#32728,#32729,#32730,#32731,#32732,
#32733,#32734,#32735,#32736,#32737,#32738,#32739,#32740,#32741,#32742,#32743,
#32744,#32745,#32746,#32747,#32748,#32749,#32750),.UNSPECIFIED.,.F.,.F.)
B_SPLINE_CURVE_WITH_KNOTS((6,1,1,1,1,1,1,1,1,1,1,1,1,1,1,1,1,1,1,1,1,1,
1,1,1,1,1,1,1,1,1,1,1,1,1,1,1,1,1,1,1,1,1,1,1,1,1,1,1,1,1,1,1,1,1,1,1,1,
1,1,1,1,1,1,1,6),(-1.,-0.984615384615383,-0.969230769230768,-0.953846153846152,
-0.938461538461537,-0.923076923076922,-0.907692307692306,-0.892307692307691,
-0.876923076923076,-0.86153846153846,-0.846153846153845,-0.83076923076923,
-0.815384615384614,-0.799999999999999,-0.784615384615384,-0.769230769230768,
-0.753846153846153,-0.738461538461538,-0.723076923076922,-0.707692307692307,
-0.692307692307692,-0.676923076923076,-0.661538461538461,-0.646153846153846,
-0.63076923076923,-0.615384615384615,-0.6,-0.584615384615384,-0.569230769230769,
-0.553846153846154,-0.538461538461538,-0.523076923076923,-0.507692307692308,
-0.492307692307692,-0.476923076923077,-0.461538461538462,-0.446153846153846,
-0.430769230769231,-0.415384615384615,-0.4,-0.384615384615385,-0.369230769230769,
-0.353846153846154,-0.338461538461538,-0.323076923076923,-0.307692307692308,
-0.292307692307692,-0.276923076923077,-0.261538461538462,-0.246153846153846,
-0.230769230769231,-0.215384615384615,-0.2,-0.184615384615385,-0.169230769230769,
-0.153846153846154,-0.138461538461538,-0.123076923076923,-0.107692307692308,
-0.0923076923076923,-0.0769230769230769,-0.0615384615384615,-0.0461538461538462,
-0.0307692307692308,-0.0153846153846154,0.),.UNSPECIFIED.)
CURVE()
GEOMETRIC_REPRESENTATION_ITEM()
RATIONAL_B_SPLINE_CURVE((1.,1.,1.,1.,1.,1.,1.,1.,1.,1.,1.,1.,1.,1.,1.,1.,
1.,1.,1.,1.,1.,1.,1.,1.,1.,1.,1.,1.,1.,1.,1.,1.,1.,1.,1.,1.,1.,1.,1.,1.,
1.,1.,1.,1.,1.,1.,1.,1.,1.,1.,1.,1.,1.,1.,1.,1.,1.,1.,1.,1.,1.,1.,1.,1.,
1.,1.,1.,1.,1.,1.))
REPRESENTATION_ITEM('')
);
#185=(
BOUNDED_CURVE()
B_SPLINE_CURVE(5,(#32897,#32898,#32899,#32900,#32901,#32902,#32903,#32904,
#32905,#32906,#32907,#32908,#32909,#32910,#32911,#32912,#32913,#32914,#32915,
#32916,#32917,#32918,#32919,#32920,#32921,#32922,#32923,#32924,#32925,#32926,
#32927,#32928,#32929,#32930,#32931,#32932,#32933,#32934,#32935,#32936,#32937,
#32938,#32939,#32940,#32941,#32942,#32943,#32944,#32945,#32946,#32947,#32948,
#32949,#32950,#32951,#32952,#32953,#32954,#32955,#32956,#32957,#32958,#32959,
#32960,#32961,#32962,#32963,#32964,#32965,#32966),.UNSPECIFIED.,.F.,.F.)
B_SPLINE_CURVE_WITH_KNOTS((6,1,1,1,1,1,1,1,1,1,1,1,1,1,1,1,1,1,1,1,1,1,
1,1,1,1,1,1,1,1,1,1,1,1,1,1,1,1,1,1,1,1,1,1,1,1,1,1,1,1,1,1,1,1,1,1,1,1,
1,1,1,1,1,1,1,6),(-1.,-0.984615384615383,-0.969230769230768,-0.953846153846152,
-0.938461538461537,-0.923076923076922,-0.907692307692306,-0.892307692307691,
-0.876923076923076,-0.86153846153846,-0.846153846153845,-0.83076923076923,
-0.815384615384614,-0.799999999999999,-0.784615384615384,-0.769230769230768,
-0.753846153846153,-0.738461538461538,-0.723076923076922,-0.707692307692307,
-0.692307692307692,-0.676923076923076,-0.661538461538461,-0.646153846153846,
-0.63076923076923,-0.615384615384615,-0.6,-0.584615384615384,-0.569230769230769,
-0.553846153846154,-0.538461538461538,-0.523076923076923,-0.507692307692308,
-0.492307692307692,-0.476923076923077,-0.461538461538462,-0.446153846153846,
-0.430769230769231,-0.415384615384615,-0.4,-0.384615384615385,-0.369230769230769,
-0.353846153846154,-0.338461538461538,-0.323076923076923,-0.307692307692308,
-0.292307692307692,-0.276923076923077,-0.261538461538462,-0.246153846153846,
-0.230769230769231,-0.215384615384615,-0.2,-0.184615384615385,-0.169230769230769,
-0.153846153846154,-0.138461538461538,-0.123076923076923,-0.107692307692308,
-0.0923076923076923,-0.0769230769230769,-0.0615384615384615,-0.0461538461538462,
-0.0307692307692308,-0.0153846153846154,0.),.UNSPECIFIED.)
CURVE()
GEOMETRIC_REPRESENTATION_ITEM()
RATIONAL_B_SPLINE_CURVE((1.,1.,1.,1.,1.,1.,1.,1.,1.,1.,1.,1.,1.,1.,1.,1.,
1.,1.,1.,1.,1.,1.,1.,1.,1.,1.,1.,1.,1.,1.,1.,1.,1.,1.,1.,1.,1.,1.,1.,1.,
1.,1.,1.,1.,1.,1.,1.,1.,1.,1.,1.,1.,1.,1.,1.,1.,1.,1.,1.,1.,1.,1.,1.,1.,
1.,1.,1.,1.,1.,1.))
REPRESENTATION_ITEM('')
);
#186=(
BOUNDED_CURVE()
B_SPLINE_CURVE(5,(#33113,#33114,#33115,#33116,#33117,#33118,#33119,#33120,
#33121,#33122,#33123,#33124,#33125,#33126,#33127,#33128,#33129,#33130,#33131,
#33132,#33133,#33134,#33135,#33136,#33137,#33138,#33139,#33140,#33141,#33142,
#33143,#33144,#33145,#33146,#33147,#33148,#33149,#33150,#33151,#33152,#33153,
#33154,#33155,#33156,#33157,#33158,#33159,#33160,#33161,#33162,#33163,#33164,
#33165,#33166,#33167,#33168,#33169,#33170,#33171,#33172,#33173,#33174,#33175,
#33176,#33177,#33178,#33179,#33180,#33181,#33182),.UNSPECIFIED.,.F.,.F.)
B_SPLINE_CURVE_WITH_KNOTS((6,1,1,1,1,1,1,1,1,1,1,1,1,1,1,1,1,1,1,1,1,1,
1,1,1,1,1,1,1,1,1,1,1,1,1,1,1,1,1,1,1,1,1,1,1,1,1,1,1,1,1,1,1,1,1,1,1,1,
1,1,1,1,1,1,1,6),(-1.,-0.984615384615383,-0.969230769230768,-0.953846153846152,
-0.938461538461537,-0.923076923076922,-0.907692307692306,-0.892307692307691,
-0.876923076923076,-0.86153846153846,-0.846153846153845,-0.83076923076923,
-0.815384615384614,-0.799999999999999,-0.784615384615384,-0.769230769230768,
-0.753846153846153,-0.738461538461538,-0.723076923076922,-0.707692307692307,
-0.692307692307692,-0.676923076923076,-0.661538461538461,-0.646153846153846,
-0.63076923076923,-0.615384615384615,-0.6,-0.584615384615384,-0.569230769230769,
-0.553846153846154,-0.538461538461538,-0.523076923076923,-0.507692307692308,
-0.492307692307692,-0.476923076923077,-0.461538461538462,-0.446153846153846,
-0.430769230769231,-0.415384615384615,-0.4,-0.384615384615385,-0.369230769230769,
-0.353846153846154,-0.338461538461538,-0.323076923076923,-0.307692307692308,
-0.292307692307692,-0.276923076923077,-0.261538461538462,-0.246153846153846,
-0.230769230769231,-0.215384615384615,-0.2,-0.184615384615385,-0.169230769230769,
-0.153846153846154,-0.138461538461538,-0.123076923076923,-0.107692307692308,
-0.0923076923076923,-0.0769230769230769,-0.0615384615384615,-0.0461538461538462,
-0.0307692307692308,-0.0153846153846154,0.),.UNSPECIFIED.)
CURVE()
GEOMETRIC_REPRESENTATION_ITEM()
RATIONAL_B_SPLINE_CURVE((1.,1.,1.,1.,1.,1.,1.,1.,1.,1.,1.,1.,1.,1.,1.,1.,
1.,1.,1.,1.,1.,1.,1.,1.,1.,1.,1.,1.,1.,1.,1.,1.,1.,1.,1.,1.,1.,1.,1.,1.,
1.,1.,1.,1.,1.,1.,1.,1.,1.,1.,1.,1.,1.,1.,1.,1.,1.,1.,1.,1.,1.,1.,1.,1.,
1.,1.,1.,1.,1.,1.))
REPRESENTATION_ITEM('')
);
#187=(
BOUNDED_CURVE()
B_SPLINE_CURVE(5,(#33329,#33330,#33331,#33332,#33333,#33334,#33335,#33336,
#33337,#33338,#33339,#33340,#33341,#33342,#33343,#33344,#33345,#33346,#33347,
#33348,#33349,#33350,#33351,#33352,#33353,#33354,#33355,#33356,#33357,#33358,
#33359,#33360,#33361,#33362,#33363,#33364,#33365,#33366,#33367,#33368,#33369,
#33370,#33371,#33372,#33373,#33374,#33375,#33376,#33377,#33378,#33379,#33380,
#33381,#33382,#33383,#33384,#33385,#33386,#33387,#33388,#33389,#33390,#33391,
#33392,#33393,#33394,#33395,#33396,#33397,#33398),.UNSPECIFIED.,.F.,.F.)
B_SPLINE_CURVE_WITH_KNOTS((6,1,1,1,1,1,1,1,1,1,1,1,1,1,1,1,1,1,1,1,1,1,
1,1,1,1,1,1,1,1,1,1,1,1,1,1,1,1,1,1,1,1,1,1,1,1,1,1,1,1,1,1,1,1,1,1,1,1,
1,1,1,1,1,1,1,6),(-1.,-0.984615384615383,-0.969230769230768,-0.953846153846152,
-0.938461538461537,-0.923076923076922,-0.907692307692306,-0.892307692307691,
-0.876923076923076,-0.86153846153846,-0.846153846153845,-0.83076923076923,
-0.815384615384614,-0.799999999999999,-0.784615384615384,-0.769230769230768,
-0.753846153846153,-0.738461538461538,-0.723076923076922,-0.707692307692307,
-0.692307692307692,-0.676923076923076,-0.661538461538461,-0.646153846153846,
-0.63076923076923,-0.615384615384615,-0.6,-0.584615384615384,-0.569230769230769,
-0.553846153846154,-0.538461538461538,-0.523076923076923,-0.507692307692308,
-0.492307692307692,-0.476923076923077,-0.461538461538462,-0.446153846153846,
-0.430769230769231,-0.415384615384615,-0.4,-0.384615384615385,-0.369230769230769,
-0.353846153846154,-0.338461538461538,-0.323076923076923,-0.307692307692308,
-0.292307692307692,-0.276923076923077,-0.261538461538462,-0.246153846153846,
-0.230769230769231,-0.215384615384615,-0.2,-0.184615384615385,-0.169230769230769,
-0.153846153846154,-0.138461538461538,-0.123076923076923,-0.107692307692308,
-0.0923076923076923,-0.0769230769230769,-0.0615384615384615,-0.0461538461538462,
-0.0307692307692308,-0.0153846153846154,0.),.UNSPECIFIED.)
CURVE()
GEOMETRIC_REPRESENTATION_ITEM()
RATIONAL_B_SPLINE_CURVE((1.,1.,1.,1.,1.,1.,1.,1.,1.,1.,1.,1.,1.,1.,1.,1.,
1.,1.,1.,1.,1.,1.,1.,1.,1.,1.,1.,1.,1.,1.,1.,1.,1.,1.,1.,1.,1.,1.,1.,1.,
1.,1.,1.,1.,1.,1.,1.,1.,1.,1.,1.,1.,1.,1.,1.,1.,1.,1.,1.,1.,1.,1.,1.,1.,
1.,1.,1.,1.,1.,1.))
REPRESENTATION_ITEM('')
);
#188=(
BOUNDED_CURVE()
B_SPLINE_CURVE(5,(#33545,#33546,#33547,#33548,#33549,#33550,#33551,#33552,
#33553,#33554,#33555,#33556,#33557,#33558,#33559,#33560,#33561,#33562,#33563,
#33564,#33565,#33566,#33567,#33568,#33569,#33570,#33571,#33572,#33573,#33574,
#33575,#33576,#33577,#33578,#33579,#33580,#33581,#33582,#33583,#33584,#33585,
#33586,#33587,#33588,#33589,#33590,#33591,#33592,#33593,#33594,#33595,#33596,
#33597,#33598,#33599,#33600,#33601,#33602,#33603,#33604,#33605,#33606,#33607,
#33608,#33609,#33610,#33611,#33612,#33613,#33614),.UNSPECIFIED.,.F.,.F.)
B_SPLINE_CURVE_WITH_KNOTS((6,1,1,1,1,1,1,1,1,1,1,1,1,1,1,1,1,1,1,1,1,1,
1,1,1,1,1,1,1,1,1,1,1,1,1,1,1,1,1,1,1,1,1,1,1,1,1,1,1,1,1,1,1,1,1,1,1,1,
1,1,1,1,1,1,1,6),(-1.,-0.984615384615383,-0.969230769230768,-0.953846153846152,
-0.938461538461537,-0.923076923076922,-0.907692307692306,-0.892307692307691,
-0.876923076923076,-0.86153846153846,-0.846153846153845,-0.83076923076923,
-0.815384615384614,-0.799999999999999,-0.784615384615384,-0.769230769230768,
-0.753846153846153,-0.738461538461538,-0.723076923076922,-0.707692307692307,
-0.692307692307692,-0.676923076923076,-0.661538461538461,-0.646153846153846,
-0.63076923076923,-0.615384615384615,-0.6,-0.584615384615384,-0.569230769230769,
-0.553846153846154,-0.538461538461538,-0.523076923076923,-0.507692307692308,
-0.492307692307692,-0.476923076923077,-0.461538461538462,-0.446153846153846,
-0.430769230769231,-0.415384615384615,-0.4,-0.384615384615385,-0.369230769230769,
-0.353846153846154,-0.338461538461538,-0.323076923076923,-0.307692307692308,
-0.292307692307692,-0.276923076923077,-0.261538461538462,-0.246153846153846,
-0.230769230769231,-0.215384615384615,-0.2,-0.184615384615385,-0.169230769230769,
-0.153846153846154,-0.138461538461538,-0.123076923076923,-0.107692307692308,
-0.0923076923076923,-0.0769230769230769,-0.0615384615384615,-0.0461538461538462,
-0.0307692307692308,-0.0153846153846154,0.),.UNSPECIFIED.)
CURVE()
GEOMETRIC_REPRESENTATION_ITEM()
RATIONAL_B_SPLINE_CURVE((1.,1.,1.,1.,1.,1.,1.,1.,1.,1.,1.,1.,1.,1.,1.,1.,
1.,1.,1.,1.,1.,1.,1.,1.,1.,1.,1.,1.,1.,1.,1.,1.,1.,1.,1.,1.,1.,1.,1.,1.,
1.,1.,1.,1.,1.,1.,1.,1.,1.,1.,1.,1.,1.,1.,1.,1.,1.,1.,1.,1.,1.,1.,1.,1.,
1.,1.,1.,1.,1.,1.))
REPRESENTATION_ITEM('')
);
#189=(
BOUNDED_CURVE()
B_SPLINE_CURVE(5,(#33761,#33762,#33763,#33764,#33765,#33766,#33767,#33768,
#33769,#33770,#33771,#33772,#33773,#33774,#33775,#33776,#33777,#33778,#33779,
#33780,#33781,#33782,#33783,#33784,#33785,#33786,#33787,#33788,#33789,#33790,
#33791,#33792,#33793,#33794,#33795,#33796,#33797,#33798,#33799,#33800,#33801,
#33802,#33803,#33804,#33805,#33806,#33807,#33808,#33809,#33810,#33811,#33812,
#33813,#33814,#33815,#33816,#33817,#33818,#33819,#33820,#33821,#33822,#33823,
#33824,#33825,#33826,#33827,#33828,#33829,#33830),.UNSPECIFIED.,.F.,.F.)
B_SPLINE_CURVE_WITH_KNOTS((6,1,1,1,1,1,1,1,1,1,1,1,1,1,1,1,1,1,1,1,1,1,
1,1,1,1,1,1,1,1,1,1,1,1,1,1,1,1,1,1,1,1,1,1,1,1,1,1,1,1,1,1,1,1,1,1,1,1,
1,1,1,1,1,1,1,6),(-1.,-0.984615384615383,-0.969230769230768,-0.953846153846152,
-0.938461538461537,-0.923076923076922,-0.907692307692306,-0.892307692307691,
-0.876923076923076,-0.86153846153846,-0.846153846153845,-0.83076923076923,
-0.815384615384614,-0.799999999999999,-0.784615384615384,-0.769230769230768,
-0.753846153846153,-0.738461538461538,-0.723076923076922,-0.707692307692307,
-0.692307692307692,-0.676923076923076,-0.661538461538461,-0.646153846153846,
-0.63076923076923,-0.615384615384615,-0.6,-0.584615384615384,-0.569230769230769,
-0.553846153846154,-0.538461538461538,-0.523076923076923,-0.507692307692308,
-0.492307692307692,-0.476923076923077,-0.461538461538462,-0.446153846153846,
-0.430769230769231,-0.415384615384615,-0.4,-0.384615384615385,-0.369230769230769,
-0.353846153846154,-0.338461538461538,-0.323076923076923,-0.307692307692308,
-0.292307692307692,-0.276923076923077,-0.261538461538462,-0.246153846153846,
-0.230769230769231,-0.215384615384615,-0.2,-0.184615384615385,-0.169230769230769,
-0.153846153846154,-0.138461538461538,-0.123076923076923,-0.107692307692308,
-0.0923076923076923,-0.0769230769230769,-0.0615384615384615,-0.0461538461538462,
-0.0307692307692308,-0.0153846153846154,0.),.UNSPECIFIED.)
CURVE()
GEOMETRIC_REPRESENTATION_ITEM()
RATIONAL_B_SPLINE_CURVE((1.,1.,1.,1.,1.,1.,1.,1.,1.,1.,1.,1.,1.,1.,1.,1.,
1.,1.,1.,1.,1.,1.,1.,1.,1.,1.,1.,1.,1.,1.,1.,1.,1.,1.,1.,1.,1.,1.,1.,1.,
1.,1.,1.,1.,1.,1.,1.,1.,1.,1.,1.,1.,1.,1.,1.,1.,1.,1.,1.,1.,1.,1.,1.,1.,
1.,1.,1.,1.,1.,1.))
REPRESENTATION_ITEM('')
);
#190=(
BOUNDED_CURVE()
B_SPLINE_CURVE(5,(#33977,#33978,#33979,#33980,#33981,#33982,#33983,#33984,
#33985,#33986,#33987,#33988,#33989,#33990,#33991,#33992,#33993,#33994,#33995,
#33996,#33997,#33998,#33999,#34000,#34001,#34002,#34003,#34004,#34005,#34006,
#34007,#34008,#34009,#34010,#34011,#34012,#34013,#34014,#34015,#34016,#34017,
#34018,#34019,#34020,#34021,#34022,#34023,#34024,#34025,#34026,#34027,#34028,
#34029,#34030,#34031,#34032,#34033,#34034,#34035,#34036,#34037,#34038,#34039,
#34040,#34041,#34042,#34043,#34044,#34045,#34046),.UNSPECIFIED.,.F.,.F.)
B_SPLINE_CURVE_WITH_KNOTS((6,1,1,1,1,1,1,1,1,1,1,1,1,1,1,1,1,1,1,1,1,1,
1,1,1,1,1,1,1,1,1,1,1,1,1,1,1,1,1,1,1,1,1,1,1,1,1,1,1,1,1,1,1,1,1,1,1,1,
1,1,1,1,1,1,1,6),(-1.,-0.984615384615383,-0.969230769230768,-0.953846153846152,
-0.938461538461537,-0.923076923076922,-0.907692307692306,-0.892307692307691,
-0.876923076923076,-0.86153846153846,-0.846153846153845,-0.83076923076923,
-0.815384615384614,-0.799999999999999,-0.784615384615384,-0.769230769230768,
-0.753846153846153,-0.738461538461538,-0.723076923076922,-0.707692307692307,
-0.692307692307692,-0.676923076923076,-0.661538461538461,-0.646153846153846,
-0.63076923076923,-0.615384615384615,-0.6,-0.584615384615384,-0.569230769230769,
-0.553846153846154,-0.538461538461538,-0.523076923076923,-0.507692307692308,
-0.492307692307692,-0.476923076923077,-0.461538461538462,-0.446153846153846,
-0.430769230769231,-0.415384615384615,-0.4,-0.384615384615385,-0.369230769230769,
-0.353846153846154,-0.338461538461538,-0.323076923076923,-0.307692307692308,
-0.292307692307692,-0.276923076923077,-0.261538461538462,-0.246153846153846,
-0.230769230769231,-0.215384615384615,-0.2,-0.184615384615385,-0.169230769230769,
-0.153846153846154,-0.138461538461538,-0.123076923076923,-0.107692307692308,
-0.0923076923076923,-0.0769230769230769,-0.0615384615384615,-0.0461538461538462,
-0.0307692307692308,-0.0153846153846154,0.),.UNSPECIFIED.)
CURVE()
GEOMETRIC_REPRESENTATION_ITEM()
RATIONAL_B_SPLINE_CURVE((1.,1.,1.,1.,1.,1.,1.,1.,1.,1.,1.,1.,1.,1.,1.,1.,
1.,1.,1.,1.,1.,1.,1.,1.,1.,1.,1.,1.,1.,1.,1.,1.,1.,1.,1.,1.,1.,1.,1.,1.,
1.,1.,1.,1.,1.,1.,1.,1.,1.,1.,1.,1.,1.,1.,1.,1.,1.,1.,1.,1.,1.,1.,1.,1.,
1.,1.,1.,1.,1.,1.))
REPRESENTATION_ITEM('')
);
#191=(
BOUNDED_CURVE()
B_SPLINE_CURVE(5,(#34193,#34194,#34195,#34196,#34197,#34198,#34199,#34200,
#34201,#34202,#34203,#34204,#34205,#34206,#34207,#34208,#34209,#34210,#34211,
#34212,#34213,#34214,#34215,#34216,#34217,#34218,#34219,#34220,#34221,#34222,
#34223,#34224,#34225,#34226,#34227,#34228,#34229,#34230,#34231,#34232,#34233,
#34234,#34235,#34236,#34237,#34238,#34239,#34240,#34241,#34242,#34243,#34244,
#34245,#34246,#34247,#34248,#34249,#34250,#34251,#34252,#34253,#34254,#34255,
#34256,#34257,#34258,#34259,#34260,#34261,#34262),.UNSPECIFIED.,.F.,.F.)
B_SPLINE_CURVE_WITH_KNOTS((6,1,1,1,1,1,1,1,1,1,1,1,1,1,1,1,1,1,1,1,1,1,
1,1,1,1,1,1,1,1,1,1,1,1,1,1,1,1,1,1,1,1,1,1,1,1,1,1,1,1,1,1,1,1,1,1,1,1,
1,1,1,1,1,1,1,6),(-1.,-0.984615384615383,-0.969230769230768,-0.953846153846152,
-0.938461538461537,-0.923076923076922,-0.907692307692306,-0.892307692307691,
-0.876923076923076,-0.86153846153846,-0.846153846153845,-0.83076923076923,
-0.815384615384614,-0.799999999999999,-0.784615384615384,-0.769230769230768,
-0.753846153846153,-0.738461538461538,-0.723076923076922,-0.707692307692307,
-0.692307692307692,-0.676923076923076,-0.661538461538461,-0.646153846153846,
-0.63076923076923,-0.615384615384615,-0.6,-0.584615384615384,-0.569230769230769,
-0.553846153846154,-0.538461538461538,-0.523076923076923,-0.507692307692308,
-0.492307692307692,-0.476923076923077,-0.461538461538462,-0.446153846153846,
-0.430769230769231,-0.415384615384615,-0.4,-0.384615384615385,-0.369230769230769,
-0.353846153846154,-0.338461538461538,-0.323076923076923,-0.307692307692308,
-0.292307692307692,-0.276923076923077,-0.261538461538462,-0.246153846153846,
-0.230769230769231,-0.215384615384615,-0.2,-0.184615384615385,-0.169230769230769,
-0.153846153846154,-0.138461538461538,-0.123076923076923,-0.107692307692308,
-0.0923076923076923,-0.0769230769230769,-0.0615384615384615,-0.0461538461538462,
-0.0307692307692308,-0.0153846153846154,0.),.UNSPECIFIED.)
CURVE()
GEOMETRIC_REPRESENTATION_ITEM()
RATIONAL_B_SPLINE_CURVE((1.,1.,1.,1.,1.,1.,1.,1.,1.,1.,1.,1.,1.,1.,1.,1.,
1.,1.,1.,1.,1.,1.,1.,1.,1.,1.,1.,1.,1.,1.,1.,1.,1.,1.,1.,1.,1.,1.,1.,1.,
1.,1.,1.,1.,1.,1.,1.,1.,1.,1.,1.,1.,1.,1.,1.,1.,1.,1.,1.,1.,1.,1.,1.,1.,
1.,1.,1.,1.,1.,1.))
REPRESENTATION_ITEM('')
);
#192=(
BOUNDED_CURVE()
B_SPLINE_CURVE(5,(#34409,#34410,#34411,#34412,#34413,#34414,#34415,#34416,
#34417,#34418,#34419,#34420,#34421,#34422,#34423,#34424,#34425,#34426,#34427,
#34428,#34429,#34430,#34431,#34432,#34433,#34434,#34435,#34436,#34437,#34438,
#34439,#34440,#34441,#34442,#34443,#34444,#34445,#34446,#34447,#34448,#34449,
#34450,#34451,#34452,#34453,#34454,#34455,#34456,#34457,#34458,#34459,#34460,
#34461,#34462,#34463,#34464,#34465,#34466,#34467,#34468,#34469,#34470,#34471,
#34472,#34473,#34474,#34475,#34476,#34477,#34478),.UNSPECIFIED.,.F.,.F.)
B_SPLINE_CURVE_WITH_KNOTS((6,1,1,1,1,1,1,1,1,1,1,1,1,1,1,1,1,1,1,1,1,1,
1,1,1,1,1,1,1,1,1,1,1,1,1,1,1,1,1,1,1,1,1,1,1,1,1,1,1,1,1,1,1,1,1,1,1,1,
1,1,1,1,1,1,1,6),(-1.,-0.984615384615383,-0.969230769230768,-0.953846153846152,
-0.938461538461537,-0.923076923076922,-0.907692307692306,-0.892307692307691,
-0.876923076923076,-0.86153846153846,-0.846153846153845,-0.83076923076923,
-0.815384615384614,-0.799999999999999,-0.784615384615384,-0.769230769230768,
-0.753846153846153,-0.738461538461538,-0.723076923076922,-0.707692307692307,
-0.692307692307692,-0.676923076923076,-0.661538461538461,-0.646153846153846,
-0.63076923076923,-0.615384615384615,-0.6,-0.584615384615384,-0.569230769230769,
-0.553846153846154,-0.538461538461538,-0.523076923076923,-0.507692307692308,
-0.492307692307692,-0.476923076923077,-0.461538461538462,-0.446153846153846,
-0.430769230769231,-0.415384615384615,-0.4,-0.384615384615385,-0.369230769230769,
-0.353846153846154,-0.338461538461538,-0.323076923076923,-0.307692307692308,
-0.292307692307692,-0.276923076923077,-0.261538461538462,-0.246153846153846,
-0.230769230769231,-0.215384615384615,-0.2,-0.184615384615385,-0.169230769230769,
-0.153846153846154,-0.138461538461538,-0.123076923076923,-0.107692307692308,
-0.0923076923076923,-0.0769230769230769,-0.0615384615384615,-0.0461538461538462,
-0.0307692307692308,-0.0153846153846154,0.),.UNSPECIFIED.)
CURVE()
GEOMETRIC_REPRESENTATION_ITEM()
RATIONAL_B_SPLINE_CURVE((1.,1.,1.,1.,1.,1.,1.,1.,1.,1.,1.,1.,1.,1.,1.,1.,
1.,1.,1.,1.,1.,1.,1.,1.,1.,1.,1.,1.,1.,1.,1.,1.,1.,1.,1.,1.,1.,1.,1.,1.,
1.,1.,1.,1.,1.,1.,1.,1.,1.,1.,1.,1.,1.,1.,1.,1.,1.,1.,1.,1.,1.,1.,1.,1.,
1.,1.,1.,1.,1.,1.))
REPRESENTATION_ITEM('')
);
#193=(
BOUNDED_CURVE()
B_SPLINE_CURVE(5,(#34625,#34626,#34627,#34628,#34629,#34630,#34631,#34632,
#34633,#34634,#34635,#34636,#34637,#34638,#34639,#34640,#34641,#34642,#34643,
#34644,#34645,#34646,#34647,#34648,#34649,#34650,#34651,#34652,#34653,#34654,
#34655,#34656,#34657,#34658,#34659,#34660,#34661,#34662,#34663,#34664,#34665,
#34666,#34667,#34668,#34669,#34670,#34671,#34672,#34673,#34674,#34675,#34676,
#34677,#34678,#34679,#34680,#34681,#34682,#34683,#34684,#34685,#34686,#34687,
#34688,#34689,#34690,#34691,#34692,#34693,#34694),.UNSPECIFIED.,.F.,.F.)
B_SPLINE_CURVE_WITH_KNOTS((6,1,1,1,1,1,1,1,1,1,1,1,1,1,1,1,1,1,1,1,1,1,
1,1,1,1,1,1,1,1,1,1,1,1,1,1,1,1,1,1,1,1,1,1,1,1,1,1,1,1,1,1,1,1,1,1,1,1,
1,1,1,1,1,1,1,6),(-1.,-0.984615384615383,-0.969230769230768,-0.953846153846152,
-0.938461538461537,-0.923076923076922,-0.907692307692306,-0.892307692307691,
-0.876923076923076,-0.86153846153846,-0.846153846153845,-0.83076923076923,
-0.815384615384614,-0.799999999999999,-0.784615384615384,-0.769230769230768,
-0.753846153846153,-0.738461538461538,-0.723076923076922,-0.707692307692307,
-0.692307692307692,-0.676923076923076,-0.661538461538461,-0.646153846153846,
-0.63076923076923,-0.615384615384615,-0.6,-0.584615384615384,-0.569230769230769,
-0.553846153846154,-0.538461538461538,-0.523076923076923,-0.507692307692308,
-0.492307692307692,-0.476923076923077,-0.461538461538462,-0.446153846153846,
-0.430769230769231,-0.415384615384615,-0.4,-0.384615384615385,-0.369230769230769,
-0.353846153846154,-0.338461538461538,-0.323076923076923,-0.307692307692308,
-0.292307692307692,-0.276923076923077,-0.261538461538462,-0.246153846153846,
-0.230769230769231,-0.215384615384615,-0.2,-0.184615384615385,-0.169230769230769,
-0.153846153846154,-0.138461538461538,-0.123076923076923,-0.107692307692308,
-0.0923076923076923,-0.0769230769230769,-0.0615384615384615,-0.0461538461538462,
-0.0307692307692308,-0.0153846153846154,0.),.UNSPECIFIED.)
CURVE()
GEOMETRIC_REPRESENTATION_ITEM()
RATIONAL_B_SPLINE_CURVE((1.,1.,1.,1.,1.,1.,1.,1.,1.,1.,1.,1.,1.,1.,1.,1.,
1.,1.,1.,1.,1.,1.,1.,1.,1.,1.,1.,1.,1.,1.,1.,1.,1.,1.,1.,1.,1.,1.,1.,1.,
1.,1.,1.,1.,1.,1.,1.,1.,1.,1.,1.,1.,1.,1.,1.,1.,1.,1.,1.,1.,1.,1.,1.,1.,
1.,1.,1.,1.,1.,1.))
REPRESENTATION_ITEM('')
);
#194=(
BOUNDED_CURVE()
B_SPLINE_CURVE(5,(#34841,#34842,#34843,#34844,#34845,#34846,#34847,#34848,
#34849,#34850,#34851,#34852,#34853,#34854,#34855,#34856,#34857,#34858,#34859,
#34860,#34861,#34862,#34863,#34864,#34865,#34866,#34867,#34868,#34869,#34870,
#34871,#34872,#34873,#34874,#34875,#34876,#34877,#34878,#34879,#34880,#34881,
#34882,#34883,#34884,#34885,#34886,#34887,#34888,#34889,#34890,#34891,#34892,
#34893,#34894,#34895,#34896,#34897,#34898,#34899,#34900,#34901,#34902,#34903,
#34904,#34905,#34906,#34907,#34908,#34909,#34910),.UNSPECIFIED.,.F.,.F.)
B_SPLINE_CURVE_WITH_KNOTS((6,1,1,1,1,1,1,1,1,1,1,1,1,1,1,1,1,1,1,1,1,1,
1,1,1,1,1,1,1,1,1,1,1,1,1,1,1,1,1,1,1,1,1,1,1,1,1,1,1,1,1,1,1,1,1,1,1,1,
1,1,1,1,1,1,1,6),(-1.,-0.984615384615383,-0.969230769230768,-0.953846153846152,
-0.938461538461537,-0.923076923076922,-0.907692307692306,-0.892307692307691,
-0.876923076923076,-0.86153846153846,-0.846153846153845,-0.83076923076923,
-0.815384615384614,-0.799999999999999,-0.784615384615384,-0.769230769230768,
-0.753846153846153,-0.738461538461538,-0.723076923076922,-0.707692307692307,
-0.692307692307692,-0.676923076923076,-0.661538461538461,-0.646153846153846,
-0.63076923076923,-0.615384615384615,-0.6,-0.584615384615384,-0.569230769230769,
-0.553846153846154,-0.538461538461538,-0.523076923076923,-0.507692307692308,
-0.492307692307692,-0.476923076923077,-0.461538461538462,-0.446153846153846,
-0.430769230769231,-0.415384615384615,-0.4,-0.384615384615385,-0.369230769230769,
-0.353846153846154,-0.338461538461538,-0.323076923076923,-0.307692307692308,
-0.292307692307692,-0.276923076923077,-0.261538461538462,-0.246153846153846,
-0.230769230769231,-0.215384615384615,-0.2,-0.184615384615385,-0.169230769230769,
-0.153846153846154,-0.138461538461538,-0.123076923076923,-0.107692307692308,
-0.0923076923076923,-0.0769230769230769,-0.0615384615384615,-0.0461538461538462,
-0.0307692307692308,-0.0153846153846154,0.),.UNSPECIFIED.)
CURVE()
GEOMETRIC_REPRESENTATION_ITEM()
RATIONAL_B_SPLINE_CURVE((1.,1.,1.,1.,1.,1.,1.,1.,1.,1.,1.,1.,1.,1.,1.,1.,
1.,1.,1.,1.,1.,1.,1.,1.,1.,1.,1.,1.,1.,1.,1.,1.,1.,1.,1.,1.,1.,1.,1.,1.,
1.,1.,1.,1.,1.,1.,1.,1.,1.,1.,1.,1.,1.,1.,1.,1.,1.,1.,1.,1.,1.,1.,1.,1.,
1.,1.,1.,1.,1.,1.))
REPRESENTATION_ITEM('')
);
#195=(
BOUNDED_CURVE()
B_SPLINE_CURVE(5,(#35057,#35058,#35059,#35060,#35061,#35062,#35063,#35064,
#35065,#35066,#35067,#35068,#35069,#35070,#35071,#35072,#35073,#35074,#35075,
#35076,#35077,#35078,#35079,#35080,#35081,#35082,#35083,#35084,#35085,#35086,
#35087,#35088,#35089,#35090,#35091,#35092,#35093,#35094,#35095,#35096,#35097,
#35098,#35099,#35100,#35101,#35102,#35103,#35104,#35105,#35106,#35107,#35108,
#35109,#35110,#35111,#35112,#35113,#35114,#35115,#35116,#35117,#35118,#35119,
#35120,#35121,#35122,#35123,#35124,#35125,#35126),.UNSPECIFIED.,.F.,.F.)
B_SPLINE_CURVE_WITH_KNOTS((6,1,1,1,1,1,1,1,1,1,1,1,1,1,1,1,1,1,1,1,1,1,
1,1,1,1,1,1,1,1,1,1,1,1,1,1,1,1,1,1,1,1,1,1,1,1,1,1,1,1,1,1,1,1,1,1,1,1,
1,1,1,1,1,1,1,6),(-1.,-0.984615384615383,-0.969230769230768,-0.953846153846152,
-0.938461538461537,-0.923076923076922,-0.907692307692306,-0.892307692307691,
-0.876923076923076,-0.86153846153846,-0.846153846153845,-0.83076923076923,
-0.815384615384614,-0.799999999999999,-0.784615384615384,-0.769230769230768,
-0.753846153846153,-0.738461538461538,-0.723076923076922,-0.707692307692307,
-0.692307692307692,-0.676923076923076,-0.661538461538461,-0.646153846153846,
-0.63076923076923,-0.615384615384615,-0.6,-0.584615384615384,-0.569230769230769,
-0.553846153846154,-0.538461538461538,-0.523076923076923,-0.507692307692308,
-0.492307692307692,-0.476923076923077,-0.461538461538462,-0.446153846153846,
-0.430769230769231,-0.415384615384615,-0.4,-0.384615384615385,-0.369230769230769,
-0.353846153846154,-0.338461538461538,-0.323076923076923,-0.307692307692308,
-0.292307692307692,-0.276923076923077,-0.261538461538462,-0.246153846153846,
-0.230769230769231,-0.215384615384615,-0.2,-0.184615384615385,-0.169230769230769,
-0.153846153846154,-0.138461538461538,-0.123076923076923,-0.107692307692308,
-0.0923076923076923,-0.0769230769230769,-0.0615384615384615,-0.0461538461538462,
-0.0307692307692308,-0.0153846153846154,0.),.UNSPECIFIED.)
CURVE()
GEOMETRIC_REPRESENTATION_ITEM()
RATIONAL_B_SPLINE_CURVE((1.,1.,1.,1.,1.,1.,1.,1.,1.,1.,1.,1.,1.,1.,1.,1.,
1.,1.,1.,1.,1.,1.,1.,1.,1.,1.,1.,1.,1.,1.,1.,1.,1.,1.,1.,1.,1.,1.,1.,1.,
1.,1.,1.,1.,1.,1.,1.,1.,1.,1.,1.,1.,1.,1.,1.,1.,1.,1.,1.,1.,1.,1.,1.,1.,
1.,1.,1.,1.,1.,1.))
REPRESENTATION_ITEM('')
);
#196=(
BOUNDED_CURVE()
B_SPLINE_CURVE(5,(#35273,#35274,#35275,#35276,#35277,#35278,#35279,#35280,
#35281,#35282,#35283,#35284,#35285,#35286,#35287,#35288,#35289,#35290,#35291,
#35292,#35293,#35294,#35295,#35296,#35297,#35298,#35299,#35300,#35301,#35302,
#35303,#35304,#35305,#35306,#35307,#35308,#35309,#35310,#35311,#35312,#35313,
#35314,#35315,#35316,#35317,#35318,#35319,#35320,#35321,#35322,#35323,#35324,
#35325,#35326,#35327,#35328,#35329,#35330,#35331,#35332,#35333,#35334,#35335,
#35336,#35337,#35338,#35339,#35340,#35341,#35342),.UNSPECIFIED.,.F.,.F.)
B_SPLINE_CURVE_WITH_KNOTS((6,1,1,1,1,1,1,1,1,1,1,1,1,1,1,1,1,1,1,1,1,1,
1,1,1,1,1,1,1,1,1,1,1,1,1,1,1,1,1,1,1,1,1,1,1,1,1,1,1,1,1,1,1,1,1,1,1,1,
1,1,1,1,1,1,1,6),(-1.,-0.984615384615383,-0.969230769230768,-0.953846153846152,
-0.938461538461537,-0.923076923076922,-0.907692307692306,-0.892307692307691,
-0.876923076923076,-0.86153846153846,-0.846153846153845,-0.83076923076923,
-0.815384615384614,-0.799999999999999,-0.784615384615384,-0.769230769230768,
-0.753846153846153,-0.738461538461538,-0.723076923076922,-0.707692307692307,
-0.692307692307692,-0.676923076923076,-0.661538461538461,-0.646153846153846,
-0.63076923076923,-0.615384615384615,-0.6,-0.584615384615384,-0.569230769230769,
-0.553846153846154,-0.538461538461538,-0.523076923076923,-0.507692307692308,
-0.492307692307692,-0.476923076923077,-0.461538461538462,-0.446153846153846,
-0.430769230769231,-0.415384615384615,-0.4,-0.384615384615385,-0.369230769230769,
-0.353846153846154,-0.338461538461538,-0.323076923076923,-0.307692307692308,
-0.292307692307692,-0.276923076923077,-0.261538461538462,-0.246153846153846,
-0.230769230769231,-0.215384615384615,-0.2,-0.184615384615385,-0.169230769230769,
-0.153846153846154,-0.138461538461538,-0.123076923076923,-0.107692307692308,
-0.0923076923076923,-0.0769230769230769,-0.0615384615384615,-0.0461538461538462,
-0.0307692307692308,-0.0153846153846154,0.),.UNSPECIFIED.)
CURVE()
GEOMETRIC_REPRESENTATION_ITEM()
RATIONAL_B_SPLINE_CURVE((1.,1.,1.,1.,1.,1.,1.,1.,1.,1.,1.,1.,1.,1.,1.,1.,
1.,1.,1.,1.,1.,1.,1.,1.,1.,1.,1.,1.,1.,1.,1.,1.,1.,1.,1.,1.,1.,1.,1.,1.,
1.,1.,1.,1.,1.,1.,1.,1.,1.,1.,1.,1.,1.,1.,1.,1.,1.,1.,1.,1.,1.,1.,1.,1.,
1.,1.,1.,1.,1.,1.))
REPRESENTATION_ITEM('')
);
#197=(
BOUNDED_CURVE()
B_SPLINE_CURVE(5,(#35489,#35490,#35491,#35492,#35493,#35494,#35495,#35496,
#35497,#35498,#35499,#35500,#35501,#35502,#35503,#35504,#35505,#35506,#35507,
#35508,#35509,#35510,#35511,#35512,#35513,#35514,#35515,#35516,#35517,#35518,
#35519,#35520,#35521,#35522,#35523,#35524,#35525,#35526,#35527,#35528,#35529,
#35530,#35531,#35532,#35533,#35534,#35535,#35536,#35537,#35538,#35539,#35540,
#35541,#35542,#35543,#35544,#35545,#35546,#35547,#35548,#35549,#35550,#35551,
#35552,#35553,#35554,#35555,#35556,#35557,#35558),.UNSPECIFIED.,.F.,.F.)
B_SPLINE_CURVE_WITH_KNOTS((6,1,1,1,1,1,1,1,1,1,1,1,1,1,1,1,1,1,1,1,1,1,
1,1,1,1,1,1,1,1,1,1,1,1,1,1,1,1,1,1,1,1,1,1,1,1,1,1,1,1,1,1,1,1,1,1,1,1,
1,1,1,1,1,1,1,6),(-1.,-0.984615384615383,-0.969230769230768,-0.953846153846152,
-0.938461538461537,-0.923076923076922,-0.907692307692306,-0.892307692307691,
-0.876923076923076,-0.86153846153846,-0.846153846153845,-0.83076923076923,
-0.815384615384614,-0.799999999999999,-0.784615384615384,-0.769230769230768,
-0.753846153846153,-0.738461538461538,-0.723076923076922,-0.707692307692307,
-0.692307692307692,-0.676923076923076,-0.661538461538461,-0.646153846153846,
-0.63076923076923,-0.615384615384615,-0.6,-0.584615384615384,-0.569230769230769,
-0.553846153846154,-0.538461538461538,-0.523076923076923,-0.507692307692308,
-0.492307692307692,-0.476923076923077,-0.461538461538462,-0.446153846153846,
-0.430769230769231,-0.415384615384615,-0.4,-0.384615384615385,-0.369230769230769,
-0.353846153846154,-0.338461538461538,-0.323076923076923,-0.307692307692308,
-0.292307692307692,-0.276923076923077,-0.261538461538462,-0.246153846153846,
-0.230769230769231,-0.215384615384615,-0.2,-0.184615384615385,-0.169230769230769,
-0.153846153846154,-0.138461538461538,-0.123076923076923,-0.107692307692308,
-0.0923076923076923,-0.0769230769230769,-0.0615384615384615,-0.0461538461538462,
-0.0307692307692308,-0.0153846153846154,0.),.UNSPECIFIED.)
CURVE()
GEOMETRIC_REPRESENTATION_ITEM()
RATIONAL_B_SPLINE_CURVE((1.,1.,1.,1.,1.,1.,1.,1.,1.,1.,1.,1.,1.,1.,1.,1.,
1.,1.,1.,1.,1.,1.,1.,1.,1.,1.,1.,1.,1.,1.,1.,1.,1.,1.,1.,1.,1.,1.,1.,1.,
1.,1.,1.,1.,1.,1.,1.,1.,1.,1.,1.,1.,1.,1.,1.,1.,1.,1.,1.,1.,1.,1.,1.,1.,
1.,1.,1.,1.,1.,1.))
REPRESENTATION_ITEM('')
);
#198=(
BOUNDED_CURVE()
B_SPLINE_CURVE(5,(#35705,#35706,#35707,#35708,#35709,#35710,#35711,#35712,
#35713,#35714,#35715,#35716,#35717,#35718,#35719,#35720,#35721,#35722,#35723,
#35724,#35725,#35726,#35727,#35728,#35729,#35730,#35731,#35732,#35733,#35734,
#35735,#35736,#35737,#35738,#35739,#35740,#35741,#35742,#35743,#35744,#35745,
#35746,#35747,#35748,#35749,#35750,#35751,#35752,#35753,#35754,#35755,#35756,
#35757,#35758,#35759,#35760,#35761,#35762,#35763,#35764,#35765,#35766,#35767,
#35768,#35769,#35770,#35771,#35772,#35773,#35774),.UNSPECIFIED.,.F.,.F.)
B_SPLINE_CURVE_WITH_KNOTS((6,1,1,1,1,1,1,1,1,1,1,1,1,1,1,1,1,1,1,1,1,1,
1,1,1,1,1,1,1,1,1,1,1,1,1,1,1,1,1,1,1,1,1,1,1,1,1,1,1,1,1,1,1,1,1,1,1,1,
1,1,1,1,1,1,1,6),(-1.,-0.984615384615383,-0.969230769230768,-0.953846153846152,
-0.938461538461537,-0.923076923076922,-0.907692307692306,-0.892307692307691,
-0.876923076923076,-0.86153846153846,-0.846153846153845,-0.83076923076923,
-0.815384615384614,-0.799999999999999,-0.784615384615384,-0.769230769230768,
-0.753846153846153,-0.738461538461538,-0.723076923076922,-0.707692307692307,
-0.692307692307692,-0.676923076923076,-0.661538461538461,-0.646153846153846,
-0.63076923076923,-0.615384615384615,-0.6,-0.584615384615384,-0.569230769230769,
-0.553846153846154,-0.538461538461538,-0.523076923076923,-0.507692307692308,
-0.492307692307692,-0.476923076923077,-0.461538461538462,-0.446153846153846,
-0.430769230769231,-0.415384615384615,-0.4,-0.384615384615385,-0.369230769230769,
-0.353846153846154,-0.338461538461538,-0.323076923076923,-0.307692307692308,
-0.292307692307692,-0.276923076923077,-0.261538461538462,-0.246153846153846,
-0.230769230769231,-0.215384615384615,-0.2,-0.184615384615385,-0.169230769230769,
-0.153846153846154,-0.138461538461538,-0.123076923076923,-0.107692307692308,
-0.0923076923076923,-0.0769230769230769,-0.0615384615384615,-0.0461538461538462,
-0.0307692307692308,-0.0153846153846154,0.),.UNSPECIFIED.)
CURVE()
GEOMETRIC_REPRESENTATION_ITEM()
RATIONAL_B_SPLINE_CURVE((1.,1.,1.,1.,1.,1.,1.,1.,1.,1.,1.,1.,1.,1.,1.,1.,
1.,1.,1.,1.,1.,1.,1.,1.,1.,1.,1.,1.,1.,1.,1.,1.,1.,1.,1.,1.,1.,1.,1.,1.,
1.,1.,1.,1.,1.,1.,1.,1.,1.,1.,1.,1.,1.,1.,1.,1.,1.,1.,1.,1.,1.,1.,1.,1.,
1.,1.,1.,1.,1.,1.))
REPRESENTATION_ITEM('')
);
#199=(
BOUNDED_CURVE()
B_SPLINE_CURVE(5,(#35921,#35922,#35923,#35924,#35925,#35926,#35927,#35928,
#35929,#35930,#35931,#35932,#35933,#35934,#35935,#35936,#35937,#35938,#35939,
#35940,#35941,#35942,#35943,#35944,#35945,#35946,#35947,#35948,#35949,#35950,
#35951,#35952,#35953,#35954,#35955,#35956,#35957,#35958,#35959,#35960,#35961,
#35962,#35963,#35964,#35965,#35966,#35967,#35968,#35969,#35970,#35971,#35972,
#35973,#35974,#35975,#35976,#35977,#35978,#35979,#35980,#35981,#35982,#35983,
#35984,#35985,#35986,#35987,#35988,#35989,#35990),.UNSPECIFIED.,.F.,.F.)
B_SPLINE_CURVE_WITH_KNOTS((6,1,1,1,1,1,1,1,1,1,1,1,1,1,1,1,1,1,1,1,1,1,
1,1,1,1,1,1,1,1,1,1,1,1,1,1,1,1,1,1,1,1,1,1,1,1,1,1,1,1,1,1,1,1,1,1,1,1,
1,1,1,1,1,1,1,6),(-1.,-0.984615384615383,-0.969230769230768,-0.953846153846152,
-0.938461538461537,-0.923076923076922,-0.907692307692306,-0.892307692307691,
-0.876923076923076,-0.86153846153846,-0.846153846153845,-0.83076923076923,
-0.815384615384614,-0.799999999999999,-0.784615384615384,-0.769230769230768,
-0.753846153846153,-0.738461538461538,-0.723076923076922,-0.707692307692307,
-0.692307692307692,-0.676923076923076,-0.661538461538461,-0.646153846153846,
-0.63076923076923,-0.615384615384615,-0.6,-0.584615384615384,-0.569230769230769,
-0.553846153846154,-0.538461538461538,-0.523076923076923,-0.507692307692308,
-0.492307692307692,-0.476923076923077,-0.461538461538462,-0.446153846153846,
-0.430769230769231,-0.415384615384615,-0.4,-0.384615384615385,-0.369230769230769,
-0.353846153846154,-0.338461538461538,-0.323076923076923,-0.307692307692308,
-0.292307692307692,-0.276923076923077,-0.261538461538462,-0.246153846153846,
-0.230769230769231,-0.215384615384615,-0.2,-0.184615384615385,-0.169230769230769,
-0.153846153846154,-0.138461538461538,-0.123076923076923,-0.107692307692308,
-0.0923076923076923,-0.0769230769230769,-0.0615384615384615,-0.0461538461538462,
-0.0307692307692308,-0.0153846153846154,0.),.UNSPECIFIED.)
CURVE()
GEOMETRIC_REPRESENTATION_ITEM()
RATIONAL_B_SPLINE_CURVE((1.,1.,1.,1.,1.,1.,1.,1.,1.,1.,1.,1.,1.,1.,1.,1.,
1.,1.,1.,1.,1.,1.,1.,1.,1.,1.,1.,1.,1.,1.,1.,1.,1.,1.,1.,1.,1.,1.,1.,1.,
1.,1.,1.,1.,1.,1.,1.,1.,1.,1.,1.,1.,1.,1.,1.,1.,1.,1.,1.,1.,1.,1.,1.,1.,
1.,1.,1.,1.,1.,1.))
REPRESENTATION_ITEM('')
);
#200=(
BOUNDED_CURVE()
B_SPLINE_CURVE(5,(#36137,#36138,#36139,#36140,#36141,#36142,#36143,#36144,
#36145,#36146,#36147,#36148,#36149,#36150,#36151,#36152,#36153,#36154,#36155,
#36156,#36157,#36158,#36159,#36160,#36161,#36162,#36163,#36164,#36165,#36166,
#36167,#36168,#36169,#36170,#36171,#36172,#36173,#36174,#36175,#36176,#36177,
#36178,#36179,#36180,#36181,#36182,#36183,#36184,#36185,#36186,#36187,#36188,
#36189,#36190,#36191,#36192,#36193,#36194,#36195,#36196,#36197,#36198,#36199,
#36200,#36201,#36202,#36203,#36204,#36205,#36206),.UNSPECIFIED.,.F.,.F.)
B_SPLINE_CURVE_WITH_KNOTS((6,1,1,1,1,1,1,1,1,1,1,1,1,1,1,1,1,1,1,1,1,1,
1,1,1,1,1,1,1,1,1,1,1,1,1,1,1,1,1,1,1,1,1,1,1,1,1,1,1,1,1,1,1,1,1,1,1,1,
1,1,1,1,1,1,1,6),(-1.,-0.984615384615383,-0.969230769230768,-0.953846153846152,
-0.938461538461537,-0.923076923076922,-0.907692307692306,-0.892307692307691,
-0.876923076923076,-0.86153846153846,-0.846153846153845,-0.83076923076923,
-0.815384615384614,-0.799999999999999,-0.784615384615384,-0.769230769230768,
-0.753846153846153,-0.738461538461538,-0.723076923076922,-0.707692307692307,
-0.692307692307692,-0.676923076923076,-0.661538461538461,-0.646153846153846,
-0.63076923076923,-0.615384615384615,-0.6,-0.584615384615384,-0.569230769230769,
-0.553846153846154,-0.538461538461538,-0.523076923076923,-0.507692307692308,
-0.492307692307692,-0.476923076923077,-0.461538461538462,-0.446153846153846,
-0.430769230769231,-0.415384615384615,-0.4,-0.384615384615385,-0.369230769230769,
-0.353846153846154,-0.338461538461538,-0.323076923076923,-0.307692307692308,
-0.292307692307692,-0.276923076923077,-0.261538461538462,-0.246153846153846,
-0.230769230769231,-0.215384615384615,-0.2,-0.184615384615385,-0.169230769230769,
-0.153846153846154,-0.138461538461538,-0.123076923076923,-0.107692307692308,
-0.0923076923076923,-0.0769230769230769,-0.0615384615384615,-0.0461538461538462,
-0.0307692307692308,-0.0153846153846154,0.),.UNSPECIFIED.)
CURVE()
GEOMETRIC_REPRESENTATION_ITEM()
RATIONAL_B_SPLINE_CURVE((1.,1.,1.,1.,1.,1.,1.,1.,1.,1.,1.,1.,1.,1.,1.,1.,
1.,1.,1.,1.,1.,1.,1.,1.,1.,1.,1.,1.,1.,1.,1.,1.,1.,1.,1.,1.,1.,1.,1.,1.,
1.,1.,1.,1.,1.,1.,1.,1.,1.,1.,1.,1.,1.,1.,1.,1.,1.,1.,1.,1.,1.,1.,1.,1.,
1.,1.,1.,1.,1.,1.))
REPRESENTATION_ITEM('')
);
#201=(
BOUNDED_CURVE()
B_SPLINE_CURVE(5,(#36353,#36354,#36355,#36356,#36357,#36358,#36359,#36360,
#36361,#36362,#36363,#36364,#36365,#36366,#36367,#36368,#36369,#36370,#36371,
#36372,#36373,#36374,#36375,#36376,#36377,#36378,#36379,#36380,#36381,#36382,
#36383,#36384,#36385,#36386,#36387,#36388,#36389,#36390,#36391,#36392,#36393,
#36394,#36395,#36396,#36397,#36398,#36399,#36400,#36401,#36402,#36403,#36404,
#36405,#36406,#36407,#36408,#36409,#36410,#36411,#36412,#36413,#36414,#36415,
#36416,#36417,#36418,#36419,#36420,#36421,#36422),.UNSPECIFIED.,.F.,.F.)
B_SPLINE_CURVE_WITH_KNOTS((6,1,1,1,1,1,1,1,1,1,1,1,1,1,1,1,1,1,1,1,1,1,
1,1,1,1,1,1,1,1,1,1,1,1,1,1,1,1,1,1,1,1,1,1,1,1,1,1,1,1,1,1,1,1,1,1,1,1,
1,1,1,1,1,1,1,6),(-1.,-0.984615384615383,-0.969230769230768,-0.953846153846152,
-0.938461538461537,-0.923076923076922,-0.907692307692306,-0.892307692307691,
-0.876923076923076,-0.86153846153846,-0.846153846153845,-0.83076923076923,
-0.815384615384614,-0.799999999999999,-0.784615384615384,-0.769230769230768,
-0.753846153846153,-0.738461538461538,-0.723076923076922,-0.707692307692307,
-0.692307692307692,-0.676923076923076,-0.661538461538461,-0.646153846153846,
-0.63076923076923,-0.615384615384615,-0.6,-0.584615384615384,-0.569230769230769,
-0.553846153846154,-0.538461538461538,-0.523076923076923,-0.507692307692308,
-0.492307692307692,-0.476923076923077,-0.461538461538462,-0.446153846153846,
-0.430769230769231,-0.415384615384615,-0.4,-0.384615384615385,-0.369230769230769,
-0.353846153846154,-0.338461538461538,-0.323076923076923,-0.307692307692308,
-0.292307692307692,-0.276923076923077,-0.261538461538462,-0.246153846153846,
-0.230769230769231,-0.215384615384615,-0.2,-0.184615384615385,-0.169230769230769,
-0.153846153846154,-0.138461538461538,-0.123076923076923,-0.107692307692308,
-0.0923076923076923,-0.0769230769230769,-0.0615384615384615,-0.0461538461538462,
-0.0307692307692308,-0.0153846153846154,0.),.UNSPECIFIED.)
CURVE()
GEOMETRIC_REPRESENTATION_ITEM()
RATIONAL_B_SPLINE_CURVE((1.,1.,1.,1.,1.,1.,1.,1.,1.,1.,1.,1.,1.,1.,1.,1.,
1.,1.,1.,1.,1.,1.,1.,1.,1.,1.,1.,1.,1.,1.,1.,1.,1.,1.,1.,1.,1.,1.,1.,1.,
1.,1.,1.,1.,1.,1.,1.,1.,1.,1.,1.,1.,1.,1.,1.,1.,1.,1.,1.,1.,1.,1.,1.,1.,
1.,1.,1.,1.,1.,1.))
REPRESENTATION_ITEM('')
);
#202=(
BOUNDED_CURVE()
B_SPLINE_CURVE(5,(#36569,#36570,#36571,#36572,#36573,#36574,#36575,#36576,
#36577,#36578,#36579,#36580,#36581,#36582,#36583,#36584,#36585,#36586,#36587,
#36588,#36589,#36590,#36591,#36592,#36593,#36594,#36595,#36596,#36597,#36598,
#36599,#36600,#36601,#36602,#36603,#36604,#36605,#36606,#36607,#36608,#36609,
#36610,#36611,#36612,#36613,#36614,#36615,#36616,#36617,#36618,#36619,#36620,
#36621,#36622,#36623,#36624,#36625,#36626,#36627,#36628,#36629,#36630,#36631,
#36632,#36633,#36634,#36635,#36636,#36637,#36638),.UNSPECIFIED.,.F.,.F.)
B_SPLINE_CURVE_WITH_KNOTS((6,1,1,1,1,1,1,1,1,1,1,1,1,1,1,1,1,1,1,1,1,1,
1,1,1,1,1,1,1,1,1,1,1,1,1,1,1,1,1,1,1,1,1,1,1,1,1,1,1,1,1,1,1,1,1,1,1,1,
1,1,1,1,1,1,1,6),(-1.,-0.984615384615383,-0.969230769230768,-0.953846153846152,
-0.938461538461537,-0.923076923076922,-0.907692307692306,-0.892307692307691,
-0.876923076923076,-0.86153846153846,-0.846153846153845,-0.83076923076923,
-0.815384615384614,-0.799999999999999,-0.784615384615384,-0.769230769230768,
-0.753846153846153,-0.738461538461538,-0.723076923076922,-0.707692307692307,
-0.692307692307692,-0.676923076923076,-0.661538461538461,-0.646153846153846,
-0.63076923076923,-0.615384615384615,-0.6,-0.584615384615384,-0.569230769230769,
-0.553846153846154,-0.538461538461538,-0.523076923076923,-0.507692307692308,
-0.492307692307692,-0.476923076923077,-0.461538461538462,-0.446153846153846,
-0.430769230769231,-0.415384615384615,-0.4,-0.384615384615385,-0.369230769230769,
-0.353846153846154,-0.338461538461538,-0.323076923076923,-0.307692307692308,
-0.292307692307692,-0.276923076923077,-0.261538461538462,-0.246153846153846,
-0.230769230769231,-0.215384615384615,-0.2,-0.184615384615385,-0.169230769230769,
-0.153846153846154,-0.138461538461538,-0.123076923076923,-0.107692307692308,
-0.0923076923076923,-0.0769230769230769,-0.0615384615384615,-0.0461538461538462,
-0.0307692307692308,-0.0153846153846154,0.),.UNSPECIFIED.)
CURVE()
GEOMETRIC_REPRESENTATION_ITEM()
RATIONAL_B_SPLINE_CURVE((1.,1.,1.,1.,1.,1.,1.,1.,1.,1.,1.,1.,1.,1.,1.,1.,
1.,1.,1.,1.,1.,1.,1.,1.,1.,1.,1.,1.,1.,1.,1.,1.,1.,1.,1.,1.,1.,1.,1.,1.,
1.,1.,1.,1.,1.,1.,1.,1.,1.,1.,1.,1.,1.,1.,1.,1.,1.,1.,1.,1.,1.,1.,1.,1.,
1.,1.,1.,1.,1.,1.))
REPRESENTATION_ITEM('')
);
#203=(
BOUNDED_CURVE()
B_SPLINE_CURVE(5,(#36785,#36786,#36787,#36788,#36789,#36790,#36791,#36792,
#36793,#36794,#36795,#36796,#36797,#36798,#36799,#36800,#36801,#36802,#36803,
#36804,#36805,#36806,#36807,#36808,#36809,#36810,#36811,#36812,#36813,#36814,
#36815,#36816,#36817,#36818,#36819,#36820,#36821,#36822,#36823,#36824,#36825,
#36826,#36827,#36828,#36829,#36830,#36831,#36832,#36833,#36834,#36835,#36836,
#36837,#36838,#36839,#36840,#36841,#36842,#36843,#36844,#36845,#36846,#36847,
#36848,#36849,#36850,#36851,#36852,#36853,#36854),.UNSPECIFIED.,.F.,.F.)
B_SPLINE_CURVE_WITH_KNOTS((6,1,1,1,1,1,1,1,1,1,1,1,1,1,1,1,1,1,1,1,1,1,
1,1,1,1,1,1,1,1,1,1,1,1,1,1,1,1,1,1,1,1,1,1,1,1,1,1,1,1,1,1,1,1,1,1,1,1,
1,1,1,1,1,1,1,6),(-1.,-0.984615384615383,-0.969230769230768,-0.953846153846152,
-0.938461538461537,-0.923076923076922,-0.907692307692306,-0.892307692307691,
-0.876923076923076,-0.86153846153846,-0.846153846153845,-0.83076923076923,
-0.815384615384614,-0.799999999999999,-0.784615384615384,-0.769230769230768,
-0.753846153846153,-0.738461538461538,-0.723076923076922,-0.707692307692307,
-0.692307692307692,-0.676923076923076,-0.661538461538461,-0.646153846153846,
-0.63076923076923,-0.615384615384615,-0.6,-0.584615384615384,-0.569230769230769,
-0.553846153846154,-0.538461538461538,-0.523076923076923,-0.507692307692308,
-0.492307692307692,-0.476923076923077,-0.461538461538462,-0.446153846153846,
-0.430769230769231,-0.415384615384615,-0.4,-0.384615384615385,-0.369230769230769,
-0.353846153846154,-0.338461538461538,-0.323076923076923,-0.307692307692308,
-0.292307692307692,-0.276923076923077,-0.261538461538462,-0.246153846153846,
-0.230769230769231,-0.215384615384615,-0.2,-0.184615384615385,-0.169230769230769,
-0.153846153846154,-0.138461538461538,-0.123076923076923,-0.107692307692308,
-0.0923076923076923,-0.0769230769230769,-0.0615384615384615,-0.0461538461538462,
-0.0307692307692308,-0.0153846153846154,0.),.UNSPECIFIED.)
CURVE()
GEOMETRIC_REPRESENTATION_ITEM()
RATIONAL_B_SPLINE_CURVE((1.,1.,1.,1.,1.,1.,1.,1.,1.,1.,1.,1.,1.,1.,1.,1.,
1.,1.,1.,1.,1.,1.,1.,1.,1.,1.,1.,1.,1.,1.,1.,1.,1.,1.,1.,1.,1.,1.,1.,1.,
1.,1.,1.,1.,1.,1.,1.,1.,1.,1.,1.,1.,1.,1.,1.,1.,1.,1.,1.,1.,1.,1.,1.,1.,
1.,1.,1.,1.,1.,1.))
REPRESENTATION_ITEM('')
);
#204=(
BOUNDED_CURVE()
B_SPLINE_CURVE(5,(#37001,#37002,#37003,#37004,#37005,#37006,#37007,#37008,
#37009,#37010,#37011,#37012,#37013,#37014,#37015,#37016,#37017,#37018,#37019,
#37020,#37021,#37022,#37023,#37024,#37025,#37026,#37027,#37028,#37029,#37030,
#37031,#37032,#37033,#37034,#37035,#37036,#37037,#37038,#37039,#37040,#37041,
#37042,#37043,#37044,#37045,#37046,#37047,#37048,#37049,#37050,#37051,#37052,
#37053,#37054,#37055,#37056,#37057,#37058,#37059,#37060,#37061,#37062,#37063,
#37064,#37065,#37066,#37067,#37068,#37069,#37070),.UNSPECIFIED.,.F.,.F.)
B_SPLINE_CURVE_WITH_KNOTS((6,1,1,1,1,1,1,1,1,1,1,1,1,1,1,1,1,1,1,1,1,1,
1,1,1,1,1,1,1,1,1,1,1,1,1,1,1,1,1,1,1,1,1,1,1,1,1,1,1,1,1,1,1,1,1,1,1,1,
1,1,1,1,1,1,1,6),(-1.,-0.984615384615383,-0.969230769230768,-0.953846153846152,
-0.938461538461537,-0.923076923076922,-0.907692307692306,-0.892307692307691,
-0.876923076923076,-0.86153846153846,-0.846153846153845,-0.83076923076923,
-0.815384615384614,-0.799999999999999,-0.784615384615384,-0.769230769230768,
-0.753846153846153,-0.738461538461538,-0.723076923076922,-0.707692307692307,
-0.692307692307692,-0.676923076923076,-0.661538461538461,-0.646153846153846,
-0.63076923076923,-0.615384615384615,-0.6,-0.584615384615384,-0.569230769230769,
-0.553846153846154,-0.538461538461538,-0.523076923076923,-0.507692307692308,
-0.492307692307692,-0.476923076923077,-0.461538461538462,-0.446153846153846,
-0.430769230769231,-0.415384615384615,-0.4,-0.384615384615385,-0.369230769230769,
-0.353846153846154,-0.338461538461538,-0.323076923076923,-0.307692307692308,
-0.292307692307692,-0.276923076923077,-0.261538461538462,-0.246153846153846,
-0.230769230769231,-0.215384615384615,-0.2,-0.184615384615385,-0.169230769230769,
-0.153846153846154,-0.138461538461538,-0.123076923076923,-0.107692307692308,
-0.0923076923076923,-0.0769230769230769,-0.0615384615384615,-0.0461538461538462,
-0.0307692307692308,-0.0153846153846154,0.),.UNSPECIFIED.)
CURVE()
GEOMETRIC_REPRESENTATION_ITEM()
RATIONAL_B_SPLINE_CURVE((1.,1.,1.,1.,1.,1.,1.,1.,1.,1.,1.,1.,1.,1.,1.,1.,
1.,1.,1.,1.,1.,1.,1.,1.,1.,1.,1.,1.,1.,1.,1.,1.,1.,1.,1.,1.,1.,1.,1.,1.,
1.,1.,1.,1.,1.,1.,1.,1.,1.,1.,1.,1.,1.,1.,1.,1.,1.,1.,1.,1.,1.,1.,1.,1.,
1.,1.,1.,1.,1.,1.))
REPRESENTATION_ITEM('')
);
#205=(
BOUNDED_CURVE()
B_SPLINE_CURVE(5,(#37217,#37218,#37219,#37220,#37221,#37222,#37223,#37224,
#37225,#37226,#37227,#37228,#37229,#37230,#37231,#37232,#37233,#37234,#37235,
#37236,#37237,#37238,#37239,#37240,#37241,#37242,#37243,#37244,#37245,#37246,
#37247,#37248,#37249,#37250,#37251,#37252,#37253,#37254,#37255,#37256,#37257,
#37258,#37259,#37260,#37261,#37262,#37263,#37264,#37265,#37266,#37267,#37268,
#37269,#37270,#37271,#37272,#37273,#37274,#37275,#37276,#37277,#37278,#37279,
#37280,#37281,#37282,#37283,#37284,#37285,#37286),.UNSPECIFIED.,.F.,.F.)
B_SPLINE_CURVE_WITH_KNOTS((6,1,1,1,1,1,1,1,1,1,1,1,1,1,1,1,1,1,1,1,1,1,
1,1,1,1,1,1,1,1,1,1,1,1,1,1,1,1,1,1,1,1,1,1,1,1,1,1,1,1,1,1,1,1,1,1,1,1,
1,1,1,1,1,1,1,6),(-1.,-0.984615384615383,-0.969230769230768,-0.953846153846152,
-0.938461538461537,-0.923076923076922,-0.907692307692306,-0.892307692307691,
-0.876923076923076,-0.86153846153846,-0.846153846153845,-0.83076923076923,
-0.815384615384614,-0.799999999999999,-0.784615384615384,-0.769230769230768,
-0.753846153846153,-0.738461538461538,-0.723076923076922,-0.707692307692307,
-0.692307692307692,-0.676923076923076,-0.661538461538461,-0.646153846153846,
-0.63076923076923,-0.615384615384615,-0.6,-0.584615384615384,-0.569230769230769,
-0.553846153846154,-0.538461538461538,-0.523076923076923,-0.507692307692308,
-0.492307692307692,-0.476923076923077,-0.461538461538462,-0.446153846153846,
-0.430769230769231,-0.415384615384615,-0.4,-0.384615384615385,-0.369230769230769,
-0.353846153846154,-0.338461538461538,-0.323076923076923,-0.307692307692308,
-0.292307692307692,-0.276923076923077,-0.261538461538462,-0.246153846153846,
-0.230769230769231,-0.215384615384615,-0.2,-0.184615384615385,-0.169230769230769,
-0.153846153846154,-0.138461538461538,-0.123076923076923,-0.107692307692308,
-0.0923076923076923,-0.0769230769230769,-0.0615384615384615,-0.0461538461538462,
-0.0307692307692308,-0.0153846153846154,0.),.UNSPECIFIED.)
CURVE()
GEOMETRIC_REPRESENTATION_ITEM()
RATIONAL_B_SPLINE_CURVE((1.,1.,1.,1.,1.,1.,1.,1.,1.,1.,1.,1.,1.,1.,1.,1.,
1.,1.,1.,1.,1.,1.,1.,1.,1.,1.,1.,1.,1.,1.,1.,1.,1.,1.,1.,1.,1.,1.,1.,1.,
1.,1.,1.,1.,1.,1.,1.,1.,1.,1.,1.,1.,1.,1.,1.,1.,1.,1.,1.,1.,1.,1.,1.,1.,
1.,1.,1.,1.,1.,1.))
REPRESENTATION_ITEM('')
);
#206=(
BOUNDED_CURVE()
B_SPLINE_CURVE(5,(#37433,#37434,#37435,#37436,#37437,#37438,#37439,#37440,
#37441,#37442,#37443,#37444,#37445,#37446,#37447,#37448,#37449,#37450,#37451,
#37452,#37453,#37454,#37455,#37456,#37457,#37458,#37459,#37460,#37461,#37462,
#37463,#37464,#37465,#37466,#37467,#37468,#37469,#37470,#37471,#37472,#37473,
#37474,#37475,#37476,#37477,#37478,#37479,#37480,#37481,#37482,#37483,#37484,
#37485,#37486,#37487,#37488,#37489,#37490,#37491,#37492,#37493,#37494,#37495,
#37496,#37497,#37498,#37499,#37500,#37501,#37502),.UNSPECIFIED.,.F.,.F.)
B_SPLINE_CURVE_WITH_KNOTS((6,1,1,1,1,1,1,1,1,1,1,1,1,1,1,1,1,1,1,1,1,1,
1,1,1,1,1,1,1,1,1,1,1,1,1,1,1,1,1,1,1,1,1,1,1,1,1,1,1,1,1,1,1,1,1,1,1,1,
1,1,1,1,1,1,1,6),(-1.,-0.984615384615383,-0.969230769230768,-0.953846153846152,
-0.938461538461537,-0.923076923076922,-0.907692307692306,-0.892307692307691,
-0.876923076923076,-0.86153846153846,-0.846153846153845,-0.83076923076923,
-0.815384615384614,-0.799999999999999,-0.784615384615384,-0.769230769230768,
-0.753846153846153,-0.738461538461538,-0.723076923076922,-0.707692307692307,
-0.692307692307692,-0.676923076923076,-0.661538461538461,-0.646153846153846,
-0.63076923076923,-0.615384615384615,-0.6,-0.584615384615384,-0.569230769230769,
-0.553846153846154,-0.538461538461538,-0.523076923076923,-0.507692307692308,
-0.492307692307692,-0.476923076923077,-0.461538461538462,-0.446153846153846,
-0.430769230769231,-0.415384615384615,-0.4,-0.384615384615385,-0.369230769230769,
-0.353846153846154,-0.338461538461538,-0.323076923076923,-0.307692307692308,
-0.292307692307692,-0.276923076923077,-0.261538461538462,-0.246153846153846,
-0.230769230769231,-0.215384615384615,-0.2,-0.184615384615385,-0.169230769230769,
-0.153846153846154,-0.138461538461538,-0.123076923076923,-0.107692307692308,
-0.0923076923076923,-0.0769230769230769,-0.0615384615384615,-0.0461538461538462,
-0.0307692307692308,-0.0153846153846154,0.),.UNSPECIFIED.)
CURVE()
GEOMETRIC_REPRESENTATION_ITEM()
RATIONAL_B_SPLINE_CURVE((1.,1.,1.,1.,1.,1.,1.,1.,1.,1.,1.,1.,1.,1.,1.,1.,
1.,1.,1.,1.,1.,1.,1.,1.,1.,1.,1.,1.,1.,1.,1.,1.,1.,1.,1.,1.,1.,1.,1.,1.,
1.,1.,1.,1.,1.,1.,1.,1.,1.,1.,1.,1.,1.,1.,1.,1.,1.,1.,1.,1.,1.,1.,1.,1.,
1.,1.,1.,1.,1.,1.))
REPRESENTATION_ITEM('')
);
#207=(
BOUNDED_CURVE()
B_SPLINE_CURVE(5,(#37649,#37650,#37651,#37652,#37653,#37654,#37655,#37656,
#37657,#37658,#37659,#37660,#37661,#37662,#37663,#37664,#37665,#37666,#37667,
#37668,#37669,#37670,#37671,#37672,#37673,#37674,#37675,#37676,#37677,#37678,
#37679,#37680,#37681,#37682,#37683,#37684,#37685,#37686,#37687,#37688,#37689,
#37690,#37691,#37692,#37693,#37694,#37695,#37696,#37697,#37698,#37699,#37700,
#37701,#37702,#37703,#37704,#37705,#37706,#37707,#37708,#37709,#37710,#37711,
#37712,#37713,#37714,#37715,#37716,#37717,#37718),.UNSPECIFIED.,.F.,.F.)
B_SPLINE_CURVE_WITH_KNOTS((6,1,1,1,1,1,1,1,1,1,1,1,1,1,1,1,1,1,1,1,1,1,
1,1,1,1,1,1,1,1,1,1,1,1,1,1,1,1,1,1,1,1,1,1,1,1,1,1,1,1,1,1,1,1,1,1,1,1,
1,1,1,1,1,1,1,6),(-1.,-0.984615384615383,-0.969230769230768,-0.953846153846152,
-0.938461538461537,-0.923076923076922,-0.907692307692306,-0.892307692307691,
-0.876923076923076,-0.86153846153846,-0.846153846153845,-0.83076923076923,
-0.815384615384614,-0.799999999999999,-0.784615384615384,-0.769230769230768,
-0.753846153846153,-0.738461538461538,-0.723076923076922,-0.707692307692307,
-0.692307692307692,-0.676923076923076,-0.661538461538461,-0.646153846153846,
-0.63076923076923,-0.615384615384615,-0.6,-0.584615384615384,-0.569230769230769,
-0.553846153846154,-0.538461538461538,-0.523076923076923,-0.507692307692308,
-0.492307692307692,-0.476923076923077,-0.461538461538462,-0.446153846153846,
-0.430769230769231,-0.415384615384615,-0.4,-0.384615384615385,-0.369230769230769,
-0.353846153846154,-0.338461538461538,-0.323076923076923,-0.307692307692308,
-0.292307692307692,-0.276923076923077,-0.261538461538462,-0.246153846153846,
-0.230769230769231,-0.215384615384615,-0.2,-0.184615384615385,-0.169230769230769,
-0.153846153846154,-0.138461538461538,-0.123076923076923,-0.107692307692308,
-0.0923076923076923,-0.0769230769230769,-0.0615384615384615,-0.0461538461538462,
-0.0307692307692308,-0.0153846153846154,0.),.UNSPECIFIED.)
CURVE()
GEOMETRIC_REPRESENTATION_ITEM()
RATIONAL_B_SPLINE_CURVE((1.,1.,1.,1.,1.,1.,1.,1.,1.,1.,1.,1.,1.,1.,1.,1.,
1.,1.,1.,1.,1.,1.,1.,1.,1.,1.,1.,1.,1.,1.,1.,1.,1.,1.,1.,1.,1.,1.,1.,1.,
1.,1.,1.,1.,1.,1.,1.,1.,1.,1.,1.,1.,1.,1.,1.,1.,1.,1.,1.,1.,1.,1.,1.,1.,
1.,1.,1.,1.,1.,1.))
REPRESENTATION_ITEM('')
);
#208=(
BOUNDED_CURVE()
B_SPLINE_CURVE(5,(#37865,#37866,#37867,#37868,#37869,#37870,#37871,#37872,
#37873,#37874,#37875,#37876,#37877,#37878,#37879,#37880,#37881,#37882,#37883,
#37884,#37885,#37886,#37887,#37888,#37889,#37890,#37891,#37892,#37893,#37894,
#37895,#37896,#37897,#37898,#37899,#37900,#37901,#37902,#37903,#37904,#37905,
#37906,#37907,#37908,#37909,#37910,#37911,#37912,#37913,#37914,#37915,#37916,
#37917,#37918,#37919,#37920,#37921,#37922,#37923,#37924,#37925,#37926,#37927,
#37928,#37929,#37930,#37931,#37932,#37933,#37934),.UNSPECIFIED.,.F.,.F.)
B_SPLINE_CURVE_WITH_KNOTS((6,1,1,1,1,1,1,1,1,1,1,1,1,1,1,1,1,1,1,1,1,1,
1,1,1,1,1,1,1,1,1,1,1,1,1,1,1,1,1,1,1,1,1,1,1,1,1,1,1,1,1,1,1,1,1,1,1,1,
1,1,1,1,1,1,1,6),(-1.,-0.984615384615383,-0.969230769230768,-0.953846153846152,
-0.938461538461537,-0.923076923076922,-0.907692307692306,-0.892307692307691,
-0.876923076923076,-0.86153846153846,-0.846153846153845,-0.83076923076923,
-0.815384615384614,-0.799999999999999,-0.784615384615384,-0.769230769230768,
-0.753846153846153,-0.738461538461538,-0.723076923076922,-0.707692307692307,
-0.692307692307692,-0.676923076923076,-0.661538461538461,-0.646153846153846,
-0.63076923076923,-0.615384615384615,-0.6,-0.584615384615384,-0.569230769230769,
-0.553846153846154,-0.538461538461538,-0.523076923076923,-0.507692307692308,
-0.492307692307692,-0.476923076923077,-0.461538461538462,-0.446153846153846,
-0.430769230769231,-0.415384615384615,-0.4,-0.384615384615385,-0.369230769230769,
-0.353846153846154,-0.338461538461538,-0.323076923076923,-0.307692307692308,
-0.292307692307692,-0.276923076923077,-0.261538461538462,-0.246153846153846,
-0.230769230769231,-0.215384615384615,-0.2,-0.184615384615385,-0.169230769230769,
-0.153846153846154,-0.138461538461538,-0.123076923076923,-0.107692307692308,
-0.0923076923076923,-0.0769230769230769,-0.0615384615384615,-0.0461538461538462,
-0.0307692307692308,-0.0153846153846154,0.),.UNSPECIFIED.)
CURVE()
GEOMETRIC_REPRESENTATION_ITEM()
RATIONAL_B_SPLINE_CURVE((1.,1.,1.,1.,1.,1.,1.,1.,1.,1.,1.,1.,1.,1.,1.,1.,
1.,1.,1.,1.,1.,1.,1.,1.,1.,1.,1.,1.,1.,1.,1.,1.,1.,1.,1.,1.,1.,1.,1.,1.,
1.,1.,1.,1.,1.,1.,1.,1.,1.,1.,1.,1.,1.,1.,1.,1.,1.,1.,1.,1.,1.,1.,1.,1.,
1.,1.,1.,1.,1.,1.))
REPRESENTATION_ITEM('')
);
#209=(
BOUNDED_CURVE()
B_SPLINE_CURVE(5,(#38081,#38082,#38083,#38084,#38085,#38086,#38087,#38088,
#38089,#38090,#38091,#38092,#38093,#38094,#38095,#38096,#38097,#38098,#38099,
#38100,#38101,#38102,#38103,#38104,#38105,#38106,#38107,#38108,#38109,#38110,
#38111,#38112,#38113,#38114,#38115,#38116,#38117,#38118,#38119,#38120,#38121,
#38122,#38123,#38124,#38125,#38126,#38127,#38128,#38129,#38130,#38131,#38132,
#38133,#38134,#38135,#38136,#38137,#38138,#38139,#38140,#38141,#38142,#38143,
#38144,#38145,#38146,#38147,#38148,#38149,#38150),.UNSPECIFIED.,.F.,.F.)
B_SPLINE_CURVE_WITH_KNOTS((6,1,1,1,1,1,1,1,1,1,1,1,1,1,1,1,1,1,1,1,1,1,
1,1,1,1,1,1,1,1,1,1,1,1,1,1,1,1,1,1,1,1,1,1,1,1,1,1,1,1,1,1,1,1,1,1,1,1,
1,1,1,1,1,1,1,6),(-1.,-0.984615384615383,-0.969230769230768,-0.953846153846152,
-0.938461538461537,-0.923076923076922,-0.907692307692306,-0.892307692307691,
-0.876923076923076,-0.86153846153846,-0.846153846153845,-0.83076923076923,
-0.815384615384614,-0.799999999999999,-0.784615384615384,-0.769230769230768,
-0.753846153846153,-0.738461538461538,-0.723076923076922,-0.707692307692307,
-0.692307692307692,-0.676923076923076,-0.661538461538461,-0.646153846153846,
-0.63076923076923,-0.615384615384615,-0.6,-0.584615384615384,-0.569230769230769,
-0.553846153846154,-0.538461538461538,-0.523076923076923,-0.507692307692308,
-0.492307692307692,-0.476923076923077,-0.461538461538462,-0.446153846153846,
-0.430769230769231,-0.415384615384615,-0.4,-0.384615384615385,-0.369230769230769,
-0.353846153846154,-0.338461538461538,-0.323076923076923,-0.307692307692308,
-0.292307692307692,-0.276923076923077,-0.261538461538462,-0.246153846153846,
-0.230769230769231,-0.215384615384615,-0.2,-0.184615384615385,-0.169230769230769,
-0.153846153846154,-0.138461538461538,-0.123076923076923,-0.107692307692308,
-0.0923076923076923,-0.0769230769230769,-0.0615384615384615,-0.0461538461538462,
-0.0307692307692308,-0.0153846153846154,0.),.UNSPECIFIED.)
CURVE()
GEOMETRIC_REPRESENTATION_ITEM()
RATIONAL_B_SPLINE_CURVE((1.,1.,1.,1.,1.,1.,1.,1.,1.,1.,1.,1.,1.,1.,1.,1.,
1.,1.,1.,1.,1.,1.,1.,1.,1.,1.,1.,1.,1.,1.,1.,1.,1.,1.,1.,1.,1.,1.,1.,1.,
1.,1.,1.,1.,1.,1.,1.,1.,1.,1.,1.,1.,1.,1.,1.,1.,1.,1.,1.,1.,1.,1.,1.,1.,
1.,1.,1.,1.,1.,1.))
REPRESENTATION_ITEM('')
);
#210=(
BOUNDED_CURVE()
B_SPLINE_CURVE(5,(#38297,#38298,#38299,#38300,#38301,#38302,#38303,#38304,
#38305,#38306,#38307,#38308,#38309,#38310,#38311,#38312,#38313,#38314,#38315,
#38316,#38317,#38318,#38319,#38320,#38321,#38322,#38323,#38324,#38325,#38326,
#38327,#38328,#38329,#38330,#38331,#38332,#38333,#38334,#38335,#38336,#38337,
#38338,#38339,#38340,#38341,#38342,#38343,#38344,#38345,#38346,#38347,#38348,
#38349,#38350,#38351,#38352,#38353,#38354,#38355,#38356,#38357,#38358,#38359,
#38360,#38361,#38362,#38363,#38364,#38365,#38366),.UNSPECIFIED.,.F.,.F.)
B_SPLINE_CURVE_WITH_KNOTS((6,1,1,1,1,1,1,1,1,1,1,1,1,1,1,1,1,1,1,1,1,1,
1,1,1,1,1,1,1,1,1,1,1,1,1,1,1,1,1,1,1,1,1,1,1,1,1,1,1,1,1,1,1,1,1,1,1,1,
1,1,1,1,1,1,1,6),(-1.,-0.984615384615383,-0.969230769230768,-0.953846153846152,
-0.938461538461537,-0.923076923076922,-0.907692307692306,-0.892307692307691,
-0.876923076923076,-0.86153846153846,-0.846153846153845,-0.83076923076923,
-0.815384615384614,-0.799999999999999,-0.784615384615384,-0.769230769230768,
-0.753846153846153,-0.738461538461538,-0.723076923076922,-0.707692307692307,
-0.692307692307692,-0.676923076923076,-0.661538461538461,-0.646153846153846,
-0.63076923076923,-0.615384615384615,-0.6,-0.584615384615384,-0.569230769230769,
-0.553846153846154,-0.538461538461538,-0.523076923076923,-0.507692307692308,
-0.492307692307692,-0.476923076923077,-0.461538461538462,-0.446153846153846,
-0.430769230769231,-0.415384615384615,-0.4,-0.384615384615385,-0.369230769230769,
-0.353846153846154,-0.338461538461538,-0.323076923076923,-0.307692307692308,
-0.292307692307692,-0.276923076923077,-0.261538461538462,-0.246153846153846,
-0.230769230769231,-0.215384615384615,-0.2,-0.184615384615385,-0.169230769230769,
-0.153846153846154,-0.138461538461538,-0.123076923076923,-0.107692307692308,
-0.0923076923076923,-0.0769230769230769,-0.0615384615384615,-0.0461538461538462,
-0.0307692307692308,-0.0153846153846154,0.),.UNSPECIFIED.)
CURVE()
GEOMETRIC_REPRESENTATION_ITEM()
RATIONAL_B_SPLINE_CURVE((1.,1.,1.,1.,1.,1.,1.,1.,1.,1.,1.,1.,1.,1.,1.,1.,
1.,1.,1.,1.,1.,1.,1.,1.,1.,1.,1.,1.,1.,1.,1.,1.,1.,1.,1.,1.,1.,1.,1.,1.,
1.,1.,1.,1.,1.,1.,1.,1.,1.,1.,1.,1.,1.,1.,1.,1.,1.,1.,1.,1.,1.,1.,1.,1.,
1.,1.,1.,1.,1.,1.))
REPRESENTATION_ITEM('')
);
#211=(
BOUNDED_CURVE()
B_SPLINE_CURVE(5,(#38781,#38782,#38783,#38784,#38785,#38786,#38787,#38788,
#38789,#38790,#38791,#38792,#38793,#38794,#38795,#38796,#38797,#38798,#38799,
#38800,#38801,#38802,#38803,#38804,#38805,#38806,#38807,#38808,#38809,#38810,
#38811,#38812,#38813,#38814,#38815,#38816,#38817,#38818,#38819,#38820,#38821,
#38822,#38823,#38824,#38825,#38826,#38827,#38828,#38829,#38830,#38831,#38832,
#38833,#38834,#38835,#38836,#38837,#38838,#38839,#38840,#38841,#38842,#38843,
#38844,#38845,#38846,#38847,#38848,#38849,#38850),.UNSPECIFIED.,.F.,.F.)
B_SPLINE_CURVE_WITH_KNOTS((6,1,1,1,1,1,1,1,1,1,1,1,1,1,1,1,1,1,1,1,1,1,
1,1,1,1,1,1,1,1,1,1,1,1,1,1,1,1,1,1,1,1,1,1,1,1,1,1,1,1,1,1,1,1,1,1,1,1,
1,1,1,1,1,1,1,6),(0.00577184337450058,0.0153846153846154,0.0307692307692308,
0.0461538461538462,0.0615384615384615,0.0769230769230769,0.0923076923076923,
0.107692307692308,0.123076923076923,0.138461538461538,0.153846153846154,
0.169230769230769,0.184615384615385,0.2,0.215384615384615,0.230769230769231,
0.246153846153846,0.261538461538462,0.276923076923077,0.292307692307692,
0.307692307692308,0.323076923076923,0.338461538461538,0.353846153846154,
0.369230769230769,0.384615384615385,0.4,0.415384615384615,0.430769230769231,
0.446153846153846,0.461538461538462,0.476923076923077,0.492307692307692,
0.507692307692308,0.523076923076923,0.538461538461538,0.553846153846154,
0.569230769230769,0.584615384615384,0.6,0.615384615384615,0.63076923076923,
0.646153846153846,0.661538461538461,0.676923076923076,0.692307692307692,
0.707692307692307,0.723076923076922,0.738461538461538,0.753846153846153,
0.769230769230768,0.784615384615384,0.799999999999999,0.815384615384614,
0.83076923076923,0.846153846153845,0.86153846153846,0.876923076923076,0.892307692307691,
0.907692307692306,0.923076923076922,0.938461538461537,0.953846153846152,
0.969230769230768,0.984615384615383,1.),.UNSPECIFIED.)
CURVE()
GEOMETRIC_REPRESENTATION_ITEM()
RATIONAL_B_SPLINE_CURVE((1.,1.,1.,1.,1.,1.,1.,1.,1.,1.,1.,1.,1.,1.,1.,1.,
1.,1.,1.,1.,1.,1.,1.,1.,1.,1.,1.,1.,1.,1.,1.,1.,1.,1.,1.,1.,1.,1.,1.,1.,
1.,1.,1.,1.,1.,1.,1.,1.,1.,1.,1.,1.,1.,1.,1.,1.,1.,1.,1.,1.,1.,1.,1.,1.,
1.,1.,1.,1.,1.,1.))
REPRESENTATION_ITEM('')
);
#212=(
BOUNDED_CURVE()
B_SPLINE_CURVE(5,(#38854,#38855,#38856,#38857,#38858,#38859,#38860,#38861,
#38862,#38863,#38864,#38865,#38866,#38867,#38868,#38869,#38870,#38871,#38872,
#38873,#38874,#38875,#38876,#38877,#38878,#38879,#38880,#38881,#38882,#38883,
#38884,#38885,#38886,#38887,#38888,#38889,#38890,#38891,#38892,#38893,#38894,
#38895,#38896,#38897,#38898,#38899,#38900,#38901,#38902,#38903,#38904,#38905,
#38906,#38907,#38908,#38909,#38910,#38911,#38912,#38913,#38914,#38915,#38916,
#38917,#38918,#38919,#38920,#38921,#38922,#38923),.UNSPECIFIED.,.F.,.F.)
B_SPLINE_CURVE_WITH_KNOTS((6,1,1,1,1,1,1,1,1,1,1,1,1,1,1,1,1,1,1,1,1,1,
1,1,1,1,1,1,1,1,1,1,1,1,1,1,1,1,1,1,1,1,1,1,1,1,1,1,1,1,1,1,1,1,1,1,1,1,
1,1,1,1,1,1,1,6),(0.,0.0153846153846154,0.0307692307692308,0.0461538461538462,
0.0615384615384615,0.0769230769230769,0.0923076923076923,0.107692307692308,
0.123076923076923,0.138461538461538,0.153846153846154,0.169230769230769,
0.184615384615385,0.2,0.215384615384615,0.230769230769231,0.246153846153846,
0.261538461538462,0.276923076923077,0.292307692307692,0.307692307692308,
0.323076923076923,0.338461538461538,0.353846153846154,0.369230769230769,
0.384615384615385,0.4,0.415384615384615,0.430769230769231,0.446153846153846,
0.461538461538462,0.476923076923077,0.492307692307692,0.507692307692308,
0.523076923076923,0.538461538461538,0.553846153846154,0.569230769230769,
0.584615384615384,0.6,0.615384615384615,0.63076923076923,0.646153846153846,
0.661538461538461,0.676923076923076,0.692307692307692,0.707692307692307,
0.723076923076922,0.738461538461538,0.753846153846153,0.769230769230768,
0.784615384615384,0.799999999999999,0.815384615384614,0.83076923076923,
0.846153846153845,0.86153846153846,0.876923076923076,0.892307692307691,
0.907692307692306,0.923076923076922,0.938461538461537,0.953846153846152,
0.969230769230768,0.984615384615383,0.994228156739708),.UNSPECIFIED.)
CURVE()
GEOMETRIC_REPRESENTATION_ITEM()
RATIONAL_B_SPLINE_CURVE((1.,1.,1.,1.,1.,1.,1.,1.,1.,1.,1.,1.,1.,1.,1.,1.,
1.,1.,1.,1.,1.,1.,1.,1.,1.,1.,1.,1.,1.,1.,1.,1.,1.,1.,1.,1.,1.,1.,1.,1.,
1.,1.,1.,1.,1.,1.,1.,1.,1.,1.,1.,1.,1.,1.,1.,1.,1.,1.,1.,1.,1.,1.,1.,1.,
1.,1.,1.,1.,1.,1.))
REPRESENTATION_ITEM('')
);
#213=(
BOUNDED_CURVE()
B_SPLINE_CURVE(5,(#38927,#38928,#38929,#38930,#38931,#38932,#38933,#38934,
#38935,#38936,#38937,#38938,#38939,#38940,#38941,#38942,#38943,#38944,#38945,
#38946,#38947,#38948,#38949,#38950,#38951,#38952,#38953,#38954,#38955,#38956,
#38957,#38958,#38959,#38960,#38961,#38962,#38963,#38964,#38965,#38966,#38967,
#38968,#38969,#38970,#38971,#38972,#38973,#38974,#38975,#38976,#38977,#38978,
#38979,#38980,#38981,#38982,#38983,#38984,#38985,#38986,#38987,#38988,#38989,
#38990,#38991,#38992,#38993,#38994,#38995,#38996),.UNSPECIFIED.,.F.,.F.)
B_SPLINE_CURVE_WITH_KNOTS((6,1,1,1,1,1,1,1,1,1,1,1,1,1,1,1,1,1,1,1,1,1,
1,1,1,1,1,1,1,1,1,1,1,1,1,1,1,1,1,1,1,1,1,1,1,1,1,1,1,1,1,1,1,1,1,1,1,1,
1,1,1,1,1,1,1,6),(0.0057718433745091,0.0153846153846154,0.0307692307692308,
0.0461538461538462,0.0615384615384615,0.0769230769230769,0.0923076923076923,
0.107692307692308,0.123076923076923,0.138461538461538,0.153846153846154,
0.169230769230769,0.184615384615385,0.2,0.215384615384615,0.230769230769231,
0.246153846153846,0.261538461538462,0.276923076923077,0.292307692307692,
0.307692307692308,0.323076923076923,0.338461538461538,0.353846153846154,
0.369230769230769,0.384615384615385,0.4,0.415384615384615,0.430769230769231,
0.446153846153846,0.461538461538462,0.476923076923077,0.492307692307692,
0.507692307692308,0.523076923076923,0.538461538461538,0.553846153846154,
0.569230769230769,0.584615384615384,0.6,0.615384615384615,0.63076923076923,
0.646153846153846,0.661538461538461,0.676923076923076,0.692307692307692,
0.707692307692307,0.723076923076922,0.738461538461538,0.753846153846153,
0.769230769230768,0.784615384615384,0.799999999999999,0.815384615384614,
0.83076923076923,0.846153846153845,0.86153846153846,0.876923076923076,0.892307692307691,
0.907692307692306,0.923076923076922,0.938461538461537,0.953846153846152,
0.969230769230768,0.984615384615383,1.),.UNSPECIFIED.)
CURVE()
GEOMETRIC_REPRESENTATION_ITEM()
RATIONAL_B_SPLINE_CURVE((1.,1.,1.,1.,1.,1.,1.,1.,1.,1.,1.,1.,1.,1.,1.,1.,
1.,1.,1.,1.,1.,1.,1.,1.,1.,1.,1.,1.,1.,1.,1.,1.,1.,1.,1.,1.,1.,1.,1.,1.,
1.,1.,1.,1.,1.,1.,1.,1.,1.,1.,1.,1.,1.,1.,1.,1.,1.,1.,1.,1.,1.,1.,1.,1.,
1.,1.,1.,1.,1.,1.))
REPRESENTATION_ITEM('')
);
#214=(
BOUNDED_CURVE()
B_SPLINE_CURVE(5,(#39000,#39001,#39002,#39003,#39004,#39005,#39006,#39007,
#39008,#39009,#39010,#39011,#39012,#39013,#39014,#39015,#39016,#39017,#39018,
#39019,#39020,#39021,#39022,#39023,#39024,#39025,#39026,#39027,#39028,#39029,
#39030,#39031,#39032,#39033,#39034,#39035,#39036,#39037,#39038,#39039,#39040,
#39041,#39042,#39043,#39044,#39045,#39046,#39047,#39048,#39049,#39050,#39051,
#39052,#39053,#39054,#39055,#39056,#39057,#39058,#39059,#39060,#39061,#39062,
#39063,#39064,#39065,#39066,#39067,#39068,#39069),.UNSPECIFIED.,.F.,.F.)
B_SPLINE_CURVE_WITH_KNOTS((6,1,1,1,1,1,1,1,1,1,1,1,1,1,1,1,1,1,1,1,1,1,
1,1,1,1,1,1,1,1,1,1,1,1,1,1,1,1,1,1,1,1,1,1,1,1,1,1,1,1,1,1,1,1,1,1,1,1,
1,1,1,1,1,1,1,6),(0.,0.0153846153846154,0.0307692307692308,0.0461538461538462,
0.0615384615384615,0.0769230769230769,0.0923076923076923,0.107692307692308,
0.123076923076923,0.138461538461538,0.153846153846154,0.169230769230769,
0.184615384615385,0.2,0.215384615384615,0.230769230769231,0.246153846153846,
0.261538461538462,0.276923076923077,0.292307692307692,0.307692307692308,
0.323076923076923,0.338461538461538,0.353846153846154,0.369230769230769,
0.384615384615385,0.4,0.415384615384615,0.430769230769231,0.446153846153846,
0.461538461538462,0.476923076923077,0.492307692307692,0.507692307692308,
0.523076923076923,0.538461538461538,0.553846153846154,0.569230769230769,
0.584615384615384,0.6,0.615384615384615,0.63076923076923,0.646153846153846,
0.661538461538461,0.676923076923076,0.692307692307692,0.707692307692307,
0.723076923076922,0.738461538461538,0.753846153846153,0.769230769230768,
0.784615384615384,0.799999999999999,0.815384615384614,0.83076923076923,
0.846153846153845,0.86153846153846,0.876923076923076,0.892307692307691,
0.907692307692306,0.923076923076922,0.938461538461537,0.953846153846152,
0.969230769230768,0.984615384615383,0.994228156739689),.UNSPECIFIED.)
CURVE()
GEOMETRIC_REPRESENTATION_ITEM()
RATIONAL_B_SPLINE_CURVE((1.,1.,1.,1.,1.,1.,1.,1.,1.,1.,1.,1.,1.,1.,1.,1.,
1.,1.,1.,1.,1.,1.,1.,1.,1.,1.,1.,1.,1.,1.,1.,1.,1.,1.,1.,1.,1.,1.,1.,1.,
1.,1.,1.,1.,1.,1.,1.,1.,1.,1.,1.,1.,1.,1.,1.,1.,1.,1.,1.,1.,1.,1.,1.,1.,
1.,1.,1.,1.,1.,1.))
REPRESENTATION_ITEM('')
);
#215=(
BOUNDED_CURVE()
B_SPLINE_CURVE(5,(#39073,#39074,#39075,#39076,#39077,#39078,#39079,#39080,
#39081,#39082,#39083,#39084,#39085,#39086,#39087,#39088,#39089,#39090,#39091,
#39092,#39093,#39094,#39095,#39096,#39097,#39098,#39099,#39100,#39101,#39102,
#39103,#39104,#39105,#39106,#39107,#39108,#39109,#39110,#39111,#39112,#39113,
#39114,#39115,#39116,#39117,#39118,#39119,#39120,#39121,#39122,#39123,#39124,
#39125,#39126,#39127,#39128,#39129,#39130,#39131,#39132,#39133,#39134,#39135,
#39136,#39137,#39138,#39139,#39140,#39141,#39142),.UNSPECIFIED.,.F.,.F.)
B_SPLINE_CURVE_WITH_KNOTS((6,1,1,1,1,1,1,1,1,1,1,1,1,1,1,1,1,1,1,1,1,1,
1,1,1,1,1,1,1,1,1,1,1,1,1,1,1,1,1,1,1,1,1,1,1,1,1,1,1,1,1,1,1,1,1,1,1,1,
1,1,1,1,1,1,1,6),(0.00577184337448946,0.0153846153846154,0.0307692307692308,
0.0461538461538462,0.0615384615384615,0.0769230769230769,0.0923076923076923,
0.107692307692308,0.123076923076923,0.138461538461538,0.153846153846154,
0.169230769230769,0.184615384615385,0.2,0.215384615384615,0.230769230769231,
0.246153846153846,0.261538461538462,0.276923076923077,0.292307692307692,
0.307692307692308,0.323076923076923,0.338461538461538,0.353846153846154,
0.369230769230769,0.384615384615385,0.4,0.415384615384615,0.430769230769231,
0.446153846153846,0.461538461538462,0.476923076923077,0.492307692307692,
0.507692307692308,0.523076923076923,0.538461538461538,0.553846153846154,
0.569230769230769,0.584615384615384,0.6,0.615384615384615,0.63076923076923,
0.646153846153846,0.661538461538461,0.676923076923076,0.692307692307692,
0.707692307692307,0.723076923076922,0.738461538461538,0.753846153846153,
0.769230769230768,0.784615384615384,0.799999999999999,0.815384615384614,
0.83076923076923,0.846153846153845,0.86153846153846,0.876923076923076,0.892307692307691,
0.907692307692306,0.923076923076922,0.938461538461537,0.953846153846152,
0.969230769230768,0.984615384615383,1.),.UNSPECIFIED.)
CURVE()
GEOMETRIC_REPRESENTATION_ITEM()
RATIONAL_B_SPLINE_CURVE((1.,1.,1.,1.,1.,1.,1.,1.,1.,1.,1.,1.,1.,1.,1.,1.,
1.,1.,1.,1.,1.,1.,1.,1.,1.,1.,1.,1.,1.,1.,1.,1.,1.,1.,1.,1.,1.,1.,1.,1.,
1.,1.,1.,1.,1.,1.,1.,1.,1.,1.,1.,1.,1.,1.,1.,1.,1.,1.,1.,1.,1.,1.,1.,1.,
1.,1.,1.,1.,1.,1.))
REPRESENTATION_ITEM('')
);
#216=(
BOUNDED_CURVE()
B_SPLINE_CURVE(5,(#39146,#39147,#39148,#39149,#39150,#39151,#39152,#39153,
#39154,#39155,#39156,#39157,#39158,#39159,#39160,#39161,#39162,#39163,#39164,
#39165,#39166,#39167,#39168,#39169,#39170,#39171,#39172,#39173,#39174,#39175,
#39176,#39177,#39178,#39179,#39180,#39181,#39182,#39183,#39184,#39185,#39186,
#39187,#39188,#39189,#39190,#39191,#39192,#39193,#39194,#39195,#39196,#39197,
#39198,#39199,#39200,#39201,#39202,#39203,#39204,#39205,#39206,#39207,#39208,
#39209,#39210,#39211,#39212,#39213,#39214,#39215),.UNSPECIFIED.,.F.,.F.)
B_SPLINE_CURVE_WITH_KNOTS((6,1,1,1,1,1,1,1,1,1,1,1,1,1,1,1,1,1,1,1,1,1,
1,1,1,1,1,1,1,1,1,1,1,1,1,1,1,1,1,1,1,1,1,1,1,1,1,1,1,1,1,1,1,1,1,1,1,1,
1,1,1,1,1,1,1,6),(0.,0.0153846153846154,0.0307692307692308,0.0461538461538462,
0.0615384615384615,0.0769230769230769,0.0923076923076923,0.107692307692308,
0.123076923076923,0.138461538461538,0.153846153846154,0.169230769230769,
0.184615384615385,0.2,0.215384615384615,0.230769230769231,0.246153846153846,
0.261538461538462,0.276923076923077,0.292307692307692,0.307692307692308,
0.323076923076923,0.338461538461538,0.353846153846154,0.369230769230769,
0.384615384615385,0.4,0.415384615384615,0.430769230769231,0.446153846153846,
0.461538461538462,0.476923076923077,0.492307692307692,0.507692307692308,
0.523076923076923,0.538461538461538,0.553846153846154,0.569230769230769,
0.584615384615384,0.6,0.615384615384615,0.63076923076923,0.646153846153846,
0.661538461538461,0.676923076923076,0.692307692307692,0.707692307692307,
0.723076923076922,0.738461538461538,0.753846153846153,0.769230769230768,
0.784615384615384,0.799999999999999,0.815384615384614,0.83076923076923,
0.846153846153845,0.86153846153846,0.876923076923076,0.892307692307691,
0.907692307692306,0.923076923076922,0.938461538461537,0.953846153846152,
0.969230769230768,0.984615384615383,0.994228156739718),.UNSPECIFIED.)
CURVE()
GEOMETRIC_REPRESENTATION_ITEM()
RATIONAL_B_SPLINE_CURVE((1.,1.,1.,1.,1.,1.,1.,1.,1.,1.,1.,1.,1.,1.,1.,1.,
1.,1.,1.,1.,1.,1.,1.,1.,1.,1.,1.,1.,1.,1.,1.,1.,1.,1.,1.,1.,1.,1.,1.,1.,
1.,1.,1.,1.,1.,1.,1.,1.,1.,1.,1.,1.,1.,1.,1.,1.,1.,1.,1.,1.,1.,1.,1.,1.,
1.,1.,1.,1.,1.,1.))
REPRESENTATION_ITEM('')
);
#217=(
BOUNDED_CURVE()
B_SPLINE_CURVE(5,(#39219,#39220,#39221,#39222,#39223,#39224,#39225,#39226,
#39227,#39228,#39229,#39230,#39231,#39232,#39233,#39234,#39235,#39236,#39237,
#39238,#39239,#39240,#39241,#39242,#39243,#39244,#39245,#39246,#39247,#39248,
#39249,#39250,#39251,#39252,#39253,#39254,#39255,#39256,#39257,#39258,#39259,
#39260,#39261,#39262,#39263,#39264,#39265,#39266,#39267,#39268,#39269,#39270,
#39271,#39272,#39273,#39274,#39275,#39276,#39277,#39278,#39279,#39280,#39281,
#39282,#39283,#39284,#39285,#39286,#39287,#39288),.UNSPECIFIED.,.F.,.F.)
B_SPLINE_CURVE_WITH_KNOTS((6,1,1,1,1,1,1,1,1,1,1,1,1,1,1,1,1,1,1,1,1,1,
1,1,1,1,1,1,1,1,1,1,1,1,1,1,1,1,1,1,1,1,1,1,1,1,1,1,1,1,1,1,1,1,1,1,1,1,
1,1,1,1,1,1,1,6),(0.00577184337450897,0.0153846153846154,0.0307692307692308,
0.0461538461538462,0.0615384615384615,0.0769230769230769,0.0923076923076923,
0.107692307692308,0.123076923076923,0.138461538461538,0.153846153846154,
0.169230769230769,0.184615384615385,0.2,0.215384615384615,0.230769230769231,
0.246153846153846,0.261538461538462,0.276923076923077,0.292307692307692,
0.307692307692308,0.323076923076923,0.338461538461538,0.353846153846154,
0.369230769230769,0.384615384615385,0.4,0.415384615384615,0.430769230769231,
0.446153846153846,0.461538461538462,0.476923076923077,0.492307692307692,
0.507692307692308,0.523076923076923,0.538461538461538,0.553846153846154,
0.569230769230769,0.584615384615384,0.6,0.615384615384615,0.63076923076923,
0.646153846153846,0.661538461538461,0.676923076923076,0.692307692307692,
0.707692307692307,0.723076923076922,0.738461538461538,0.753846153846153,
0.769230769230768,0.784615384615384,0.799999999999999,0.815384615384614,
0.83076923076923,0.846153846153845,0.86153846153846,0.876923076923076,0.892307692307691,
0.907692307692306,0.923076923076922,0.938461538461537,0.953846153846152,
0.969230769230768,0.984615384615383,1.),.UNSPECIFIED.)
CURVE()
GEOMETRIC_REPRESENTATION_ITEM()
RATIONAL_B_SPLINE_CURVE((1.,1.,1.,1.,1.,1.,1.,1.,1.,1.,1.,1.,1.,1.,1.,1.,
1.,1.,1.,1.,1.,1.,1.,1.,1.,1.,1.,1.,1.,1.,1.,1.,1.,1.,1.,1.,1.,1.,1.,1.,
1.,1.,1.,1.,1.,1.,1.,1.,1.,1.,1.,1.,1.,1.,1.,1.,1.,1.,1.,1.,1.,1.,1.,1.,
1.,1.,1.,1.,1.,1.))
REPRESENTATION_ITEM('')
);
#218=(
BOUNDED_CURVE()
B_SPLINE_CURVE(5,(#39292,#39293,#39294,#39295,#39296,#39297,#39298,#39299,
#39300,#39301,#39302,#39303,#39304,#39305,#39306,#39307,#39308,#39309,#39310,
#39311,#39312,#39313,#39314,#39315,#39316,#39317,#39318,#39319,#39320,#39321,
#39322,#39323,#39324,#39325,#39326,#39327,#39328,#39329,#39330,#39331,#39332,
#39333,#39334,#39335,#39336,#39337,#39338,#39339,#39340,#39341,#39342,#39343,
#39344,#39345,#39346,#39347,#39348,#39349,#39350,#39351,#39352,#39353,#39354,
#39355,#39356,#39357,#39358,#39359,#39360,#39361),.UNSPECIFIED.,.F.,.F.)
B_SPLINE_CURVE_WITH_KNOTS((6,1,1,1,1,1,1,1,1,1,1,1,1,1,1,1,1,1,1,1,1,1,
1,1,1,1,1,1,1,1,1,1,1,1,1,1,1,1,1,1,1,1,1,1,1,1,1,1,1,1,1,1,1,1,1,1,1,1,
1,1,1,1,1,1,1,6),(0.,0.0153846153846154,0.0307692307692308,0.0461538461538462,
0.0615384615384615,0.0769230769230769,0.0923076923076923,0.107692307692308,
0.123076923076923,0.138461538461538,0.153846153846154,0.169230769230769,
0.184615384615385,0.2,0.215384615384615,0.230769230769231,0.246153846153846,
0.261538461538462,0.276923076923077,0.292307692307692,0.307692307692308,
0.323076923076923,0.338461538461538,0.353846153846154,0.369230769230769,
0.384615384615385,0.4,0.415384615384615,0.430769230769231,0.446153846153846,
0.461538461538462,0.476923076923077,0.492307692307692,0.507692307692308,
0.523076923076923,0.538461538461538,0.553846153846154,0.569230769230769,
0.584615384615384,0.6,0.615384615384615,0.63076923076923,0.646153846153846,
0.661538461538461,0.676923076923076,0.692307692307692,0.707692307692307,
0.723076923076922,0.738461538461538,0.753846153846153,0.769230769230768,
0.784615384615384,0.799999999999999,0.815384615384614,0.83076923076923,
0.846153846153845,0.86153846153846,0.876923076923076,0.892307692307691,
0.907692307692306,0.923076923076922,0.938461538461537,0.953846153846152,
0.969230769230768,0.984615384615383,0.994228156739701),.UNSPECIFIED.)
CURVE()
GEOMETRIC_REPRESENTATION_ITEM()
RATIONAL_B_SPLINE_CURVE((1.,1.,1.,1.,1.,1.,1.,1.,1.,1.,1.,1.,1.,1.,1.,1.,
1.,1.,1.,1.,1.,1.,1.,1.,1.,1.,1.,1.,1.,1.,1.,1.,1.,1.,1.,1.,1.,1.,1.,1.,
1.,1.,1.,1.,1.,1.,1.,1.,1.,1.,1.,1.,1.,1.,1.,1.,1.,1.,1.,1.,1.,1.,1.,1.,
1.,1.,1.,1.,1.,1.))
REPRESENTATION_ITEM('')
);
#219=(
BOUNDED_CURVE()
B_SPLINE_CURVE(5,(#39365,#39366,#39367,#39368,#39369,#39370,#39371,#39372,
#39373,#39374,#39375,#39376,#39377,#39378,#39379,#39380,#39381,#39382,#39383,
#39384,#39385,#39386,#39387,#39388,#39389,#39390,#39391,#39392,#39393,#39394,
#39395,#39396,#39397,#39398,#39399,#39400,#39401,#39402,#39403,#39404,#39405,
#39406,#39407,#39408,#39409,#39410,#39411,#39412,#39413,#39414,#39415,#39416,
#39417,#39418,#39419,#39420,#39421,#39422,#39423,#39424,#39425,#39426,#39427,
#39428,#39429,#39430,#39431,#39432,#39433,#39434),.UNSPECIFIED.,.F.,.F.)
B_SPLINE_CURVE_WITH_KNOTS((6,1,1,1,1,1,1,1,1,1,1,1,1,1,1,1,1,1,1,1,1,1,
1,1,1,1,1,1,1,1,1,1,1,1,1,1,1,1,1,1,1,1,1,1,1,1,1,1,1,1,1,1,1,1,1,1,1,1,
1,1,1,1,1,1,1,6),(0.00577184337451001,0.0153846153846154,0.0307692307692308,
0.0461538461538462,0.0615384615384615,0.0769230769230769,0.0923076923076923,
0.107692307692308,0.123076923076923,0.138461538461538,0.153846153846154,
0.169230769230769,0.184615384615385,0.2,0.215384615384615,0.230769230769231,
0.246153846153846,0.261538461538462,0.276923076923077,0.292307692307692,
0.307692307692308,0.323076923076923,0.338461538461538,0.353846153846154,
0.369230769230769,0.384615384615385,0.4,0.415384615384615,0.430769230769231,
0.446153846153846,0.461538461538462,0.476923076923077,0.492307692307692,
0.507692307692308,0.523076923076923,0.538461538461538,0.553846153846154,
0.569230769230769,0.584615384615384,0.6,0.615384615384615,0.63076923076923,
0.646153846153846,0.661538461538461,0.676923076923076,0.692307692307692,
0.707692307692307,0.723076923076922,0.738461538461538,0.753846153846153,
0.769230769230768,0.784615384615384,0.799999999999999,0.815384615384614,
0.83076923076923,0.846153846153845,0.86153846153846,0.876923076923076,0.892307692307691,
0.907692307692306,0.923076923076922,0.938461538461537,0.953846153846152,
0.969230769230768,0.984615384615383,1.),.UNSPECIFIED.)
CURVE()
GEOMETRIC_REPRESENTATION_ITEM()
RATIONAL_B_SPLINE_CURVE((1.,1.,1.,1.,1.,1.,1.,1.,1.,1.,1.,1.,1.,1.,1.,1.,
1.,1.,1.,1.,1.,1.,1.,1.,1.,1.,1.,1.,1.,1.,1.,1.,1.,1.,1.,1.,1.,1.,1.,1.,
1.,1.,1.,1.,1.,1.,1.,1.,1.,1.,1.,1.,1.,1.,1.,1.,1.,1.,1.,1.,1.,1.,1.,1.,
1.,1.,1.,1.,1.,1.))
REPRESENTATION_ITEM('')
);
#220=(
BOUNDED_CURVE()
B_SPLINE_CURVE(5,(#39438,#39439,#39440,#39441,#39442,#39443,#39444,#39445,
#39446,#39447,#39448,#39449,#39450,#39451,#39452,#39453,#39454,#39455,#39456,
#39457,#39458,#39459,#39460,#39461,#39462,#39463,#39464,#39465,#39466,#39467,
#39468,#39469,#39470,#39471,#39472,#39473,#39474,#39475,#39476,#39477,#39478,
#39479,#39480,#39481,#39482,#39483,#39484,#39485,#39486,#39487,#39488,#39489,
#39490,#39491,#39492,#39493,#39494,#39495,#39496,#39497,#39498,#39499,#39500,
#39501,#39502,#39503,#39504,#39505,#39506,#39507),.UNSPECIFIED.,.F.,.F.)
B_SPLINE_CURVE_WITH_KNOTS((6,1,1,1,1,1,1,1,1,1,1,1,1,1,1,1,1,1,1,1,1,1,
1,1,1,1,1,1,1,1,1,1,1,1,1,1,1,1,1,1,1,1,1,1,1,1,1,1,1,1,1,1,1,1,1,1,1,1,
1,1,1,1,1,1,1,6),(0.,0.0153846153846154,0.0307692307692308,0.0461538461538462,
0.0615384615384615,0.0769230769230769,0.0923076923076923,0.107692307692308,
0.123076923076923,0.138461538461538,0.153846153846154,0.169230769230769,
0.184615384615385,0.2,0.215384615384615,0.230769230769231,0.246153846153846,
0.261538461538462,0.276923076923077,0.292307692307692,0.307692307692308,
0.323076923076923,0.338461538461538,0.353846153846154,0.369230769230769,
0.384615384615385,0.4,0.415384615384615,0.430769230769231,0.446153846153846,
0.461538461538462,0.476923076923077,0.492307692307692,0.507692307692308,
0.523076923076923,0.538461538461538,0.553846153846154,0.569230769230769,
0.584615384615384,0.6,0.615384615384615,0.63076923076923,0.646153846153846,
0.661538461538461,0.676923076923076,0.692307692307692,0.707692307692307,
0.723076923076922,0.738461538461538,0.753846153846153,0.769230769230768,
0.784615384615384,0.799999999999999,0.815384615384614,0.83076923076923,
0.846153846153845,0.86153846153846,0.876923076923076,0.892307692307691,
0.907692307692306,0.923076923076922,0.938461538461537,0.953846153846152,
0.969230769230768,0.984615384615383,0.994228156739697),.UNSPECIFIED.)
CURVE()
GEOMETRIC_REPRESENTATION_ITEM()
RATIONAL_B_SPLINE_CURVE((1.,1.,1.,1.,1.,1.,1.,1.,1.,1.,1.,1.,1.,1.,1.,1.,
1.,1.,1.,1.,1.,1.,1.,1.,1.,1.,1.,1.,1.,1.,1.,1.,1.,1.,1.,1.,1.,1.,1.,1.,
1.,1.,1.,1.,1.,1.,1.,1.,1.,1.,1.,1.,1.,1.,1.,1.,1.,1.,1.,1.,1.,1.,1.,1.,
1.,1.,1.,1.,1.,1.))
REPRESENTATION_ITEM('')
);
#221=(
BOUNDED_CURVE()
B_SPLINE_CURVE(5,(#39511,#39512,#39513,#39514,#39515,#39516,#39517,#39518,
#39519,#39520,#39521,#39522,#39523,#39524,#39525,#39526,#39527,#39528,#39529,
#39530,#39531,#39532,#39533,#39534,#39535,#39536,#39537,#39538,#39539,#39540,
#39541,#39542,#39543,#39544,#39545,#39546,#39547,#39548,#39549,#39550,#39551,
#39552,#39553,#39554,#39555,#39556,#39557,#39558,#39559,#39560,#39561,#39562,
#39563,#39564,#39565,#39566,#39567,#39568,#39569,#39570,#39571,#39572,#39573,
#39574,#39575,#39576,#39577,#39578,#39579,#39580),.UNSPECIFIED.,.F.,.F.)
B_SPLINE_CURVE_WITH_KNOTS((6,1,1,1,1,1,1,1,1,1,1,1,1,1,1,1,1,1,1,1,1,1,
1,1,1,1,1,1,1,1,1,1,1,1,1,1,1,1,1,1,1,1,1,1,1,1,1,1,1,1,1,1,1,1,1,1,1,1,
1,1,1,1,1,1,1,6),(0.00577184337452306,0.0153846153846154,0.0307692307692308,
0.0461538461538462,0.0615384615384615,0.0769230769230769,0.0923076923076923,
0.107692307692308,0.123076923076923,0.138461538461538,0.153846153846154,
0.169230769230769,0.184615384615385,0.2,0.215384615384615,0.230769230769231,
0.246153846153846,0.261538461538462,0.276923076923077,0.292307692307692,
0.307692307692308,0.323076923076923,0.338461538461538,0.353846153846154,
0.369230769230769,0.384615384615385,0.4,0.415384615384615,0.430769230769231,
0.446153846153846,0.461538461538462,0.476923076923077,0.492307692307692,
0.507692307692308,0.523076923076923,0.538461538461538,0.553846153846154,
0.569230769230769,0.584615384615384,0.6,0.615384615384615,0.63076923076923,
0.646153846153846,0.661538461538461,0.676923076923076,0.692307692307692,
0.707692307692307,0.723076923076922,0.738461538461538,0.753846153846153,
0.769230769230768,0.784615384615384,0.799999999999999,0.815384615384614,
0.83076923076923,0.846153846153845,0.86153846153846,0.876923076923076,0.892307692307691,
0.907692307692306,0.923076923076922,0.938461538461537,0.953846153846152,
0.969230769230768,0.984615384615383,1.),.UNSPECIFIED.)
CURVE()
GEOMETRIC_REPRESENTATION_ITEM()
RATIONAL_B_SPLINE_CURVE((1.,1.,1.,1.,1.,1.,1.,1.,1.,1.,1.,1.,1.,1.,1.,1.,
1.,1.,1.,1.,1.,1.,1.,1.,1.,1.,1.,1.,1.,1.,1.,1.,1.,1.,1.,1.,1.,1.,1.,1.,
1.,1.,1.,1.,1.,1.,1.,1.,1.,1.,1.,1.,1.,1.,1.,1.,1.,1.,1.,1.,1.,1.,1.,1.,
1.,1.,1.,1.,1.,1.))
REPRESENTATION_ITEM('')
);
#222=(
BOUNDED_CURVE()
B_SPLINE_CURVE(5,(#39584,#39585,#39586,#39587,#39588,#39589,#39590,#39591,
#39592,#39593,#39594,#39595,#39596,#39597,#39598,#39599,#39600,#39601,#39602,
#39603,#39604,#39605,#39606,#39607,#39608,#39609,#39610,#39611,#39612,#39613,
#39614,#39615,#39616,#39617,#39618,#39619,#39620,#39621,#39622,#39623,#39624,
#39625,#39626,#39627,#39628,#39629,#39630,#39631,#39632,#39633,#39634,#39635,
#39636,#39637,#39638,#39639,#39640,#39641,#39642,#39643,#39644,#39645,#39646,
#39647,#39648,#39649,#39650,#39651,#39652,#39653),.UNSPECIFIED.,.F.,.F.)
B_SPLINE_CURVE_WITH_KNOTS((6,1,1,1,1,1,1,1,1,1,1,1,1,1,1,1,1,1,1,1,1,1,
1,1,1,1,1,1,1,1,1,1,1,1,1,1,1,1,1,1,1,1,1,1,1,1,1,1,1,1,1,1,1,1,1,1,1,1,
1,1,1,1,1,1,1,6),(0.,0.0153846153846154,0.0307692307692308,0.0461538461538462,
0.0615384615384615,0.0769230769230769,0.0923076923076923,0.107692307692308,
0.123076923076923,0.138461538461538,0.153846153846154,0.169230769230769,
0.184615384615385,0.2,0.215384615384615,0.230769230769231,0.246153846153846,
0.261538461538462,0.276923076923077,0.292307692307692,0.307692307692308,
0.323076923076923,0.338461538461538,0.353846153846154,0.369230769230769,
0.384615384615385,0.4,0.415384615384615,0.430769230769231,0.446153846153846,
0.461538461538462,0.476923076923077,0.492307692307692,0.507692307692308,
0.523076923076923,0.538461538461538,0.553846153846154,0.569230769230769,
0.584615384615384,0.6,0.615384615384615,0.63076923076923,0.646153846153846,
0.661538461538461,0.676923076923076,0.692307692307692,0.707692307692307,
0.723076923076922,0.738461538461538,0.753846153846153,0.769230769230768,
0.784615384615384,0.799999999999999,0.815384615384614,0.83076923076923,
0.846153846153845,0.86153846153846,0.876923076923076,0.892307692307691,
0.907692307692306,0.923076923076922,0.938461538461537,0.953846153846152,
0.969230769230768,0.984615384615383,0.994228156739688),.UNSPECIFIED.)
CURVE()
GEOMETRIC_REPRESENTATION_ITEM()
RATIONAL_B_SPLINE_CURVE((1.,1.,1.,1.,1.,1.,1.,1.,1.,1.,1.,1.,1.,1.,1.,1.,
1.,1.,1.,1.,1.,1.,1.,1.,1.,1.,1.,1.,1.,1.,1.,1.,1.,1.,1.,1.,1.,1.,1.,1.,
1.,1.,1.,1.,1.,1.,1.,1.,1.,1.,1.,1.,1.,1.,1.,1.,1.,1.,1.,1.,1.,1.,1.,1.,
1.,1.,1.,1.,1.,1.))
REPRESENTATION_ITEM('')
);
#223=(
BOUNDED_CURVE()
B_SPLINE_CURVE(5,(#39657,#39658,#39659,#39660,#39661,#39662,#39663,#39664,
#39665,#39666,#39667,#39668,#39669,#39670,#39671,#39672,#39673,#39674,#39675,
#39676,#39677,#39678,#39679,#39680,#39681,#39682,#39683,#39684,#39685,#39686,
#39687,#39688,#39689,#39690,#39691,#39692,#39693,#39694,#39695,#39696,#39697,
#39698,#39699,#39700,#39701,#39702,#39703,#39704,#39705,#39706,#39707,#39708,
#39709,#39710,#39711,#39712,#39713,#39714,#39715,#39716,#39717,#39718,#39719,
#39720,#39721,#39722,#39723,#39724,#39725,#39726),.UNSPECIFIED.,.F.,.F.)
B_SPLINE_CURVE_WITH_KNOTS((6,1,1,1,1,1,1,1,1,1,1,1,1,1,1,1,1,1,1,1,1,1,
1,1,1,1,1,1,1,1,1,1,1,1,1,1,1,1,1,1,1,1,1,1,1,1,1,1,1,1,1,1,1,1,1,1,1,1,
1,1,1,1,1,1,1,6),(0.00577184337449862,0.0153846153846154,0.0307692307692308,
0.0461538461538462,0.0615384615384615,0.0769230769230769,0.0923076923076923,
0.107692307692308,0.123076923076923,0.138461538461538,0.153846153846154,
0.169230769230769,0.184615384615385,0.2,0.215384615384615,0.230769230769231,
0.246153846153846,0.261538461538462,0.276923076923077,0.292307692307692,
0.307692307692308,0.323076923076923,0.338461538461538,0.353846153846154,
0.369230769230769,0.384615384615385,0.4,0.415384615384615,0.430769230769231,
0.446153846153846,0.461538461538462,0.476923076923077,0.492307692307692,
0.507692307692308,0.523076923076923,0.538461538461538,0.553846153846154,
0.569230769230769,0.584615384615384,0.6,0.615384615384615,0.63076923076923,
0.646153846153846,0.661538461538461,0.676923076923076,0.692307692307692,
0.707692307692307,0.723076923076922,0.738461538461538,0.753846153846153,
0.769230769230768,0.784615384615384,0.799999999999999,0.815384615384614,
0.83076923076923,0.846153846153845,0.86153846153846,0.876923076923076,0.892307692307691,
0.907692307692306,0.923076923076922,0.938461538461537,0.953846153846152,
0.969230769230768,0.984615384615383,1.),.UNSPECIFIED.)
CURVE()
GEOMETRIC_REPRESENTATION_ITEM()
RATIONAL_B_SPLINE_CURVE((1.,1.,1.,1.,1.,1.,1.,1.,1.,1.,1.,1.,1.,1.,1.,1.,
1.,1.,1.,1.,1.,1.,1.,1.,1.,1.,1.,1.,1.,1.,1.,1.,1.,1.,1.,1.,1.,1.,1.,1.,
1.,1.,1.,1.,1.,1.,1.,1.,1.,1.,1.,1.,1.,1.,1.,1.,1.,1.,1.,1.,1.,1.,1.,1.,
1.,1.,1.,1.,1.,1.))
REPRESENTATION_ITEM('')
);
#224=(
BOUNDED_CURVE()
B_SPLINE_CURVE(5,(#39730,#39731,#39732,#39733,#39734,#39735,#39736,#39737,
#39738,#39739,#39740,#39741,#39742,#39743,#39744,#39745,#39746,#39747,#39748,
#39749,#39750,#39751,#39752,#39753,#39754,#39755,#39756,#39757,#39758,#39759,
#39760,#39761,#39762,#39763,#39764,#39765,#39766,#39767,#39768,#39769,#39770,
#39771,#39772,#39773,#39774,#39775,#39776,#39777,#39778,#39779,#39780,#39781,
#39782,#39783,#39784,#39785,#39786,#39787,#39788,#39789,#39790,#39791,#39792,
#39793,#39794,#39795,#39796,#39797,#39798,#39799),.UNSPECIFIED.,.F.,.F.)
B_SPLINE_CURVE_WITH_KNOTS((6,1,1,1,1,1,1,1,1,1,1,1,1,1,1,1,1,1,1,1,1,1,
1,1,1,1,1,1,1,1,1,1,1,1,1,1,1,1,1,1,1,1,1,1,1,1,1,1,1,1,1,1,1,1,1,1,1,1,
1,1,1,1,1,1,1,6),(0.,0.0153846153846154,0.0307692307692308,0.0461538461538462,
0.0615384615384615,0.0769230769230769,0.0923076923076923,0.107692307692308,
0.123076923076923,0.138461538461538,0.153846153846154,0.169230769230769,
0.184615384615385,0.2,0.215384615384615,0.230769230769231,0.246153846153846,
0.261538461538462,0.276923076923077,0.292307692307692,0.307692307692308,
0.323076923076923,0.338461538461538,0.353846153846154,0.369230769230769,
0.384615384615385,0.4,0.415384615384615,0.430769230769231,0.446153846153846,
0.461538461538462,0.476923076923077,0.492307692307692,0.507692307692308,
0.523076923076923,0.538461538461538,0.553846153846154,0.569230769230769,
0.584615384615384,0.6,0.615384615384615,0.63076923076923,0.646153846153846,
0.661538461538461,0.676923076923076,0.692307692307692,0.707692307692307,
0.723076923076922,0.738461538461538,0.753846153846153,0.769230769230768,
0.784615384615384,0.799999999999999,0.815384615384614,0.83076923076923,
0.846153846153845,0.86153846153846,0.876923076923076,0.892307692307691,
0.907692307692306,0.923076923076922,0.938461538461537,0.953846153846152,
0.969230769230768,0.984615384615383,0.994228156739696),.UNSPECIFIED.)
CURVE()
GEOMETRIC_REPRESENTATION_ITEM()
RATIONAL_B_SPLINE_CURVE((1.,1.,1.,1.,1.,1.,1.,1.,1.,1.,1.,1.,1.,1.,1.,1.,
1.,1.,1.,1.,1.,1.,1.,1.,1.,1.,1.,1.,1.,1.,1.,1.,1.,1.,1.,1.,1.,1.,1.,1.,
1.,1.,1.,1.,1.,1.,1.,1.,1.,1.,1.,1.,1.,1.,1.,1.,1.,1.,1.,1.,1.,1.,1.,1.,
1.,1.,1.,1.,1.,1.))
REPRESENTATION_ITEM('')
);
#225=(
BOUNDED_CURVE()
B_SPLINE_CURVE(5,(#39803,#39804,#39805,#39806,#39807,#39808,#39809,#39810,
#39811,#39812,#39813,#39814,#39815,#39816,#39817,#39818,#39819,#39820,#39821,
#39822,#39823,#39824,#39825,#39826,#39827,#39828,#39829,#39830,#39831,#39832,
#39833,#39834,#39835,#39836,#39837,#39838,#39839,#39840,#39841,#39842,#39843,
#39844,#39845,#39846,#39847,#39848,#39849,#39850,#39851,#39852,#39853,#39854,
#39855,#39856,#39857,#39858,#39859,#39860,#39861,#39862,#39863,#39864,#39865,
#39866,#39867,#39868,#39869,#39870,#39871,#39872),.UNSPECIFIED.,.F.,.F.)
B_SPLINE_CURVE_WITH_KNOTS((6,1,1,1,1,1,1,1,1,1,1,1,1,1,1,1,1,1,1,1,1,1,
1,1,1,1,1,1,1,1,1,1,1,1,1,1,1,1,1,1,1,1,1,1,1,1,1,1,1,1,1,1,1,1,1,1,1,1,
1,1,1,1,1,1,1,6),(0.00577184337452068,0.0153846153846154,0.0307692307692308,
0.0461538461538462,0.0615384615384615,0.0769230769230769,0.0923076923076923,
0.107692307692308,0.123076923076923,0.138461538461538,0.153846153846154,
0.169230769230769,0.184615384615385,0.2,0.215384615384615,0.230769230769231,
0.246153846153846,0.261538461538462,0.276923076923077,0.292307692307692,
0.307692307692308,0.323076923076923,0.338461538461538,0.353846153846154,
0.369230769230769,0.384615384615385,0.4,0.415384615384615,0.430769230769231,
0.446153846153846,0.461538461538462,0.476923076923077,0.492307692307692,
0.507692307692308,0.523076923076923,0.538461538461538,0.553846153846154,
0.569230769230769,0.584615384615384,0.6,0.615384615384615,0.63076923076923,
0.646153846153846,0.661538461538461,0.676923076923076,0.692307692307692,
0.707692307692307,0.723076923076922,0.738461538461538,0.753846153846153,
0.769230769230768,0.784615384615384,0.799999999999999,0.815384615384614,
0.83076923076923,0.846153846153845,0.86153846153846,0.876923076923076,0.892307692307691,
0.907692307692306,0.923076923076922,0.938461538461537,0.953846153846152,
0.969230769230768,0.984615384615383,1.),.UNSPECIFIED.)
CURVE()
GEOMETRIC_REPRESENTATION_ITEM()
RATIONAL_B_SPLINE_CURVE((1.,1.,1.,1.,1.,1.,1.,1.,1.,1.,1.,1.,1.,1.,1.,1.,
1.,1.,1.,1.,1.,1.,1.,1.,1.,1.,1.,1.,1.,1.,1.,1.,1.,1.,1.,1.,1.,1.,1.,1.,
1.,1.,1.,1.,1.,1.,1.,1.,1.,1.,1.,1.,1.,1.,1.,1.,1.,1.,1.,1.,1.,1.,1.,1.,
1.,1.,1.,1.,1.,1.))
REPRESENTATION_ITEM('')
);
#226=(
BOUNDED_CURVE()
B_SPLINE_CURVE(5,(#39876,#39877,#39878,#39879,#39880,#39881,#39882,#39883,
#39884,#39885,#39886,#39887,#39888,#39889,#39890,#39891,#39892,#39893,#39894,
#39895,#39896,#39897,#39898,#39899,#39900,#39901,#39902,#39903,#39904,#39905,
#39906,#39907,#39908,#39909,#39910,#39911,#39912,#39913,#39914,#39915,#39916,
#39917,#39918,#39919,#39920,#39921,#39922,#39923,#39924,#39925,#39926,#39927,
#39928,#39929,#39930,#39931,#39932,#39933,#39934,#39935,#39936,#39937,#39938,
#39939,#39940,#39941,#39942,#39943,#39944,#39945),.UNSPECIFIED.,.F.,.F.)
B_SPLINE_CURVE_WITH_KNOTS((6,1,1,1,1,1,1,1,1,1,1,1,1,1,1,1,1,1,1,1,1,1,
1,1,1,1,1,1,1,1,1,1,1,1,1,1,1,1,1,1,1,1,1,1,1,1,1,1,1,1,1,1,1,1,1,1,1,1,
1,1,1,1,1,1,1,6),(0.,0.0153846153846154,0.0307692307692308,0.0461538461538462,
0.0615384615384615,0.0769230769230769,0.0923076923076923,0.107692307692308,
0.123076923076923,0.138461538461538,0.153846153846154,0.169230769230769,
0.184615384615385,0.2,0.215384615384615,0.230769230769231,0.246153846153846,
0.261538461538462,0.276923076923077,0.292307692307692,0.307692307692308,
0.323076923076923,0.338461538461538,0.353846153846154,0.369230769230769,
0.384615384615385,0.4,0.415384615384615,0.430769230769231,0.446153846153846,
0.461538461538462,0.476923076923077,0.492307692307692,0.507692307692308,
0.523076923076923,0.538461538461538,0.553846153846154,0.569230769230769,
0.584615384615384,0.6,0.615384615384615,0.63076923076923,0.646153846153846,
0.661538461538461,0.676923076923076,0.692307692307692,0.707692307692307,
0.723076923076922,0.738461538461538,0.753846153846153,0.769230769230768,
0.784615384615384,0.799999999999999,0.815384615384614,0.83076923076923,
0.846153846153845,0.86153846153846,0.876923076923076,0.892307692307691,
0.907692307692306,0.923076923076922,0.938461538461537,0.953846153846152,
0.969230769230768,0.984615384615383,0.994228156739698),.UNSPECIFIED.)
CURVE()
GEOMETRIC_REPRESENTATION_ITEM()
RATIONAL_B_SPLINE_CURVE((1.,1.,1.,1.,1.,1.,1.,1.,1.,1.,1.,1.,1.,1.,1.,1.,
1.,1.,1.,1.,1.,1.,1.,1.,1.,1.,1.,1.,1.,1.,1.,1.,1.,1.,1.,1.,1.,1.,1.,1.,
1.,1.,1.,1.,1.,1.,1.,1.,1.,1.,1.,1.,1.,1.,1.,1.,1.,1.,1.,1.,1.,1.,1.,1.,
1.,1.,1.,1.,1.,1.))
REPRESENTATION_ITEM('')
);
#227=(
BOUNDED_CURVE()
B_SPLINE_CURVE(5,(#39949,#39950,#39951,#39952,#39953,#39954,#39955,#39956,
#39957,#39958,#39959,#39960,#39961,#39962,#39963,#39964,#39965,#39966,#39967,
#39968,#39969,#39970,#39971,#39972,#39973,#39974,#39975,#39976,#39977,#39978,
#39979,#39980,#39981,#39982,#39983,#39984,#39985,#39986,#39987,#39988,#39989,
#39990,#39991,#39992,#39993,#39994,#39995,#39996,#39997,#39998,#39999,#40000,
#40001,#40002,#40003,#40004,#40005,#40006,#40007,#40008,#40009,#40010,#40011,
#40012,#40013,#40014,#40015,#40016,#40017,#40018),.UNSPECIFIED.,.F.,.F.)
B_SPLINE_CURVE_WITH_KNOTS((6,1,1,1,1,1,1,1,1,1,1,1,1,1,1,1,1,1,1,1,1,1,
1,1,1,1,1,1,1,1,1,1,1,1,1,1,1,1,1,1,1,1,1,1,1,1,1,1,1,1,1,1,1,1,1,1,1,1,
1,1,1,1,1,1,1,6),(0.00577184337451607,0.0153846153846154,0.0307692307692308,
0.0461538461538462,0.0615384615384615,0.0769230769230769,0.0923076923076923,
0.107692307692308,0.123076923076923,0.138461538461538,0.153846153846154,
0.169230769230769,0.184615384615385,0.2,0.215384615384615,0.230769230769231,
0.246153846153846,0.261538461538462,0.276923076923077,0.292307692307692,
0.307692307692308,0.323076923076923,0.338461538461538,0.353846153846154,
0.369230769230769,0.384615384615385,0.4,0.415384615384615,0.430769230769231,
0.446153846153846,0.461538461538462,0.476923076923077,0.492307692307692,
0.507692307692308,0.523076923076923,0.538461538461538,0.553846153846154,
0.569230769230769,0.584615384615384,0.6,0.615384615384615,0.63076923076923,
0.646153846153846,0.661538461538461,0.676923076923076,0.692307692307692,
0.707692307692307,0.723076923076922,0.738461538461538,0.753846153846153,
0.769230769230768,0.784615384615384,0.799999999999999,0.815384615384614,
0.83076923076923,0.846153846153845,0.86153846153846,0.876923076923076,0.892307692307691,
0.907692307692306,0.923076923076922,0.938461538461537,0.953846153846152,
0.969230769230768,0.984615384615383,1.),.UNSPECIFIED.)
CURVE()
GEOMETRIC_REPRESENTATION_ITEM()
RATIONAL_B_SPLINE_CURVE((1.,1.,1.,1.,1.,1.,1.,1.,1.,1.,1.,1.,1.,1.,1.,1.,
1.,1.,1.,1.,1.,1.,1.,1.,1.,1.,1.,1.,1.,1.,1.,1.,1.,1.,1.,1.,1.,1.,1.,1.,
1.,1.,1.,1.,1.,1.,1.,1.,1.,1.,1.,1.,1.,1.,1.,1.,1.,1.,1.,1.,1.,1.,1.,1.,
1.,1.,1.,1.,1.,1.))
REPRESENTATION_ITEM('')
);
#228=(
BOUNDED_CURVE()
B_SPLINE_CURVE(5,(#40022,#40023,#40024,#40025,#40026,#40027,#40028,#40029,
#40030,#40031,#40032,#40033,#40034,#40035,#40036,#40037,#40038,#40039,#40040,
#40041,#40042,#40043,#40044,#40045,#40046,#40047,#40048,#40049,#40050,#40051,
#40052,#40053,#40054,#40055,#40056,#40057,#40058,#40059,#40060,#40061,#40062,
#40063,#40064,#40065,#40066,#40067,#40068,#40069,#40070,#40071,#40072,#40073,
#40074,#40075,#40076,#40077,#40078,#40079,#40080,#40081,#40082,#40083,#40084,
#40085,#40086,#40087,#40088,#40089,#40090,#40091),.UNSPECIFIED.,.F.,.F.)
B_SPLINE_CURVE_WITH_KNOTS((6,1,1,1,1,1,1,1,1,1,1,1,1,1,1,1,1,1,1,1,1,1,
1,1,1,1,1,1,1,1,1,1,1,1,1,1,1,1,1,1,1,1,1,1,1,1,1,1,1,1,1,1,1,1,1,1,1,1,
1,1,1,1,1,1,1,6),(0.,0.0153846153846154,0.0307692307692308,0.0461538461538462,
0.0615384615384615,0.0769230769230769,0.0923076923076923,0.107692307692308,
0.123076923076923,0.138461538461538,0.153846153846154,0.169230769230769,
0.184615384615385,0.2,0.215384615384615,0.230769230769231,0.246153846153846,
0.261538461538462,0.276923076923077,0.292307692307692,0.307692307692308,
0.323076923076923,0.338461538461538,0.353846153846154,0.369230769230769,
0.384615384615385,0.4,0.415384615384615,0.430769230769231,0.446153846153846,
0.461538461538462,0.476923076923077,0.492307692307692,0.507692307692308,
0.523076923076923,0.538461538461538,0.553846153846154,0.569230769230769,
0.584615384615384,0.6,0.615384615384615,0.63076923076923,0.646153846153846,
0.661538461538461,0.676923076923076,0.692307692307692,0.707692307692307,
0.723076923076922,0.738461538461538,0.753846153846153,0.769230769230768,
0.784615384615384,0.799999999999999,0.815384615384614,0.83076923076923,
0.846153846153845,0.86153846153846,0.876923076923076,0.892307692307691,
0.907692307692306,0.923076923076922,0.938461538461537,0.953846153846152,
0.969230769230768,0.984615384615383,0.994228156739704),.UNSPECIFIED.)
CURVE()
GEOMETRIC_REPRESENTATION_ITEM()
RATIONAL_B_SPLINE_CURVE((1.,1.,1.,1.,1.,1.,1.,1.,1.,1.,1.,1.,1.,1.,1.,1.,
1.,1.,1.,1.,1.,1.,1.,1.,1.,1.,1.,1.,1.,1.,1.,1.,1.,1.,1.,1.,1.,1.,1.,1.,
1.,1.,1.,1.,1.,1.,1.,1.,1.,1.,1.,1.,1.,1.,1.,1.,1.,1.,1.,1.,1.,1.,1.,1.,
1.,1.,1.,1.,1.,1.))
REPRESENTATION_ITEM('')
);
#229=(
BOUNDED_CURVE()
B_SPLINE_CURVE(5,(#40095,#40096,#40097,#40098,#40099,#40100,#40101,#40102,
#40103,#40104,#40105,#40106,#40107,#40108,#40109,#40110,#40111,#40112,#40113,
#40114,#40115,#40116,#40117,#40118,#40119,#40120,#40121,#40122,#40123,#40124,
#40125,#40126,#40127,#40128,#40129,#40130,#40131,#40132,#40133,#40134,#40135,
#40136,#40137,#40138,#40139,#40140,#40141,#40142,#40143,#40144,#40145,#40146,
#40147,#40148,#40149,#40150,#40151,#40152,#40153,#40154,#40155,#40156,#40157,
#40158,#40159,#40160,#40161,#40162,#40163,#40164),.UNSPECIFIED.,.F.,.F.)
B_SPLINE_CURVE_WITH_KNOTS((6,1,1,1,1,1,1,1,1,1,1,1,1,1,1,1,1,1,1,1,1,1,
1,1,1,1,1,1,1,1,1,1,1,1,1,1,1,1,1,1,1,1,1,1,1,1,1,1,1,1,1,1,1,1,1,1,1,1,
1,1,1,1,1,1,1,6),(0.00577184337449692,0.0153846153846154,0.0307692307692308,
0.0461538461538462,0.0615384615384615,0.0769230769230769,0.0923076923076923,
0.107692307692308,0.123076923076923,0.138461538461538,0.153846153846154,
0.169230769230769,0.184615384615385,0.2,0.215384615384615,0.230769230769231,
0.246153846153846,0.261538461538462,0.276923076923077,0.292307692307692,
0.307692307692308,0.323076923076923,0.338461538461538,0.353846153846154,
0.369230769230769,0.384615384615385,0.4,0.415384615384615,0.430769230769231,
0.446153846153846,0.461538461538462,0.476923076923077,0.492307692307692,
0.507692307692308,0.523076923076923,0.538461538461538,0.553846153846154,
0.569230769230769,0.584615384615384,0.6,0.615384615384615,0.63076923076923,
0.646153846153846,0.661538461538461,0.676923076923076,0.692307692307692,
0.707692307692307,0.723076923076922,0.738461538461538,0.753846153846153,
0.769230769230768,0.784615384615384,0.799999999999999,0.815384615384614,
0.83076923076923,0.846153846153845,0.86153846153846,0.876923076923076,0.892307692307691,
0.907692307692306,0.923076923076922,0.938461538461537,0.953846153846152,
0.969230769230768,0.984615384615383,1.),.UNSPECIFIED.)
CURVE()
GEOMETRIC_REPRESENTATION_ITEM()
RATIONAL_B_SPLINE_CURVE((1.,1.,1.,1.,1.,1.,1.,1.,1.,1.,1.,1.,1.,1.,1.,1.,
1.,1.,1.,1.,1.,1.,1.,1.,1.,1.,1.,1.,1.,1.,1.,1.,1.,1.,1.,1.,1.,1.,1.,1.,
1.,1.,1.,1.,1.,1.,1.,1.,1.,1.,1.,1.,1.,1.,1.,1.,1.,1.,1.,1.,1.,1.,1.,1.,
1.,1.,1.,1.,1.,1.))
REPRESENTATION_ITEM('')
);
#230=(
BOUNDED_CURVE()
B_SPLINE_CURVE(5,(#40168,#40169,#40170,#40171,#40172,#40173,#40174,#40175,
#40176,#40177,#40178,#40179,#40180,#40181,#40182,#40183,#40184,#40185,#40186,
#40187,#40188,#40189,#40190,#40191,#40192,#40193,#40194,#40195,#40196,#40197,
#40198,#40199,#40200,#40201,#40202,#40203,#40204,#40205,#40206,#40207,#40208,
#40209,#40210,#40211,#40212,#40213,#40214,#40215,#40216,#40217,#40218,#40219,
#40220,#40221,#40222,#40223,#40224,#40225,#40226,#40227,#40228,#40229,#40230,
#40231,#40232,#40233,#40234,#40235,#40236,#40237),.UNSPECIFIED.,.F.,.F.)
B_SPLINE_CURVE_WITH_KNOTS((6,1,1,1,1,1,1,1,1,1,1,1,1,1,1,1,1,1,1,1,1,1,
1,1,1,1,1,1,1,1,1,1,1,1,1,1,1,1,1,1,1,1,1,1,1,1,1,1,1,1,1,1,1,1,1,1,1,1,
1,1,1,1,1,1,1,6),(0.,0.0153846153846154,0.0307692307692308,0.0461538461538462,
0.0615384615384615,0.0769230769230769,0.0923076923076923,0.107692307692308,
0.123076923076923,0.138461538461538,0.153846153846154,0.169230769230769,
0.184615384615385,0.2,0.215384615384615,0.230769230769231,0.246153846153846,
0.261538461538462,0.276923076923077,0.292307692307692,0.307692307692308,
0.323076923076923,0.338461538461538,0.353846153846154,0.369230769230769,
0.384615384615385,0.4,0.415384615384615,0.430769230769231,0.446153846153846,
0.461538461538462,0.476923076923077,0.492307692307692,0.507692307692308,
0.523076923076923,0.538461538461538,0.553846153846154,0.569230769230769,
0.584615384615384,0.6,0.615384615384615,0.63076923076923,0.646153846153846,
0.661538461538461,0.676923076923076,0.692307692307692,0.707692307692307,
0.723076923076922,0.738461538461538,0.753846153846153,0.769230769230768,
0.784615384615384,0.799999999999999,0.815384615384614,0.83076923076923,
0.846153846153845,0.86153846153846,0.876923076923076,0.892307692307691,
0.907692307692306,0.923076923076922,0.938461538461537,0.953846153846152,
0.969230769230768,0.984615384615383,0.994228156739711),.UNSPECIFIED.)
CURVE()
GEOMETRIC_REPRESENTATION_ITEM()
RATIONAL_B_SPLINE_CURVE((1.,1.,1.,1.,1.,1.,1.,1.,1.,1.,1.,1.,1.,1.,1.,1.,
1.,1.,1.,1.,1.,1.,1.,1.,1.,1.,1.,1.,1.,1.,1.,1.,1.,1.,1.,1.,1.,1.,1.,1.,
1.,1.,1.,1.,1.,1.,1.,1.,1.,1.,1.,1.,1.,1.,1.,1.,1.,1.,1.,1.,1.,1.,1.,1.,
1.,1.,1.,1.,1.,1.))
REPRESENTATION_ITEM('')
);
#231=(
BOUNDED_CURVE()
B_SPLINE_CURVE(5,(#40241,#40242,#40243,#40244,#40245,#40246,#40247,#40248,
#40249,#40250,#40251,#40252,#40253,#40254,#40255,#40256,#40257,#40258,#40259,
#40260,#40261,#40262,#40263,#40264,#40265,#40266,#40267,#40268,#40269,#40270,
#40271,#40272,#40273,#40274,#40275,#40276,#40277,#40278,#40279,#40280,#40281,
#40282,#40283,#40284,#40285,#40286,#40287,#40288,#40289,#40290,#40291,#40292,
#40293,#40294,#40295,#40296,#40297,#40298,#40299,#40300,#40301,#40302,#40303,
#40304,#40305,#40306,#40307,#40308,#40309,#40310),.UNSPECIFIED.,.F.,.F.)
B_SPLINE_CURVE_WITH_KNOTS((6,1,1,1,1,1,1,1,1,1,1,1,1,1,1,1,1,1,1,1,1,1,
1,1,1,1,1,1,1,1,1,1,1,1,1,1,1,1,1,1,1,1,1,1,1,1,1,1,1,1,1,1,1,1,1,1,1,1,
1,1,1,1,1,1,1,6),(0.00577184337450058,0.0153846153846154,0.0307692307692308,
0.0461538461538462,0.0615384615384615,0.0769230769230769,0.0923076923076923,
0.107692307692308,0.123076923076923,0.138461538461538,0.153846153846154,
0.169230769230769,0.184615384615385,0.2,0.215384615384615,0.230769230769231,
0.246153846153846,0.261538461538462,0.276923076923077,0.292307692307692,
0.307692307692308,0.323076923076923,0.338461538461538,0.353846153846154,
0.369230769230769,0.384615384615385,0.4,0.415384615384615,0.430769230769231,
0.446153846153846,0.461538461538462,0.476923076923077,0.492307692307692,
0.507692307692308,0.523076923076923,0.538461538461538,0.553846153846154,
0.569230769230769,0.584615384615384,0.6,0.615384615384615,0.63076923076923,
0.646153846153846,0.661538461538461,0.676923076923076,0.692307692307692,
0.707692307692307,0.723076923076922,0.738461538461538,0.753846153846153,
0.769230769230768,0.784615384615384,0.799999999999999,0.815384615384614,
0.83076923076923,0.846153846153845,0.86153846153846,0.876923076923076,0.892307692307691,
0.907692307692306,0.923076923076922,0.938461538461537,0.953846153846152,
0.969230769230768,0.984615384615383,1.),.UNSPECIFIED.)
CURVE()
GEOMETRIC_REPRESENTATION_ITEM()
RATIONAL_B_SPLINE_CURVE((1.,1.,1.,1.,1.,1.,1.,1.,1.,1.,1.,1.,1.,1.,1.,1.,
1.,1.,1.,1.,1.,1.,1.,1.,1.,1.,1.,1.,1.,1.,1.,1.,1.,1.,1.,1.,1.,1.,1.,1.,
1.,1.,1.,1.,1.,1.,1.,1.,1.,1.,1.,1.,1.,1.,1.,1.,1.,1.,1.,1.,1.,1.,1.,1.,
1.,1.,1.,1.,1.,1.))
REPRESENTATION_ITEM('')
);
#232=(
BOUNDED_CURVE()
B_SPLINE_CURVE(5,(#40314,#40315,#40316,#40317,#40318,#40319,#40320,#40321,
#40322,#40323,#40324,#40325,#40326,#40327,#40328,#40329,#40330,#40331,#40332,
#40333,#40334,#40335,#40336,#40337,#40338,#40339,#40340,#40341,#40342,#40343,
#40344,#40345,#40346,#40347,#40348,#40349,#40350,#40351,#40352,#40353,#40354,
#40355,#40356,#40357,#40358,#40359,#40360,#40361,#40362,#40363,#40364,#40365,
#40366,#40367,#40368,#40369,#40370,#40371,#40372,#40373,#40374,#40375,#40376,
#40377,#40378,#40379,#40380,#40381,#40382,#40383),.UNSPECIFIED.,.F.,.F.)
B_SPLINE_CURVE_WITH_KNOTS((6,1,1,1,1,1,1,1,1,1,1,1,1,1,1,1,1,1,1,1,1,1,
1,1,1,1,1,1,1,1,1,1,1,1,1,1,1,1,1,1,1,1,1,1,1,1,1,1,1,1,1,1,1,1,1,1,1,1,
1,1,1,1,1,1,1,6),(0.,0.0153846153846154,0.0307692307692308,0.0461538461538462,
0.0615384615384615,0.0769230769230769,0.0923076923076923,0.107692307692308,
0.123076923076923,0.138461538461538,0.153846153846154,0.169230769230769,
0.184615384615385,0.2,0.215384615384615,0.230769230769231,0.246153846153846,
0.261538461538462,0.276923076923077,0.292307692307692,0.307692307692308,
0.323076923076923,0.338461538461538,0.353846153846154,0.369230769230769,
0.384615384615385,0.4,0.415384615384615,0.430769230769231,0.446153846153846,
0.461538461538462,0.476923076923077,0.492307692307692,0.507692307692308,
0.523076923076923,0.538461538461538,0.553846153846154,0.569230769230769,
0.584615384615384,0.6,0.615384615384615,0.63076923076923,0.646153846153846,
0.661538461538461,0.676923076923076,0.692307692307692,0.707692307692307,
0.723076923076922,0.738461538461538,0.753846153846153,0.769230769230768,
0.784615384615384,0.799999999999999,0.815384615384614,0.83076923076923,
0.846153846153845,0.86153846153846,0.876923076923076,0.892307692307691,
0.907692307692306,0.923076923076922,0.938461538461537,0.953846153846152,
0.969230769230768,0.984615384615383,0.994228156739701),.UNSPECIFIED.)
CURVE()
GEOMETRIC_REPRESENTATION_ITEM()
RATIONAL_B_SPLINE_CURVE((1.,1.,1.,1.,1.,1.,1.,1.,1.,1.,1.,1.,1.,1.,1.,1.,
1.,1.,1.,1.,1.,1.,1.,1.,1.,1.,1.,1.,1.,1.,1.,1.,1.,1.,1.,1.,1.,1.,1.,1.,
1.,1.,1.,1.,1.,1.,1.,1.,1.,1.,1.,1.,1.,1.,1.,1.,1.,1.,1.,1.,1.,1.,1.,1.,
1.,1.,1.,1.,1.,1.))
REPRESENTATION_ITEM('')
);
#233=(
BOUNDED_CURVE()
B_SPLINE_CURVE(5,(#40387,#40388,#40389,#40390,#40391,#40392,#40393,#40394,
#40395,#40396,#40397,#40398,#40399,#40400,#40401,#40402,#40403,#40404,#40405,
#40406,#40407,#40408,#40409,#40410,#40411,#40412,#40413,#40414,#40415,#40416,
#40417,#40418,#40419,#40420,#40421,#40422,#40423,#40424,#40425,#40426,#40427,
#40428,#40429,#40430,#40431,#40432,#40433,#40434,#40435,#40436,#40437,#40438,
#40439,#40440,#40441,#40442,#40443,#40444,#40445,#40446,#40447,#40448,#40449,
#40450,#40451,#40452,#40453,#40454,#40455,#40456),.UNSPECIFIED.,.F.,.F.)
B_SPLINE_CURVE_WITH_KNOTS((6,1,1,1,1,1,1,1,1,1,1,1,1,1,1,1,1,1,1,1,1,1,
1,1,1,1,1,1,1,1,1,1,1,1,1,1,1,1,1,1,1,1,1,1,1,1,1,1,1,1,1,1,1,1,1,1,1,1,
1,1,1,1,1,1,1,6),(0.0057718433745091,0.0153846153846154,0.0307692307692308,
0.0461538461538462,0.0615384615384615,0.0769230769230769,0.0923076923076923,
0.107692307692308,0.123076923076923,0.138461538461538,0.153846153846154,
0.169230769230769,0.184615384615385,0.2,0.215384615384615,0.230769230769231,
0.246153846153846,0.261538461538462,0.276923076923077,0.292307692307692,
0.307692307692308,0.323076923076923,0.338461538461538,0.353846153846154,
0.369230769230769,0.384615384615385,0.4,0.415384615384615,0.430769230769231,
0.446153846153846,0.461538461538462,0.476923076923077,0.492307692307692,
0.507692307692308,0.523076923076923,0.538461538461538,0.553846153846154,
0.569230769230769,0.584615384615384,0.6,0.615384615384615,0.63076923076923,
0.646153846153846,0.661538461538461,0.676923076923076,0.692307692307692,
0.707692307692307,0.723076923076922,0.738461538461538,0.753846153846153,
0.769230769230768,0.784615384615384,0.799999999999999,0.815384615384614,
0.83076923076923,0.846153846153845,0.86153846153846,0.876923076923076,0.892307692307691,
0.907692307692306,0.923076923076922,0.938461538461537,0.953846153846152,
0.969230769230768,0.984615384615383,1.),.UNSPECIFIED.)
CURVE()
GEOMETRIC_REPRESENTATION_ITEM()
RATIONAL_B_SPLINE_CURVE((1.,1.,1.,1.,1.,1.,1.,1.,1.,1.,1.,1.,1.,1.,1.,1.,
1.,1.,1.,1.,1.,1.,1.,1.,1.,1.,1.,1.,1.,1.,1.,1.,1.,1.,1.,1.,1.,1.,1.,1.,
1.,1.,1.,1.,1.,1.,1.,1.,1.,1.,1.,1.,1.,1.,1.,1.,1.,1.,1.,1.,1.,1.,1.,1.,
1.,1.,1.,1.,1.,1.))
REPRESENTATION_ITEM('')
);
#234=(
BOUNDED_CURVE()
B_SPLINE_CURVE(5,(#40460,#40461,#40462,#40463,#40464,#40465,#40466,#40467,
#40468,#40469,#40470,#40471,#40472,#40473,#40474,#40475,#40476,#40477,#40478,
#40479,#40480,#40481,#40482,#40483,#40484,#40485,#40486,#40487,#40488,#40489,
#40490,#40491,#40492,#40493,#40494,#40495,#40496,#40497,#40498,#40499,#40500,
#40501,#40502,#40503,#40504,#40505,#40506,#40507,#40508,#40509,#40510,#40511,
#40512,#40513,#40514,#40515,#40516,#40517,#40518,#40519,#40520,#40521,#40522,
#40523,#40524,#40525,#40526,#40527,#40528,#40529),.UNSPECIFIED.,.F.,.F.)
B_SPLINE_CURVE_WITH_KNOTS((6,1,1,1,1,1,1,1,1,1,1,1,1,1,1,1,1,1,1,1,1,1,
1,1,1,1,1,1,1,1,1,1,1,1,1,1,1,1,1,1,1,1,1,1,1,1,1,1,1,1,1,1,1,1,1,1,1,1,
1,1,1,1,1,1,1,6),(0.,0.0153846153846154,0.0307692307692308,0.0461538461538462,
0.0615384615384615,0.0769230769230769,0.0923076923076923,0.107692307692308,
0.123076923076923,0.138461538461538,0.153846153846154,0.169230769230769,
0.184615384615385,0.2,0.215384615384615,0.230769230769231,0.246153846153846,
0.261538461538462,0.276923076923077,0.292307692307692,0.307692307692308,
0.323076923076923,0.338461538461538,0.353846153846154,0.369230769230769,
0.384615384615385,0.4,0.415384615384615,0.430769230769231,0.446153846153846,
0.461538461538462,0.476923076923077,0.492307692307692,0.507692307692308,
0.523076923076923,0.538461538461538,0.553846153846154,0.569230769230769,
0.584615384615384,0.6,0.615384615384615,0.63076923076923,0.646153846153846,
0.661538461538461,0.676923076923076,0.692307692307692,0.707692307692307,
0.723076923076922,0.738461538461538,0.753846153846153,0.769230769230768,
0.784615384615384,0.799999999999999,0.815384615384614,0.83076923076923,
0.846153846153845,0.86153846153846,0.876923076923076,0.892307692307691,
0.907692307692306,0.923076923076922,0.938461538461537,0.953846153846152,
0.969230769230768,0.984615384615383,0.994228156739689),.UNSPECIFIED.)
CURVE()
GEOMETRIC_REPRESENTATION_ITEM()
RATIONAL_B_SPLINE_CURVE((1.,1.,1.,1.,1.,1.,1.,1.,1.,1.,1.,1.,1.,1.,1.,1.,
1.,1.,1.,1.,1.,1.,1.,1.,1.,1.,1.,1.,1.,1.,1.,1.,1.,1.,1.,1.,1.,1.,1.,1.,
1.,1.,1.,1.,1.,1.,1.,1.,1.,1.,1.,1.,1.,1.,1.,1.,1.,1.,1.,1.,1.,1.,1.,1.,
1.,1.,1.,1.,1.,1.))
REPRESENTATION_ITEM('')
);
#235=(
BOUNDED_CURVE()
B_SPLINE_CURVE(5,(#40533,#40534,#40535,#40536,#40537,#40538,#40539,#40540,
#40541,#40542,#40543,#40544,#40545,#40546,#40547,#40548,#40549,#40550,#40551,
#40552,#40553,#40554,#40555,#40556,#40557,#40558,#40559,#40560,#40561,#40562,
#40563,#40564,#40565,#40566,#40567,#40568,#40569,#40570,#40571,#40572,#40573,
#40574,#40575,#40576,#40577,#40578,#40579,#40580,#40581,#40582,#40583,#40584,
#40585,#40586,#40587,#40588,#40589,#40590,#40591,#40592,#40593,#40594,#40595,
#40596,#40597,#40598,#40599,#40600,#40601,#40602),.UNSPECIFIED.,.F.,.F.)
B_SPLINE_CURVE_WITH_KNOTS((6,1,1,1,1,1,1,1,1,1,1,1,1,1,1,1,1,1,1,1,1,1,
1,1,1,1,1,1,1,1,1,1,1,1,1,1,1,1,1,1,1,1,1,1,1,1,1,1,1,1,1,1,1,1,1,1,1,1,
1,1,1,1,1,1,1,6),(0.00577184337450777,0.0153846153846154,0.0307692307692308,
0.0461538461538462,0.0615384615384615,0.0769230769230769,0.0923076923076923,
0.107692307692308,0.123076923076923,0.138461538461538,0.153846153846154,
0.169230769230769,0.184615384615385,0.2,0.215384615384615,0.230769230769231,
0.246153846153846,0.261538461538462,0.276923076923077,0.292307692307692,
0.307692307692308,0.323076923076923,0.338461538461538,0.353846153846154,
0.369230769230769,0.384615384615385,0.4,0.415384615384615,0.430769230769231,
0.446153846153846,0.461538461538462,0.476923076923077,0.492307692307692,
0.507692307692308,0.523076923076923,0.538461538461538,0.553846153846154,
0.569230769230769,0.584615384615384,0.6,0.615384615384615,0.63076923076923,
0.646153846153846,0.661538461538461,0.676923076923076,0.692307692307692,
0.707692307692307,0.723076923076922,0.738461538461538,0.753846153846153,
0.769230769230768,0.784615384615384,0.799999999999999,0.815384615384614,
0.83076923076923,0.846153846153845,0.86153846153846,0.876923076923076,0.892307692307691,
0.907692307692306,0.923076923076922,0.938461538461537,0.953846153846152,
0.969230769230768,0.984615384615383,1.),.UNSPECIFIED.)
CURVE()
GEOMETRIC_REPRESENTATION_ITEM()
RATIONAL_B_SPLINE_CURVE((1.,1.,1.,1.,1.,1.,1.,1.,1.,1.,1.,1.,1.,1.,1.,1.,
1.,1.,1.,1.,1.,1.,1.,1.,1.,1.,1.,1.,1.,1.,1.,1.,1.,1.,1.,1.,1.,1.,1.,1.,
1.,1.,1.,1.,1.,1.,1.,1.,1.,1.,1.,1.,1.,1.,1.,1.,1.,1.,1.,1.,1.,1.,1.,1.,
1.,1.,1.,1.,1.,1.))
REPRESENTATION_ITEM('')
);
#236=(
BOUNDED_CURVE()
B_SPLINE_CURVE(5,(#40606,#40607,#40608,#40609,#40610,#40611,#40612,#40613,
#40614,#40615,#40616,#40617,#40618,#40619,#40620,#40621,#40622,#40623,#40624,
#40625,#40626,#40627,#40628,#40629,#40630,#40631,#40632,#40633,#40634,#40635,
#40636,#40637,#40638,#40639,#40640,#40641,#40642,#40643,#40644,#40645,#40646,
#40647,#40648,#40649,#40650,#40651,#40652,#40653,#40654,#40655,#40656,#40657,
#40658,#40659,#40660,#40661,#40662,#40663,#40664,#40665,#40666,#40667,#40668,
#40669,#40670,#40671,#40672,#40673,#40674,#40675),.UNSPECIFIED.,.F.,.F.)
B_SPLINE_CURVE_WITH_KNOTS((6,1,1,1,1,1,1,1,1,1,1,1,1,1,1,1,1,1,1,1,1,1,
1,1,1,1,1,1,1,1,1,1,1,1,1,1,1,1,1,1,1,1,1,1,1,1,1,1,1,1,1,1,1,1,1,1,1,1,
1,1,1,1,1,1,1,6),(0.,0.0153846153846154,0.0307692307692308,0.0461538461538462,
0.0615384615384615,0.0769230769230769,0.0923076923076923,0.107692307692308,
0.123076923076923,0.138461538461538,0.153846153846154,0.169230769230769,
0.184615384615385,0.2,0.215384615384615,0.230769230769231,0.246153846153846,
0.261538461538462,0.276923076923077,0.292307692307692,0.307692307692308,
0.323076923076923,0.338461538461538,0.353846153846154,0.369230769230769,
0.384615384615385,0.4,0.415384615384615,0.430769230769231,0.446153846153846,
0.461538461538462,0.476923076923077,0.492307692307692,0.507692307692308,
0.523076923076923,0.538461538461538,0.553846153846154,0.569230769230769,
0.584615384615384,0.6,0.615384615384615,0.63076923076923,0.646153846153846,
0.661538461538461,0.676923076923076,0.692307692307692,0.707692307692307,
0.723076923076922,0.738461538461538,0.753846153846153,0.769230769230768,
0.784615384615384,0.799999999999999,0.815384615384614,0.83076923076923,
0.846153846153845,0.86153846153846,0.876923076923076,0.892307692307691,
0.907692307692306,0.923076923076922,0.938461538461537,0.953846153846152,
0.969230769230768,0.984615384615383,0.994228156739701),.UNSPECIFIED.)
CURVE()
GEOMETRIC_REPRESENTATION_ITEM()
RATIONAL_B_SPLINE_CURVE((1.,1.,1.,1.,1.,1.,1.,1.,1.,1.,1.,1.,1.,1.,1.,1.,
1.,1.,1.,1.,1.,1.,1.,1.,1.,1.,1.,1.,1.,1.,1.,1.,1.,1.,1.,1.,1.,1.,1.,1.,
1.,1.,1.,1.,1.,1.,1.,1.,1.,1.,1.,1.,1.,1.,1.,1.,1.,1.,1.,1.,1.,1.,1.,1.,
1.,1.,1.,1.,1.,1.))
REPRESENTATION_ITEM('')
);
#237=(
BOUNDED_CURVE()
B_SPLINE_CURVE(5,(#40679,#40680,#40681,#40682,#40683,#40684,#40685,#40686,
#40687,#40688,#40689,#40690,#40691,#40692,#40693,#40694,#40695,#40696,#40697,
#40698,#40699,#40700,#40701,#40702,#40703,#40704,#40705,#40706,#40707,#40708,
#40709,#40710,#40711,#40712,#40713,#40714,#40715,#40716,#40717,#40718,#40719,
#40720,#40721,#40722,#40723,#40724,#40725,#40726,#40727,#40728,#40729,#40730,
#40731,#40732,#40733,#40734,#40735,#40736,#40737,#40738,#40739,#40740,#40741,
#40742,#40743,#40744,#40745,#40746,#40747,#40748),.UNSPECIFIED.,.F.,.F.)
B_SPLINE_CURVE_WITH_KNOTS((6,1,1,1,1,1,1,1,1,1,1,1,1,1,1,1,1,1,1,1,1,1,
1,1,1,1,1,1,1,1,1,1,1,1,1,1,1,1,1,1,1,1,1,1,1,1,1,1,1,1,1,1,1,1,1,1,1,1,
1,1,1,1,1,1,1,6),(0.00577184337450172,0.0153846153846154,0.0307692307692308,
0.0461538461538462,0.0615384615384615,0.0769230769230769,0.0923076923076923,
0.107692307692308,0.123076923076923,0.138461538461538,0.153846153846154,
0.169230769230769,0.184615384615385,0.2,0.215384615384615,0.230769230769231,
0.246153846153846,0.261538461538462,0.276923076923077,0.292307692307692,
0.307692307692308,0.323076923076923,0.338461538461538,0.353846153846154,
0.369230769230769,0.384615384615385,0.4,0.415384615384615,0.430769230769231,
0.446153846153846,0.461538461538462,0.476923076923077,0.492307692307692,
0.507692307692308,0.523076923076923,0.538461538461538,0.553846153846154,
0.569230769230769,0.584615384615384,0.6,0.615384615384615,0.63076923076923,
0.646153846153846,0.661538461538461,0.676923076923076,0.692307692307692,
0.707692307692307,0.723076923076922,0.738461538461538,0.753846153846153,
0.769230769230768,0.784615384615384,0.799999999999999,0.815384615384614,
0.83076923076923,0.846153846153845,0.86153846153846,0.876923076923076,0.892307692307691,
0.907692307692306,0.923076923076922,0.938461538461537,0.953846153846152,
0.969230769230768,0.984615384615383,1.),.UNSPECIFIED.)
CURVE()
GEOMETRIC_REPRESENTATION_ITEM()
RATIONAL_B_SPLINE_CURVE((1.,1.,1.,1.,1.,1.,1.,1.,1.,1.,1.,1.,1.,1.,1.,1.,
1.,1.,1.,1.,1.,1.,1.,1.,1.,1.,1.,1.,1.,1.,1.,1.,1.,1.,1.,1.,1.,1.,1.,1.,
1.,1.,1.,1.,1.,1.,1.,1.,1.,1.,1.,1.,1.,1.,1.,1.,1.,1.,1.,1.,1.,1.,1.,1.,
1.,1.,1.,1.,1.,1.))
REPRESENTATION_ITEM('')
);
#238=(
BOUNDED_CURVE()
B_SPLINE_CURVE(5,(#40752,#40753,#40754,#40755,#40756,#40757,#40758,#40759,
#40760,#40761,#40762,#40763,#40764,#40765,#40766,#40767,#40768,#40769,#40770,
#40771,#40772,#40773,#40774,#40775,#40776,#40777,#40778,#40779,#40780,#40781,
#40782,#40783,#40784,#40785,#40786,#40787,#40788,#40789,#40790,#40791,#40792,
#40793,#40794,#40795,#40796,#40797,#40798,#40799,#40800,#40801,#40802,#40803,
#40804,#40805,#40806,#40807,#40808,#40809,#40810,#40811,#40812,#40813,#40814,
#40815,#40816,#40817,#40818,#40819,#40820,#40821),.UNSPECIFIED.,.F.,.F.)
B_SPLINE_CURVE_WITH_KNOTS((6,1,1,1,1,1,1,1,1,1,1,1,1,1,1,1,1,1,1,1,1,1,
1,1,1,1,1,1,1,1,1,1,1,1,1,1,1,1,1,1,1,1,1,1,1,1,1,1,1,1,1,1,1,1,1,1,1,1,
1,1,1,1,1,1,1,6),(0.,0.0153846153846154,0.0307692307692308,0.0461538461538462,
0.0615384615384615,0.0769230769230769,0.0923076923076923,0.107692307692308,
0.123076923076923,0.138461538461538,0.153846153846154,0.169230769230769,
0.184615384615385,0.2,0.215384615384615,0.230769230769231,0.246153846153846,
0.261538461538462,0.276923076923077,0.292307692307692,0.307692307692308,
0.323076923076923,0.338461538461538,0.353846153846154,0.369230769230769,
0.384615384615385,0.4,0.415384615384615,0.430769230769231,0.446153846153846,
0.461538461538462,0.476923076923077,0.492307692307692,0.507692307692308,
0.523076923076923,0.538461538461538,0.553846153846154,0.569230769230769,
0.584615384615384,0.6,0.615384615384615,0.63076923076923,0.646153846153846,
0.661538461538461,0.676923076923076,0.692307692307692,0.707692307692307,
0.723076923076922,0.738461538461538,0.753846153846153,0.769230769230768,
0.784615384615384,0.799999999999999,0.815384615384614,0.83076923076923,
0.846153846153845,0.86153846153846,0.876923076923076,0.892307692307691,
0.907692307692306,0.923076923076922,0.938461538461537,0.953846153846152,
0.969230769230768,0.984615384615383,0.99422815673971),.UNSPECIFIED.)
CURVE()
GEOMETRIC_REPRESENTATION_ITEM()
RATIONAL_B_SPLINE_CURVE((1.,1.,1.,1.,1.,1.,1.,1.,1.,1.,1.,1.,1.,1.,1.,1.,
1.,1.,1.,1.,1.,1.,1.,1.,1.,1.,1.,1.,1.,1.,1.,1.,1.,1.,1.,1.,1.,1.,1.,1.,
1.,1.,1.,1.,1.,1.,1.,1.,1.,1.,1.,1.,1.,1.,1.,1.,1.,1.,1.,1.,1.,1.,1.,1.,
1.,1.,1.,1.,1.,1.))
REPRESENTATION_ITEM('')
);
#239=(
BOUNDED_CURVE()
B_SPLINE_CURVE(5,(#40825,#40826,#40827,#40828,#40829,#40830,#40831,#40832,
#40833,#40834,#40835,#40836,#40837,#40838,#40839,#40840,#40841,#40842,#40843,
#40844,#40845,#40846,#40847,#40848,#40849,#40850,#40851,#40852,#40853,#40854,
#40855,#40856,#40857,#40858,#40859,#40860,#40861,#40862,#40863,#40864,#40865,
#40866,#40867,#40868,#40869,#40870,#40871,#40872,#40873,#40874,#40875,#40876,
#40877,#40878,#40879,#40880,#40881,#40882,#40883,#40884,#40885,#40886,#40887,
#40888,#40889,#40890,#40891,#40892,#40893,#40894),.UNSPECIFIED.,.F.,.F.)
B_SPLINE_CURVE_WITH_KNOTS((6,1,1,1,1,1,1,1,1,1,1,1,1,1,1,1,1,1,1,1,1,1,
1,1,1,1,1,1,1,1,1,1,1,1,1,1,1,1,1,1,1,1,1,1,1,1,1,1,1,1,1,1,1,1,1,1,1,1,
1,1,1,1,1,1,1,6),(0.00577184337448657,0.0153846153846154,0.0307692307692308,
0.0461538461538462,0.0615384615384615,0.0769230769230769,0.0923076923076923,
0.107692307692308,0.123076923076923,0.138461538461538,0.153846153846154,
0.169230769230769,0.184615384615385,0.2,0.215384615384615,0.230769230769231,
0.246153846153846,0.261538461538462,0.276923076923077,0.292307692307692,
0.307692307692308,0.323076923076923,0.338461538461538,0.353846153846154,
0.369230769230769,0.384615384615385,0.4,0.415384615384615,0.430769230769231,
0.446153846153846,0.461538461538462,0.476923076923077,0.492307692307692,
0.507692307692308,0.523076923076923,0.538461538461538,0.553846153846154,
0.569230769230769,0.584615384615384,0.6,0.615384615384615,0.63076923076923,
0.646153846153846,0.661538461538461,0.676923076923076,0.692307692307692,
0.707692307692307,0.723076923076922,0.738461538461538,0.753846153846153,
0.769230769230768,0.784615384615384,0.799999999999999,0.815384615384614,
0.83076923076923,0.846153846153845,0.86153846153846,0.876923076923076,0.892307692307691,
0.907692307692306,0.923076923076922,0.938461538461537,0.953846153846152,
0.969230769230768,0.984615384615383,1.),.UNSPECIFIED.)
CURVE()
GEOMETRIC_REPRESENTATION_ITEM()
RATIONAL_B_SPLINE_CURVE((1.,1.,1.,1.,1.,1.,1.,1.,1.,1.,1.,1.,1.,1.,1.,1.,
1.,1.,1.,1.,1.,1.,1.,1.,1.,1.,1.,1.,1.,1.,1.,1.,1.,1.,1.,1.,1.,1.,1.,1.,
1.,1.,1.,1.,1.,1.,1.,1.,1.,1.,1.,1.,1.,1.,1.,1.,1.,1.,1.,1.,1.,1.,1.,1.,
1.,1.,1.,1.,1.,1.))
REPRESENTATION_ITEM('')
);
#240=(
BOUNDED_CURVE()
B_SPLINE_CURVE(5,(#40898,#40899,#40900,#40901,#40902,#40903,#40904,#40905,
#40906,#40907,#40908,#40909,#40910,#40911,#40912,#40913,#40914,#40915,#40916,
#40917,#40918,#40919,#40920,#40921,#40922,#40923,#40924,#40925,#40926,#40927,
#40928,#40929,#40930,#40931,#40932,#40933,#40934,#40935,#40936,#40937,#40938,
#40939,#40940,#40941,#40942,#40943,#40944,#40945,#40946,#40947,#40948,#40949,
#40950,#40951,#40952,#40953,#40954,#40955,#40956,#40957,#40958,#40959,#40960,
#40961,#40962,#40963,#40964,#40965,#40966,#40967),.UNSPECIFIED.,.F.,.F.)
B_SPLINE_CURVE_WITH_KNOTS((6,1,1,1,1,1,1,1,1,1,1,1,1,1,1,1,1,1,1,1,1,1,
1,1,1,1,1,1,1,1,1,1,1,1,1,1,1,1,1,1,1,1,1,1,1,1,1,1,1,1,1,1,1,1,1,1,1,1,
1,1,1,1,1,1,1,6),(0.,0.0153846153846154,0.0307692307692308,0.0461538461538462,
0.0615384615384615,0.0769230769230769,0.0923076923076923,0.107692307692308,
0.123076923076923,0.138461538461538,0.153846153846154,0.169230769230769,
0.184615384615385,0.2,0.215384615384615,0.230769230769231,0.246153846153846,
0.261538461538462,0.276923076923077,0.292307692307692,0.307692307692308,
0.323076923076923,0.338461538461538,0.353846153846154,0.369230769230769,
0.384615384615385,0.4,0.415384615384615,0.430769230769231,0.446153846153846,
0.461538461538462,0.476923076923077,0.492307692307692,0.507692307692308,
0.523076923076923,0.538461538461538,0.553846153846154,0.569230769230769,
0.584615384615384,0.6,0.615384615384615,0.63076923076923,0.646153846153846,
0.661538461538461,0.676923076923076,0.692307692307692,0.707692307692307,
0.723076923076922,0.738461538461538,0.753846153846153,0.769230769230768,
0.784615384615384,0.799999999999999,0.815384615384614,0.83076923076923,
0.846153846153845,0.86153846153846,0.876923076923076,0.892307692307691,
0.907692307692306,0.923076923076922,0.938461538461537,0.953846153846152,
0.969230769230768,0.984615384615383,0.994228156739709),.UNSPECIFIED.)
CURVE()
GEOMETRIC_REPRESENTATION_ITEM()
RATIONAL_B_SPLINE_CURVE((1.,1.,1.,1.,1.,1.,1.,1.,1.,1.,1.,1.,1.,1.,1.,1.,
1.,1.,1.,1.,1.,1.,1.,1.,1.,1.,1.,1.,1.,1.,1.,1.,1.,1.,1.,1.,1.,1.,1.,1.,
1.,1.,1.,1.,1.,1.,1.,1.,1.,1.,1.,1.,1.,1.,1.,1.,1.,1.,1.,1.,1.,1.,1.,1.,
1.,1.,1.,1.,1.,1.))
REPRESENTATION_ITEM('')
);
#241=(
BOUNDED_CURVE()
B_SPLINE_CURVE(5,(#40971,#40972,#40973,#40974,#40975,#40976,#40977,#40978,
#40979,#40980,#40981,#40982,#40983,#40984,#40985,#40986,#40987,#40988,#40989,
#40990,#40991,#40992,#40993,#40994,#40995,#40996,#40997,#40998,#40999,#41000,
#41001,#41002,#41003,#41004,#41005,#41006,#41007,#41008,#41009,#41010,#41011,
#41012,#41013,#41014,#41015,#41016,#41017,#41018,#41019,#41020,#41021,#41022,
#41023,#41024,#41025,#41026,#41027,#41028,#41029,#41030,#41031,#41032,#41033,
#41034,#41035,#41036,#41037,#41038,#41039,#41040),.UNSPECIFIED.,.F.,.F.)
B_SPLINE_CURVE_WITH_KNOTS((6,1,1,1,1,1,1,1,1,1,1,1,1,1,1,1,1,1,1,1,1,1,
1,1,1,1,1,1,1,1,1,1,1,1,1,1,1,1,1,1,1,1,1,1,1,1,1,1,1,1,1,1,1,1,1,1,1,1,
1,1,1,1,1,1,1,6),(0.00577184337451094,0.0153846153846154,0.0307692307692308,
0.0461538461538462,0.0615384615384615,0.0769230769230769,0.0923076923076923,
0.107692307692308,0.123076923076923,0.138461538461538,0.153846153846154,
0.169230769230769,0.184615384615385,0.2,0.215384615384615,0.230769230769231,
0.246153846153846,0.261538461538462,0.276923076923077,0.292307692307692,
0.307692307692308,0.323076923076923,0.338461538461538,0.353846153846154,
0.369230769230769,0.384615384615385,0.4,0.415384615384615,0.430769230769231,
0.446153846153846,0.461538461538462,0.476923076923077,0.492307692307692,
0.507692307692308,0.523076923076923,0.538461538461538,0.553846153846154,
0.569230769230769,0.584615384615384,0.6,0.615384615384615,0.63076923076923,
0.646153846153846,0.661538461538461,0.676923076923076,0.692307692307692,
0.707692307692307,0.723076923076922,0.738461538461538,0.753846153846153,
0.769230769230768,0.784615384615384,0.799999999999999,0.815384615384614,
0.83076923076923,0.846153846153845,0.86153846153846,0.876923076923076,0.892307692307691,
0.907692307692306,0.923076923076922,0.938461538461537,0.953846153846152,
0.969230769230768,0.984615384615383,1.),.UNSPECIFIED.)
CURVE()
GEOMETRIC_REPRESENTATION_ITEM()
RATIONAL_B_SPLINE_CURVE((1.,1.,1.,1.,1.,1.,1.,1.,1.,1.,1.,1.,1.,1.,1.,1.,
1.,1.,1.,1.,1.,1.,1.,1.,1.,1.,1.,1.,1.,1.,1.,1.,1.,1.,1.,1.,1.,1.,1.,1.,
1.,1.,1.,1.,1.,1.,1.,1.,1.,1.,1.,1.,1.,1.,1.,1.,1.,1.,1.,1.,1.,1.,1.,1.,
1.,1.,1.,1.,1.,1.))
REPRESENTATION_ITEM('')
);
#242=(
BOUNDED_CURVE()
B_SPLINE_CURVE(5,(#41044,#41045,#41046,#41047,#41048,#41049,#41050,#41051,
#41052,#41053,#41054,#41055,#41056,#41057,#41058,#41059,#41060,#41061,#41062,
#41063,#41064,#41065,#41066,#41067,#41068,#41069,#41070,#41071,#41072,#41073,
#41074,#41075,#41076,#41077,#41078,#41079,#41080,#41081,#41082,#41083,#41084,
#41085,#41086,#41087,#41088,#41089,#41090,#41091,#41092,#41093,#41094,#41095,
#41096,#41097,#41098,#41099,#41100,#41101,#41102,#41103,#41104,#41105,#41106,
#41107,#41108,#41109,#41110,#41111,#41112,#41113),.UNSPECIFIED.,.F.,.F.)
B_SPLINE_CURVE_WITH_KNOTS((6,1,1,1,1,1,1,1,1,1,1,1,1,1,1,1,1,1,1,1,1,1,
1,1,1,1,1,1,1,1,1,1,1,1,1,1,1,1,1,1,1,1,1,1,1,1,1,1,1,1,1,1,1,1,1,1,1,1,
1,1,1,1,1,1,1,6),(0.,0.0153846153846154,0.0307692307692308,0.0461538461538462,
0.0615384615384615,0.0769230769230769,0.0923076923076923,0.107692307692308,
0.123076923076923,0.138461538461538,0.153846153846154,0.169230769230769,
0.184615384615385,0.2,0.215384615384615,0.230769230769231,0.246153846153846,
0.261538461538462,0.276923076923077,0.292307692307692,0.307692307692308,
0.323076923076923,0.338461538461538,0.353846153846154,0.369230769230769,
0.384615384615385,0.4,0.415384615384615,0.430769230769231,0.446153846153846,
0.461538461538462,0.476923076923077,0.492307692307692,0.507692307692308,
0.523076923076923,0.538461538461538,0.553846153846154,0.569230769230769,
0.584615384615384,0.6,0.615384615384615,0.63076923076923,0.646153846153846,
0.661538461538461,0.676923076923076,0.692307692307692,0.707692307692307,
0.723076923076922,0.738461538461538,0.753846153846153,0.769230769230768,
0.784615384615384,0.799999999999999,0.815384615384614,0.83076923076923,
0.846153846153845,0.86153846153846,0.876923076923076,0.892307692307691,
0.907692307692306,0.923076923076922,0.938461538461537,0.953846153846152,
0.969230769230768,0.984615384615383,0.994228156739701),.UNSPECIFIED.)
CURVE()
GEOMETRIC_REPRESENTATION_ITEM()
RATIONAL_B_SPLINE_CURVE((1.,1.,1.,1.,1.,1.,1.,1.,1.,1.,1.,1.,1.,1.,1.,1.,
1.,1.,1.,1.,1.,1.,1.,1.,1.,1.,1.,1.,1.,1.,1.,1.,1.,1.,1.,1.,1.,1.,1.,1.,
1.,1.,1.,1.,1.,1.,1.,1.,1.,1.,1.,1.,1.,1.,1.,1.,1.,1.,1.,1.,1.,1.,1.,1.,
1.,1.,1.,1.,1.,1.))
REPRESENTATION_ITEM('')
);
#243=(
BOUNDED_CURVE()
B_SPLINE_CURVE(5,(#41117,#41118,#41119,#41120,#41121,#41122,#41123,#41124,
#41125,#41126,#41127,#41128,#41129,#41130,#41131,#41132,#41133,#41134,#41135,
#41136,#41137,#41138,#41139,#41140,#41141,#41142,#41143,#41144,#41145,#41146,
#41147,#41148,#41149,#41150,#41151,#41152,#41153,#41154,#41155,#41156,#41157,
#41158,#41159,#41160,#41161,#41162,#41163,#41164,#41165,#41166,#41167,#41168,
#41169,#41170,#41171,#41172,#41173,#41174,#41175,#41176,#41177,#41178,#41179,
#41180,#41181,#41182,#41183,#41184,#41185,#41186),.UNSPECIFIED.,.F.,.F.)
B_SPLINE_CURVE_WITH_KNOTS((6,1,1,1,1,1,1,1,1,1,1,1,1,1,1,1,1,1,1,1,1,1,
1,1,1,1,1,1,1,1,1,1,1,1,1,1,1,1,1,1,1,1,1,1,1,1,1,1,1,1,1,1,1,1,1,1,1,1,
1,1,1,1,1,1,1,6),(0.0057718433745102,0.0153846153846154,0.0307692307692308,
0.0461538461538462,0.0615384615384615,0.0769230769230769,0.0923076923076923,
0.107692307692308,0.123076923076923,0.138461538461538,0.153846153846154,
0.169230769230769,0.184615384615385,0.2,0.215384615384615,0.230769230769231,
0.246153846153846,0.261538461538462,0.276923076923077,0.292307692307692,
0.307692307692308,0.323076923076923,0.338461538461538,0.353846153846154,
0.369230769230769,0.384615384615385,0.4,0.415384615384615,0.430769230769231,
0.446153846153846,0.461538461538462,0.476923076923077,0.492307692307692,
0.507692307692308,0.523076923076923,0.538461538461538,0.553846153846154,
0.569230769230769,0.584615384615384,0.6,0.615384615384615,0.63076923076923,
0.646153846153846,0.661538461538461,0.676923076923076,0.692307692307692,
0.707692307692307,0.723076923076922,0.738461538461538,0.753846153846153,
0.769230769230768,0.784615384615384,0.799999999999999,0.815384615384614,
0.83076923076923,0.846153846153845,0.86153846153846,0.876923076923076,0.892307692307691,
0.907692307692306,0.923076923076922,0.938461538461537,0.953846153846152,
0.969230769230768,0.984615384615383,1.),.UNSPECIFIED.)
CURVE()
GEOMETRIC_REPRESENTATION_ITEM()
RATIONAL_B_SPLINE_CURVE((1.,1.,1.,1.,1.,1.,1.,1.,1.,1.,1.,1.,1.,1.,1.,1.,
1.,1.,1.,1.,1.,1.,1.,1.,1.,1.,1.,1.,1.,1.,1.,1.,1.,1.,1.,1.,1.,1.,1.,1.,
1.,1.,1.,1.,1.,1.,1.,1.,1.,1.,1.,1.,1.,1.,1.,1.,1.,1.,1.,1.,1.,1.,1.,1.,
1.,1.,1.,1.,1.,1.))
REPRESENTATION_ITEM('')
);
#244=(
BOUNDED_CURVE()
B_SPLINE_CURVE(5,(#41190,#41191,#41192,#41193,#41194,#41195,#41196,#41197,
#41198,#41199,#41200,#41201,#41202,#41203,#41204,#41205,#41206,#41207,#41208,
#41209,#41210,#41211,#41212,#41213,#41214,#41215,#41216,#41217,#41218,#41219,
#41220,#41221,#41222,#41223,#41224,#41225,#41226,#41227,#41228,#41229,#41230,
#41231,#41232,#41233,#41234,#41235,#41236,#41237,#41238,#41239,#41240,#41241,
#41242,#41243,#41244,#41245,#41246,#41247,#41248,#41249,#41250,#41251,#41252,
#41253,#41254,#41255,#41256,#41257,#41258,#41259),.UNSPECIFIED.,.F.,.F.)
B_SPLINE_CURVE_WITH_KNOTS((6,1,1,1,1,1,1,1,1,1,1,1,1,1,1,1,1,1,1,1,1,1,
1,1,1,1,1,1,1,1,1,1,1,1,1,1,1,1,1,1,1,1,1,1,1,1,1,1,1,1,1,1,1,1,1,1,1,1,
1,1,1,1,1,1,1,6),(0.,0.0153846153846154,0.0307692307692308,0.0461538461538462,
0.0615384615384615,0.0769230769230769,0.0923076923076923,0.107692307692308,
0.123076923076923,0.138461538461538,0.153846153846154,0.169230769230769,
0.184615384615385,0.2,0.215384615384615,0.230769230769231,0.246153846153846,
0.261538461538462,0.276923076923077,0.292307692307692,0.307692307692308,
0.323076923076923,0.338461538461538,0.353846153846154,0.369230769230769,
0.384615384615385,0.4,0.415384615384615,0.430769230769231,0.446153846153846,
0.461538461538462,0.476923076923077,0.492307692307692,0.507692307692308,
0.523076923076923,0.538461538461538,0.553846153846154,0.569230769230769,
0.584615384615384,0.6,0.615384615384615,0.63076923076923,0.646153846153846,
0.661538461538461,0.676923076923076,0.692307692307692,0.707692307692307,
0.723076923076922,0.738461538461538,0.753846153846153,0.769230769230768,
0.784615384615384,0.799999999999999,0.815384615384614,0.83076923076923,
0.846153846153845,0.86153846153846,0.876923076923076,0.892307692307691,
0.907692307692306,0.923076923076922,0.938461538461537,0.953846153846152,
0.969230769230768,0.984615384615383,0.994228156739694),.UNSPECIFIED.)
CURVE()
GEOMETRIC_REPRESENTATION_ITEM()
RATIONAL_B_SPLINE_CURVE((1.,1.,1.,1.,1.,1.,1.,1.,1.,1.,1.,1.,1.,1.,1.,1.,
1.,1.,1.,1.,1.,1.,1.,1.,1.,1.,1.,1.,1.,1.,1.,1.,1.,1.,1.,1.,1.,1.,1.,1.,
1.,1.,1.,1.,1.,1.,1.,1.,1.,1.,1.,1.,1.,1.,1.,1.,1.,1.,1.,1.,1.,1.,1.,1.,
1.,1.,1.,1.,1.,1.))
REPRESENTATION_ITEM('')
);
#245=(
BOUNDED_CURVE()
B_SPLINE_CURVE(5,(#41263,#41264,#41265,#41266,#41267,#41268,#41269,#41270,
#41271,#41272,#41273,#41274,#41275,#41276,#41277,#41278,#41279,#41280,#41281,
#41282,#41283,#41284,#41285,#41286,#41287,#41288,#41289,#41290,#41291,#41292,
#41293,#41294,#41295,#41296,#41297,#41298,#41299,#41300,#41301,#41302,#41303,
#41304,#41305,#41306,#41307,#41308,#41309,#41310,#41311,#41312,#41313,#41314,
#41315,#41316,#41317,#41318,#41319,#41320,#41321,#41322,#41323,#41324,#41325,
#41326,#41327,#41328,#41329,#41330,#41331,#41332),.UNSPECIFIED.,.F.,.F.)
B_SPLINE_CURVE_WITH_KNOTS((6,1,1,1,1,1,1,1,1,1,1,1,1,1,1,1,1,1,1,1,1,1,
1,1,1,1,1,1,1,1,1,1,1,1,1,1,1,1,1,1,1,1,1,1,1,1,1,1,1,1,1,1,1,1,1,1,1,1,
1,1,1,1,1,1,1,6),(0.00577184337452044,0.0153846153846154,0.0307692307692308,
0.0461538461538462,0.0615384615384615,0.0769230769230769,0.0923076923076923,
0.107692307692308,0.123076923076923,0.138461538461538,0.153846153846154,
0.169230769230769,0.184615384615385,0.2,0.215384615384615,0.230769230769231,
0.246153846153846,0.261538461538462,0.276923076923077,0.292307692307692,
0.307692307692308,0.323076923076923,0.338461538461538,0.353846153846154,
0.369230769230769,0.384615384615385,0.4,0.415384615384615,0.430769230769231,
0.446153846153846,0.461538461538462,0.476923076923077,0.492307692307692,
0.507692307692308,0.523076923076923,0.538461538461538,0.553846153846154,
0.569230769230769,0.584615384615384,0.6,0.615384615384615,0.63076923076923,
0.646153846153846,0.661538461538461,0.676923076923076,0.692307692307692,
0.707692307692307,0.723076923076922,0.738461538461538,0.753846153846153,
0.769230769230768,0.784615384615384,0.799999999999999,0.815384615384614,
0.83076923076923,0.846153846153845,0.86153846153846,0.876923076923076,0.892307692307691,
0.907692307692306,0.923076923076922,0.938461538461537,0.953846153846152,
0.969230769230768,0.984615384615383,1.),.UNSPECIFIED.)
CURVE()
GEOMETRIC_REPRESENTATION_ITEM()
RATIONAL_B_SPLINE_CURVE((1.,1.,1.,1.,1.,1.,1.,1.,1.,1.,1.,1.,1.,1.,1.,1.,
1.,1.,1.,1.,1.,1.,1.,1.,1.,1.,1.,1.,1.,1.,1.,1.,1.,1.,1.,1.,1.,1.,1.,1.,
1.,1.,1.,1.,1.,1.,1.,1.,1.,1.,1.,1.,1.,1.,1.,1.,1.,1.,1.,1.,1.,1.,1.,1.,
1.,1.,1.,1.,1.,1.))
REPRESENTATION_ITEM('')
);
#246=(
BOUNDED_CURVE()
B_SPLINE_CURVE(5,(#41336,#41337,#41338,#41339,#41340,#41341,#41342,#41343,
#41344,#41345,#41346,#41347,#41348,#41349,#41350,#41351,#41352,#41353,#41354,
#41355,#41356,#41357,#41358,#41359,#41360,#41361,#41362,#41363,#41364,#41365,
#41366,#41367,#41368,#41369,#41370,#41371,#41372,#41373,#41374,#41375,#41376,
#41377,#41378,#41379,#41380,#41381,#41382,#41383,#41384,#41385,#41386,#41387,
#41388,#41389,#41390,#41391,#41392,#41393,#41394,#41395,#41396,#41397,#41398,
#41399,#41400,#41401,#41402,#41403,#41404,#41405),.UNSPECIFIED.,.F.,.F.)
B_SPLINE_CURVE_WITH_KNOTS((6,1,1,1,1,1,1,1,1,1,1,1,1,1,1,1,1,1,1,1,1,1,
1,1,1,1,1,1,1,1,1,1,1,1,1,1,1,1,1,1,1,1,1,1,1,1,1,1,1,1,1,1,1,1,1,1,1,1,
1,1,1,1,1,1,1,6),(0.,0.0153846153846154,0.0307692307692308,0.0461538461538462,
0.0615384615384615,0.0769230769230769,0.0923076923076923,0.107692307692308,
0.123076923076923,0.138461538461538,0.153846153846154,0.169230769230769,
0.184615384615385,0.2,0.215384615384615,0.230769230769231,0.246153846153846,
0.261538461538462,0.276923076923077,0.292307692307692,0.307692307692308,
0.323076923076923,0.338461538461538,0.353846153846154,0.369230769230769,
0.384615384615385,0.4,0.415384615384615,0.430769230769231,0.446153846153846,
0.461538461538462,0.476923076923077,0.492307692307692,0.507692307692308,
0.523076923076923,0.538461538461538,0.553846153846154,0.569230769230769,
0.584615384615384,0.6,0.615384615384615,0.63076923076923,0.646153846153846,
0.661538461538461,0.676923076923076,0.692307692307692,0.707692307692307,
0.723076923076922,0.738461538461538,0.753846153846153,0.769230769230768,
0.784615384615384,0.799999999999999,0.815384615384614,0.83076923076923,
0.846153846153845,0.86153846153846,0.876923076923076,0.892307692307691,
0.907692307692306,0.923076923076922,0.938461538461537,0.953846153846152,
0.969230769230768,0.984615384615383,0.994228156739698),.UNSPECIFIED.)
CURVE()
GEOMETRIC_REPRESENTATION_ITEM()
RATIONAL_B_SPLINE_CURVE((1.,1.,1.,1.,1.,1.,1.,1.,1.,1.,1.,1.,1.,1.,1.,1.,
1.,1.,1.,1.,1.,1.,1.,1.,1.,1.,1.,1.,1.,1.,1.,1.,1.,1.,1.,1.,1.,1.,1.,1.,
1.,1.,1.,1.,1.,1.,1.,1.,1.,1.,1.,1.,1.,1.,1.,1.,1.,1.,1.,1.,1.,1.,1.,1.,
1.,1.,1.,1.,1.,1.))
REPRESENTATION_ITEM('')
);
#247=(
BOUNDED_CURVE()
B_SPLINE_CURVE(5,(#41409,#41410,#41411,#41412,#41413,#41414,#41415,#41416,
#41417,#41418,#41419,#41420,#41421,#41422,#41423,#41424,#41425,#41426,#41427,
#41428,#41429,#41430,#41431,#41432,#41433,#41434,#41435,#41436,#41437,#41438,
#41439,#41440,#41441,#41442,#41443,#41444,#41445,#41446,#41447,#41448,#41449,
#41450,#41451,#41452,#41453,#41454,#41455,#41456,#41457,#41458,#41459,#41460,
#41461,#41462,#41463,#41464,#41465,#41466,#41467,#41468,#41469,#41470,#41471,
#41472,#41473,#41474,#41475,#41476,#41477,#41478),.UNSPECIFIED.,.F.,.F.)
B_SPLINE_CURVE_WITH_KNOTS((6,1,1,1,1,1,1,1,1,1,1,1,1,1,1,1,1,1,1,1,1,1,
1,1,1,1,1,1,1,1,1,1,1,1,1,1,1,1,1,1,1,1,1,1,1,1,1,1,1,1,1,1,1,1,1,1,1,1,
1,1,1,1,1,1,1,6),(0.00577184337451607,0.0153846153846154,0.0307692307692308,
0.0461538461538462,0.0615384615384615,0.0769230769230769,0.0923076923076923,
0.107692307692308,0.123076923076923,0.138461538461538,0.153846153846154,
0.169230769230769,0.184615384615385,0.2,0.215384615384615,0.230769230769231,
0.246153846153846,0.261538461538462,0.276923076923077,0.292307692307692,
0.307692307692308,0.323076923076923,0.338461538461538,0.353846153846154,
0.369230769230769,0.384615384615385,0.4,0.415384615384615,0.430769230769231,
0.446153846153846,0.461538461538462,0.476923076923077,0.492307692307692,
0.507692307692308,0.523076923076923,0.538461538461538,0.553846153846154,
0.569230769230769,0.584615384615384,0.6,0.615384615384615,0.63076923076923,
0.646153846153846,0.661538461538461,0.676923076923076,0.692307692307692,
0.707692307692307,0.723076923076922,0.738461538461538,0.753846153846153,
0.769230769230768,0.784615384615384,0.799999999999999,0.815384615384614,
0.83076923076923,0.846153846153845,0.86153846153846,0.876923076923076,0.892307692307691,
0.907692307692306,0.923076923076922,0.938461538461537,0.953846153846152,
0.969230769230768,0.984615384615383,1.),.UNSPECIFIED.)
CURVE()
GEOMETRIC_REPRESENTATION_ITEM()
RATIONAL_B_SPLINE_CURVE((1.,1.,1.,1.,1.,1.,1.,1.,1.,1.,1.,1.,1.,1.,1.,1.,
1.,1.,1.,1.,1.,1.,1.,1.,1.,1.,1.,1.,1.,1.,1.,1.,1.,1.,1.,1.,1.,1.,1.,1.,
1.,1.,1.,1.,1.,1.,1.,1.,1.,1.,1.,1.,1.,1.,1.,1.,1.,1.,1.,1.,1.,1.,1.,1.,
1.,1.,1.,1.,1.,1.))
REPRESENTATION_ITEM('')
);
#248=(
BOUNDED_CURVE()
B_SPLINE_CURVE(5,(#41482,#41483,#41484,#41485,#41486,#41487,#41488,#41489,
#41490,#41491,#41492,#41493,#41494,#41495,#41496,#41497,#41498,#41499,#41500,
#41501,#41502,#41503,#41504,#41505,#41506,#41507,#41508,#41509,#41510,#41511,
#41512,#41513,#41514,#41515,#41516,#41517,#41518,#41519,#41520,#41521,#41522,
#41523,#41524,#41525,#41526,#41527,#41528,#41529,#41530,#41531,#41532,#41533,
#41534,#41535,#41536,#41537,#41538,#41539,#41540,#41541,#41542,#41543,#41544,
#41545,#41546,#41547,#41548,#41549,#41550,#41551),.UNSPECIFIED.,.F.,.F.)
B_SPLINE_CURVE_WITH_KNOTS((6,1,1,1,1,1,1,1,1,1,1,1,1,1,1,1,1,1,1,1,1,1,
1,1,1,1,1,1,1,1,1,1,1,1,1,1,1,1,1,1,1,1,1,1,1,1,1,1,1,1,1,1,1,1,1,1,1,1,
1,1,1,1,1,1,1,6),(0.,0.0153846153846154,0.0307692307692308,0.0461538461538462,
0.0615384615384615,0.0769230769230769,0.0923076923076923,0.107692307692308,
0.123076923076923,0.138461538461538,0.153846153846154,0.169230769230769,
0.184615384615385,0.2,0.215384615384615,0.230769230769231,0.246153846153846,
0.261538461538462,0.276923076923077,0.292307692307692,0.307692307692308,
0.323076923076923,0.338461538461538,0.353846153846154,0.369230769230769,
0.384615384615385,0.4,0.415384615384615,0.430769230769231,0.446153846153846,
0.461538461538462,0.476923076923077,0.492307692307692,0.507692307692308,
0.523076923076923,0.538461538461538,0.553846153846154,0.569230769230769,
0.584615384615384,0.6,0.615384615384615,0.63076923076923,0.646153846153846,
0.661538461538461,0.676923076923076,0.692307692307692,0.707692307692307,
0.723076923076922,0.738461538461538,0.753846153846153,0.769230769230768,
0.784615384615384,0.799999999999999,0.815384615384614,0.83076923076923,
0.846153846153845,0.86153846153846,0.876923076923076,0.892307692307691,
0.907692307692306,0.923076923076922,0.938461538461537,0.953846153846152,
0.969230769230768,0.984615384615383,0.994228156739704),.UNSPECIFIED.)
CURVE()
GEOMETRIC_REPRESENTATION_ITEM()
RATIONAL_B_SPLINE_CURVE((1.,1.,1.,1.,1.,1.,1.,1.,1.,1.,1.,1.,1.,1.,1.,1.,
1.,1.,1.,1.,1.,1.,1.,1.,1.,1.,1.,1.,1.,1.,1.,1.,1.,1.,1.,1.,1.,1.,1.,1.,
1.,1.,1.,1.,1.,1.,1.,1.,1.,1.,1.,1.,1.,1.,1.,1.,1.,1.,1.,1.,1.,1.,1.,1.,
1.,1.,1.,1.,1.,1.))
REPRESENTATION_ITEM('')
);
#249=(
BOUNDED_CURVE()
B_SPLINE_CURVE(5,(#41555,#41556,#41557,#41558,#41559,#41560,#41561,#41562,
#41563,#41564,#41565,#41566,#41567,#41568,#41569,#41570,#41571,#41572,#41573,
#41574,#41575,#41576,#41577,#41578,#41579,#41580,#41581,#41582,#41583,#41584,
#41585,#41586,#41587,#41588,#41589,#41590,#41591,#41592,#41593,#41594,#41595,
#41596,#41597,#41598,#41599,#41600,#41601,#41602,#41603,#41604,#41605,#41606,
#41607,#41608,#41609,#41610,#41611,#41612,#41613,#41614,#41615,#41616,#41617,
#41618,#41619,#41620,#41621,#41622,#41623,#41624),.UNSPECIFIED.,.F.,.F.)
B_SPLINE_CURVE_WITH_KNOTS((6,1,1,1,1,1,1,1,1,1,1,1,1,1,1,1,1,1,1,1,1,1,
1,1,1,1,1,1,1,1,1,1,1,1,1,1,1,1,1,1,1,1,1,1,1,1,1,1,1,1,1,1,1,1,1,1,1,1,
1,1,1,1,1,1,1,6),(0.00577184337449682,0.0153846153846154,0.0307692307692308,
0.0461538461538462,0.0615384615384615,0.0769230769230769,0.0923076923076923,
0.107692307692308,0.123076923076923,0.138461538461538,0.153846153846154,
0.169230769230769,0.184615384615385,0.2,0.215384615384615,0.230769230769231,
0.246153846153846,0.261538461538462,0.276923076923077,0.292307692307692,
0.307692307692308,0.323076923076923,0.338461538461538,0.353846153846154,
0.369230769230769,0.384615384615385,0.4,0.415384615384615,0.430769230769231,
0.446153846153846,0.461538461538462,0.476923076923077,0.492307692307692,
0.507692307692308,0.523076923076923,0.538461538461538,0.553846153846154,
0.569230769230769,0.584615384615384,0.6,0.615384615384615,0.63076923076923,
0.646153846153846,0.661538461538461,0.676923076923076,0.692307692307692,
0.707692307692307,0.723076923076922,0.738461538461538,0.753846153846153,
0.769230769230768,0.784615384615384,0.799999999999999,0.815384615384614,
0.83076923076923,0.846153846153845,0.86153846153846,0.876923076923076,0.892307692307691,
0.907692307692306,0.923076923076922,0.938461538461537,0.953846153846152,
0.969230769230768,0.984615384615383,1.),.UNSPECIFIED.)
CURVE()
GEOMETRIC_REPRESENTATION_ITEM()
RATIONAL_B_SPLINE_CURVE((1.,1.,1.,1.,1.,1.,1.,1.,1.,1.,1.,1.,1.,1.,1.,1.,
1.,1.,1.,1.,1.,1.,1.,1.,1.,1.,1.,1.,1.,1.,1.,1.,1.,1.,1.,1.,1.,1.,1.,1.,
1.,1.,1.,1.,1.,1.,1.,1.,1.,1.,1.,1.,1.,1.,1.,1.,1.,1.,1.,1.,1.,1.,1.,1.,
1.,1.,1.,1.,1.,1.))
REPRESENTATION_ITEM('')
);
#250=(
BOUNDED_CURVE()
B_SPLINE_CURVE(5,(#41628,#41629,#41630,#41631,#41632,#41633,#41634,#41635,
#41636,#41637,#41638,#41639,#41640,#41641,#41642,#41643,#41644,#41645,#41646,
#41647,#41648,#41649,#41650,#41651,#41652,#41653,#41654,#41655,#41656,#41657,
#41658,#41659,#41660,#41661,#41662,#41663,#41664,#41665,#41666,#41667,#41668,
#41669,#41670,#41671,#41672,#41673,#41674,#41675,#41676,#41677,#41678,#41679,
#41680,#41681,#41682,#41683,#41684,#41685,#41686,#41687,#41688,#41689,#41690,
#41691,#41692,#41693,#41694,#41695,#41696,#41697),.UNSPECIFIED.,.F.,.F.)
B_SPLINE_CURVE_WITH_KNOTS((6,1,1,1,1,1,1,1,1,1,1,1,1,1,1,1,1,1,1,1,1,1,
1,1,1,1,1,1,1,1,1,1,1,1,1,1,1,1,1,1,1,1,1,1,1,1,1,1,1,1,1,1,1,1,1,1,1,1,
1,1,1,1,1,1,1,6),(0.,0.0153846153846154,0.0307692307692308,0.0461538461538462,
0.0615384615384615,0.0769230769230769,0.0923076923076923,0.107692307692308,
0.123076923076923,0.138461538461538,0.153846153846154,0.169230769230769,
0.184615384615385,0.2,0.215384615384615,0.230769230769231,0.246153846153846,
0.261538461538462,0.276923076923077,0.292307692307692,0.307692307692308,
0.323076923076923,0.338461538461538,0.353846153846154,0.369230769230769,
0.384615384615385,0.4,0.415384615384615,0.430769230769231,0.446153846153846,
0.461538461538462,0.476923076923077,0.492307692307692,0.507692307692308,
0.523076923076923,0.538461538461538,0.553846153846154,0.569230769230769,
0.584615384615384,0.6,0.615384615384615,0.63076923076923,0.646153846153846,
0.661538461538461,0.676923076923076,0.692307692307692,0.707692307692307,
0.723076923076922,0.738461538461538,0.753846153846153,0.769230769230768,
0.784615384615384,0.799999999999999,0.815384615384614,0.83076923076923,
0.846153846153845,0.86153846153846,0.876923076923076,0.892307692307691,
0.907692307692306,0.923076923076922,0.938461538461537,0.953846153846152,
0.969230769230768,0.984615384615383,0.994228156739711),.UNSPECIFIED.)
CURVE()
GEOMETRIC_REPRESENTATION_ITEM()
RATIONAL_B_SPLINE_CURVE((1.,1.,1.,1.,1.,1.,1.,1.,1.,1.,1.,1.,1.,1.,1.,1.,
1.,1.,1.,1.,1.,1.,1.,1.,1.,1.,1.,1.,1.,1.,1.,1.,1.,1.,1.,1.,1.,1.,1.,1.,
1.,1.,1.,1.,1.,1.,1.,1.,1.,1.,1.,1.,1.,1.,1.,1.,1.,1.,1.,1.,1.,1.,1.,1.,
1.,1.,1.,1.,1.,1.))
REPRESENTATION_ITEM('')
);
#251=(
BOUNDED_CURVE()
B_SPLINE_CURVE(5,(#41701,#41702,#41703,#41704,#41705,#41706,#41707,#41708,
#41709,#41710,#41711,#41712,#41713,#41714,#41715,#41716,#41717,#41718,#41719,
#41720,#41721,#41722,#41723,#41724,#41725,#41726,#41727,#41728,#41729,#41730,
#41731,#41732,#41733,#41734,#41735,#41736,#41737,#41738,#41739,#41740,#41741,
#41742,#41743,#41744,#41745,#41746,#41747,#41748,#41749,#41750,#41751,#41752,
#41753,#41754,#41755,#41756,#41757,#41758,#41759,#41760,#41761,#41762,#41763,
#41764,#41765,#41766,#41767,#41768,#41769,#41770),.UNSPECIFIED.,.F.,.F.)
B_SPLINE_CURVE_WITH_KNOTS((6,1,1,1,1,1,1,1,1,1,1,1,1,1,1,1,1,1,1,1,1,1,
1,1,1,1,1,1,1,1,1,1,1,1,1,1,1,1,1,1,1,1,1,1,1,1,1,1,1,1,1,1,1,1,1,1,1,1,
1,1,1,1,1,1,1,6),(0.00577184337450313,0.0153846153846154,0.0307692307692308,
0.0461538461538462,0.0615384615384615,0.0769230769230769,0.0923076923076923,
0.107692307692308,0.123076923076923,0.138461538461538,0.153846153846154,
0.169230769230769,0.184615384615385,0.2,0.215384615384615,0.230769230769231,
0.246153846153846,0.261538461538462,0.276923076923077,0.292307692307692,
0.307692307692308,0.323076923076923,0.338461538461538,0.353846153846154,
0.369230769230769,0.384615384615385,0.4,0.415384615384615,0.430769230769231,
0.446153846153846,0.461538461538462,0.476923076923077,0.492307692307692,
0.507692307692308,0.523076923076923,0.538461538461538,0.553846153846154,
0.569230769230769,0.584615384615384,0.6,0.615384615384615,0.63076923076923,
0.646153846153846,0.661538461538461,0.676923076923076,0.692307692307692,
0.707692307692307,0.723076923076922,0.738461538461538,0.753846153846153,
0.769230769230768,0.784615384615384,0.799999999999999,0.815384615384614,
0.83076923076923,0.846153846153845,0.86153846153846,0.876923076923076,0.892307692307691,
0.907692307692306,0.923076923076922,0.938461538461537,0.953846153846152,
0.969230769230768,0.984615384615383,1.),.UNSPECIFIED.)
CURVE()
GEOMETRIC_REPRESENTATION_ITEM()
RATIONAL_B_SPLINE_CURVE((1.,1.,1.,1.,1.,1.,1.,1.,1.,1.,1.,1.,1.,1.,1.,1.,
1.,1.,1.,1.,1.,1.,1.,1.,1.,1.,1.,1.,1.,1.,1.,1.,1.,1.,1.,1.,1.,1.,1.,1.,
1.,1.,1.,1.,1.,1.,1.,1.,1.,1.,1.,1.,1.,1.,1.,1.,1.,1.,1.,1.,1.,1.,1.,1.,
1.,1.,1.,1.,1.,1.))
REPRESENTATION_ITEM('')
);
#252=(
BOUNDED_CURVE()
B_SPLINE_CURVE(5,(#41774,#41775,#41776,#41777,#41778,#41779,#41780,#41781,
#41782,#41783,#41784,#41785,#41786,#41787,#41788,#41789,#41790,#41791,#41792,
#41793,#41794,#41795,#41796,#41797,#41798,#41799,#41800,#41801,#41802,#41803,
#41804,#41805,#41806,#41807,#41808,#41809,#41810,#41811,#41812,#41813,#41814,
#41815,#41816,#41817,#41818,#41819,#41820,#41821,#41822,#41823,#41824,#41825,
#41826,#41827,#41828,#41829,#41830,#41831,#41832,#41833,#41834,#41835,#41836,
#41837,#41838,#41839,#41840,#41841,#41842,#41843),.UNSPECIFIED.,.F.,.F.)
B_SPLINE_CURVE_WITH_KNOTS((6,1,1,1,1,1,1,1,1,1,1,1,1,1,1,1,1,1,1,1,1,1,
1,1,1,1,1,1,1,1,1,1,1,1,1,1,1,1,1,1,1,1,1,1,1,1,1,1,1,1,1,1,1,1,1,1,1,1,
1,1,1,1,1,1,1,6),(0.,0.0153846153846154,0.0307692307692308,0.0461538461538462,
0.0615384615384615,0.0769230769230769,0.0923076923076923,0.107692307692308,
0.123076923076923,0.138461538461538,0.153846153846154,0.169230769230769,
0.184615384615385,0.2,0.215384615384615,0.230769230769231,0.246153846153846,
0.261538461538462,0.276923076923077,0.292307692307692,0.307692307692308,
0.323076923076923,0.338461538461538,0.353846153846154,0.369230769230769,
0.384615384615385,0.4,0.415384615384615,0.430769230769231,0.446153846153846,
0.461538461538462,0.476923076923077,0.492307692307692,0.507692307692308,
0.523076923076923,0.538461538461538,0.553846153846154,0.569230769230769,
0.584615384615384,0.6,0.615384615384615,0.63076923076923,0.646153846153846,
0.661538461538461,0.676923076923076,0.692307692307692,0.707692307692307,
0.723076923076922,0.738461538461538,0.753846153846153,0.769230769230768,
0.784615384615384,0.799999999999999,0.815384615384614,0.83076923076923,
0.846153846153845,0.86153846153846,0.876923076923076,0.892307692307691,
0.907692307692306,0.923076923076922,0.938461538461537,0.953846153846152,
0.969230769230768,0.984615384615383,0.9942281567397),.UNSPECIFIED.)
CURVE()
GEOMETRIC_REPRESENTATION_ITEM()
RATIONAL_B_SPLINE_CURVE((1.,1.,1.,1.,1.,1.,1.,1.,1.,1.,1.,1.,1.,1.,1.,1.,
1.,1.,1.,1.,1.,1.,1.,1.,1.,1.,1.,1.,1.,1.,1.,1.,1.,1.,1.,1.,1.,1.,1.,1.,
1.,1.,1.,1.,1.,1.,1.,1.,1.,1.,1.,1.,1.,1.,1.,1.,1.,1.,1.,1.,1.,1.,1.,1.,
1.,1.,1.,1.,1.,1.))
REPRESENTATION_ITEM('')
);
#253=(
BOUNDED_CURVE()
B_SPLINE_CURVE(5,(#41847,#41848,#41849,#41850,#41851,#41852,#41853,#41854,
#41855,#41856,#41857,#41858,#41859,#41860,#41861,#41862,#41863,#41864,#41865,
#41866,#41867,#41868,#41869,#41870,#41871,#41872,#41873,#41874,#41875,#41876,
#41877,#41878,#41879,#41880,#41881,#41882,#41883,#41884,#41885,#41886,#41887,
#41888,#41889,#41890,#41891,#41892,#41893,#41894,#41895,#41896,#41897,#41898,
#41899,#41900,#41901,#41902,#41903,#41904,#41905,#41906,#41907,#41908,#41909,
#41910,#41911,#41912,#41913,#41914,#41915,#41916),.UNSPECIFIED.,.F.,.F.)
B_SPLINE_CURVE_WITH_KNOTS((6,1,1,1,1,1,1,1,1,1,1,1,1,1,1,1,1,1,1,1,1,1,
1,1,1,1,1,1,1,1,1,1,1,1,1,1,1,1,1,1,1,1,1,1,1,1,1,1,1,1,1,1,1,1,1,1,1,1,
1,1,1,1,1,1,1,6),(0.00577184337452087,0.0153846153846154,0.0307692307692308,
0.0461538461538462,0.0615384615384615,0.0769230769230769,0.0923076923076923,
0.107692307692308,0.123076923076923,0.138461538461538,0.153846153846154,
0.169230769230769,0.184615384615385,0.2,0.215384615384615,0.230769230769231,
0.246153846153846,0.261538461538462,0.276923076923077,0.292307692307692,
0.307692307692308,0.323076923076923,0.338461538461538,0.353846153846154,
0.369230769230769,0.384615384615385,0.4,0.415384615384615,0.430769230769231,
0.446153846153846,0.461538461538462,0.476923076923077,0.492307692307692,
0.507692307692308,0.523076923076923,0.538461538461538,0.553846153846154,
0.569230769230769,0.584615384615384,0.6,0.615384615384615,0.63076923076923,
0.646153846153846,0.661538461538461,0.676923076923076,0.692307692307692,
0.707692307692307,0.723076923076922,0.738461538461538,0.753846153846153,
0.769230769230768,0.784615384615384,0.799999999999999,0.815384615384614,
0.83076923076923,0.846153846153845,0.86153846153846,0.876923076923076,0.892307692307691,
0.907692307692306,0.923076923076922,0.938461538461537,0.953846153846152,
0.969230769230768,0.984615384615383,1.),.UNSPECIFIED.)
CURVE()
GEOMETRIC_REPRESENTATION_ITEM()
RATIONAL_B_SPLINE_CURVE((1.,1.,1.,1.,1.,1.,1.,1.,1.,1.,1.,1.,1.,1.,1.,1.,
1.,1.,1.,1.,1.,1.,1.,1.,1.,1.,1.,1.,1.,1.,1.,1.,1.,1.,1.,1.,1.,1.,1.,1.,
1.,1.,1.,1.,1.,1.,1.,1.,1.,1.,1.,1.,1.,1.,1.,1.,1.,1.,1.,1.,1.,1.,1.,1.,
1.,1.,1.,1.,1.,1.))
REPRESENTATION_ITEM('')
);
#254=(
BOUNDED_CURVE()
B_SPLINE_CURVE(5,(#41920,#41921,#41922,#41923,#41924,#41925,#41926,#41927,
#41928,#41929,#41930,#41931,#41932,#41933,#41934,#41935,#41936,#41937,#41938,
#41939,#41940,#41941,#41942,#41943,#41944,#41945,#41946,#41947,#41948,#41949,
#41950,#41951,#41952,#41953,#41954,#41955,#41956,#41957,#41958,#41959,#41960,
#41961,#41962,#41963,#41964,#41965,#41966,#41967,#41968,#41969,#41970,#41971,
#41972,#41973,#41974,#41975,#41976,#41977,#41978,#41979,#41980,#41981,#41982,
#41983,#41984,#41985,#41986,#41987,#41988,#41989),.UNSPECIFIED.,.F.,.F.)
B_SPLINE_CURVE_WITH_KNOTS((6,1,1,1,1,1,1,1,1,1,1,1,1,1,1,1,1,1,1,1,1,1,
1,1,1,1,1,1,1,1,1,1,1,1,1,1,1,1,1,1,1,1,1,1,1,1,1,1,1,1,1,1,1,1,1,1,1,1,
1,1,1,1,1,1,1,6),(0.,0.0153846153846154,0.0307692307692308,0.0461538461538462,
0.0615384615384615,0.0769230769230769,0.0923076923076923,0.107692307692308,
0.123076923076923,0.138461538461538,0.153846153846154,0.169230769230769,
0.184615384615385,0.2,0.215384615384615,0.230769230769231,0.246153846153846,
0.261538461538462,0.276923076923077,0.292307692307692,0.307692307692308,
0.323076923076923,0.338461538461538,0.353846153846154,0.369230769230769,
0.384615384615385,0.4,0.415384615384615,0.430769230769231,0.446153846153846,
0.461538461538462,0.476923076923077,0.492307692307692,0.507692307692308,
0.523076923076923,0.538461538461538,0.553846153846154,0.569230769230769,
0.584615384615384,0.6,0.615384615384615,0.63076923076923,0.646153846153846,
0.661538461538461,0.676923076923076,0.692307692307692,0.707692307692307,
0.723076923076922,0.738461538461538,0.753846153846153,0.769230769230768,
0.784615384615384,0.799999999999999,0.815384615384614,0.83076923076923,
0.846153846153845,0.86153846153846,0.876923076923076,0.892307692307691,
0.907692307692306,0.923076923076922,0.938461538461537,0.953846153846152,
0.969230769230768,0.984615384615383,0.994228156739692),.UNSPECIFIED.)
CURVE()
GEOMETRIC_REPRESENTATION_ITEM()
RATIONAL_B_SPLINE_CURVE((1.,1.,1.,1.,1.,1.,1.,1.,1.,1.,1.,1.,1.,1.,1.,1.,
1.,1.,1.,1.,1.,1.,1.,1.,1.,1.,1.,1.,1.,1.,1.,1.,1.,1.,1.,1.,1.,1.,1.,1.,
1.,1.,1.,1.,1.,1.,1.,1.,1.,1.,1.,1.,1.,1.,1.,1.,1.,1.,1.,1.,1.,1.,1.,1.,
1.,1.,1.,1.,1.,1.))
REPRESENTATION_ITEM('')
);
#255=(
BOUNDED_CURVE()
B_SPLINE_CURVE(5,(#41993,#41994,#41995,#41996,#41997,#41998,#41999,#42000,
#42001,#42002,#42003,#42004,#42005,#42006,#42007,#42008,#42009,#42010,#42011,
#42012,#42013,#42014,#42015,#42016,#42017,#42018,#42019,#42020,#42021,#42022,
#42023,#42024,#42025,#42026,#42027,#42028,#42029,#42030,#42031,#42032,#42033,
#42034,#42035,#42036,#42037,#42038,#42039,#42040,#42041,#42042,#42043,#42044,
#42045,#42046,#42047,#42048,#42049,#42050,#42051,#42052,#42053,#42054,#42055,
#42056,#42057,#42058,#42059,#42060,#42061,#42062),.UNSPECIFIED.,.F.,.F.)
B_SPLINE_CURVE_WITH_KNOTS((6,1,1,1,1,1,1,1,1,1,1,1,1,1,1,1,1,1,1,1,1,1,
1,1,1,1,1,1,1,1,1,1,1,1,1,1,1,1,1,1,1,1,1,1,1,1,1,1,1,1,1,1,1,1,1,1,1,1,
1,1,1,1,1,1,1,6),(0.00577184337450777,0.0153846153846154,0.0307692307692308,
0.0461538461538462,0.0615384615384615,0.0769230769230769,0.0923076923076923,
0.107692307692308,0.123076923076923,0.138461538461538,0.153846153846154,
0.169230769230769,0.184615384615385,0.2,0.215384615384615,0.230769230769231,
0.246153846153846,0.261538461538462,0.276923076923077,0.292307692307692,
0.307692307692308,0.323076923076923,0.338461538461538,0.353846153846154,
0.369230769230769,0.384615384615385,0.4,0.415384615384615,0.430769230769231,
0.446153846153846,0.461538461538462,0.476923076923077,0.492307692307692,
0.507692307692308,0.523076923076923,0.538461538461538,0.553846153846154,
0.569230769230769,0.584615384615384,0.6,0.615384615384615,0.63076923076923,
0.646153846153846,0.661538461538461,0.676923076923076,0.692307692307692,
0.707692307692307,0.723076923076922,0.738461538461538,0.753846153846153,
0.769230769230768,0.784615384615384,0.799999999999999,0.815384615384614,
0.83076923076923,0.846153846153845,0.86153846153846,0.876923076923076,0.892307692307691,
0.907692307692306,0.923076923076922,0.938461538461537,0.953846153846152,
0.969230769230768,0.984615384615383,1.),.UNSPECIFIED.)
CURVE()
GEOMETRIC_REPRESENTATION_ITEM()
RATIONAL_B_SPLINE_CURVE((1.,1.,1.,1.,1.,1.,1.,1.,1.,1.,1.,1.,1.,1.,1.,1.,
1.,1.,1.,1.,1.,1.,1.,1.,1.,1.,1.,1.,1.,1.,1.,1.,1.,1.,1.,1.,1.,1.,1.,1.,
1.,1.,1.,1.,1.,1.,1.,1.,1.,1.,1.,1.,1.,1.,1.,1.,1.,1.,1.,1.,1.,1.,1.,1.,
1.,1.,1.,1.,1.,1.))
REPRESENTATION_ITEM('')
);
#256=(
BOUNDED_CURVE()
B_SPLINE_CURVE(5,(#42066,#42067,#42068,#42069,#42070,#42071,#42072,#42073,
#42074,#42075,#42076,#42077,#42078,#42079,#42080,#42081,#42082,#42083,#42084,
#42085,#42086,#42087,#42088,#42089,#42090,#42091,#42092,#42093,#42094,#42095,
#42096,#42097,#42098,#42099,#42100,#42101,#42102,#42103,#42104,#42105,#42106,
#42107,#42108,#42109,#42110,#42111,#42112,#42113,#42114,#42115,#42116,#42117,
#42118,#42119,#42120,#42121,#42122,#42123,#42124,#42125,#42126,#42127,#42128,
#42129,#42130,#42131,#42132,#42133,#42134,#42135),.UNSPECIFIED.,.F.,.F.)
B_SPLINE_CURVE_WITH_KNOTS((6,1,1,1,1,1,1,1,1,1,1,1,1,1,1,1,1,1,1,1,1,1,
1,1,1,1,1,1,1,1,1,1,1,1,1,1,1,1,1,1,1,1,1,1,1,1,1,1,1,1,1,1,1,1,1,1,1,1,
1,1,1,1,1,1,1,6),(0.,0.0153846153846154,0.0307692307692308,0.0461538461538462,
0.0615384615384615,0.0769230769230769,0.0923076923076923,0.107692307692308,
0.123076923076923,0.138461538461538,0.153846153846154,0.169230769230769,
0.184615384615385,0.2,0.215384615384615,0.230769230769231,0.246153846153846,
0.261538461538462,0.276923076923077,0.292307692307692,0.307692307692308,
0.323076923076923,0.338461538461538,0.353846153846154,0.369230769230769,
0.384615384615385,0.4,0.415384615384615,0.430769230769231,0.446153846153846,
0.461538461538462,0.476923076923077,0.492307692307692,0.507692307692308,
0.523076923076923,0.538461538461538,0.553846153846154,0.569230769230769,
0.584615384615384,0.6,0.615384615384615,0.63076923076923,0.646153846153846,
0.661538461538461,0.676923076923076,0.692307692307692,0.707692307692307,
0.723076923076922,0.738461538461538,0.753846153846153,0.769230769230768,
0.784615384615384,0.799999999999999,0.815384615384614,0.83076923076923,
0.846153846153845,0.86153846153846,0.876923076923076,0.892307692307691,
0.907692307692306,0.923076923076922,0.938461538461537,0.953846153846152,
0.969230769230768,0.984615384615383,0.994228156739701),.UNSPECIFIED.)
CURVE()
GEOMETRIC_REPRESENTATION_ITEM()
RATIONAL_B_SPLINE_CURVE((1.,1.,1.,1.,1.,1.,1.,1.,1.,1.,1.,1.,1.,1.,1.,1.,
1.,1.,1.,1.,1.,1.,1.,1.,1.,1.,1.,1.,1.,1.,1.,1.,1.,1.,1.,1.,1.,1.,1.,1.,
1.,1.,1.,1.,1.,1.,1.,1.,1.,1.,1.,1.,1.,1.,1.,1.,1.,1.,1.,1.,1.,1.,1.,1.,
1.,1.,1.,1.,1.,1.))
REPRESENTATION_ITEM('')
);
#257=(
BOUNDED_CURVE()
B_SPLINE_CURVE(5,(#42139,#42140,#42141,#42142,#42143,#42144,#42145,#42146,
#42147,#42148,#42149,#42150,#42151,#42152,#42153,#42154,#42155,#42156,#42157,
#42158,#42159,#42160,#42161,#42162,#42163,#42164,#42165,#42166,#42167,#42168,
#42169,#42170,#42171,#42172,#42173,#42174,#42175,#42176,#42177,#42178,#42179,
#42180,#42181,#42182,#42183,#42184,#42185,#42186,#42187,#42188,#42189,#42190,
#42191,#42192,#42193,#42194,#42195,#42196,#42197,#42198,#42199,#42200,#42201,
#42202,#42203,#42204,#42205,#42206,#42207,#42208),.UNSPECIFIED.,.F.,.F.)
B_SPLINE_CURVE_WITH_KNOTS((6,1,1,1,1,1,1,1,1,1,1,1,1,1,1,1,1,1,1,1,1,1,
1,1,1,1,1,1,1,1,1,1,1,1,1,1,1,1,1,1,1,1,1,1,1,1,1,1,1,1,1,1,1,1,1,1,1,1,
1,1,1,1,1,1,1,6),(0.00577184337450943,0.0153846153846154,0.0307692307692308,
0.0461538461538462,0.0615384615384615,0.0769230769230769,0.0923076923076923,
0.107692307692308,0.123076923076923,0.138461538461538,0.153846153846154,
0.169230769230769,0.184615384615385,0.2,0.215384615384615,0.230769230769231,
0.246153846153846,0.261538461538462,0.276923076923077,0.292307692307692,
0.307692307692308,0.323076923076923,0.338461538461538,0.353846153846154,
0.369230769230769,0.384615384615385,0.4,0.415384615384615,0.430769230769231,
0.446153846153846,0.461538461538462,0.476923076923077,0.492307692307692,
0.507692307692308,0.523076923076923,0.538461538461538,0.553846153846154,
0.569230769230769,0.584615384615384,0.6,0.615384615384615,0.63076923076923,
0.646153846153846,0.661538461538461,0.676923076923076,0.692307692307692,
0.707692307692307,0.723076923076922,0.738461538461538,0.753846153846153,
0.769230769230768,0.784615384615384,0.799999999999999,0.815384615384614,
0.83076923076923,0.846153846153845,0.86153846153846,0.876923076923076,0.892307692307691,
0.907692307692306,0.923076923076922,0.938461538461537,0.953846153846152,
0.969230769230768,0.984615384615383,1.),.UNSPECIFIED.)
CURVE()
GEOMETRIC_REPRESENTATION_ITEM()
RATIONAL_B_SPLINE_CURVE((1.,1.,1.,1.,1.,1.,1.,1.,1.,1.,1.,1.,1.,1.,1.,1.,
1.,1.,1.,1.,1.,1.,1.,1.,1.,1.,1.,1.,1.,1.,1.,1.,1.,1.,1.,1.,1.,1.,1.,1.,
1.,1.,1.,1.,1.,1.,1.,1.,1.,1.,1.,1.,1.,1.,1.,1.,1.,1.,1.,1.,1.,1.,1.,1.,
1.,1.,1.,1.,1.,1.))
REPRESENTATION_ITEM('')
);
#258=(
BOUNDED_CURVE()
B_SPLINE_CURVE(5,(#42212,#42213,#42214,#42215,#42216,#42217,#42218,#42219,
#42220,#42221,#42222,#42223,#42224,#42225,#42226,#42227,#42228,#42229,#42230,
#42231,#42232,#42233,#42234,#42235,#42236,#42237,#42238,#42239,#42240,#42241,
#42242,#42243,#42244,#42245,#42246,#42247,#42248,#42249,#42250,#42251,#42252,
#42253,#42254,#42255,#42256,#42257,#42258,#42259,#42260,#42261,#42262,#42263,
#42264,#42265,#42266,#42267,#42268,#42269,#42270,#42271,#42272,#42273,#42274,
#42275,#42276,#42277,#42278,#42279,#42280,#42281),.UNSPECIFIED.,.F.,.F.)
B_SPLINE_CURVE_WITH_KNOTS((6,1,1,1,1,1,1,1,1,1,1,1,1,1,1,1,1,1,1,1,1,1,
1,1,1,1,1,1,1,1,1,1,1,1,1,1,1,1,1,1,1,1,1,1,1,1,1,1,1,1,1,1,1,1,1,1,1,1,
1,1,1,1,1,1,1,6),(0.,0.0153846153846154,0.0307692307692308,0.0461538461538462,
0.0615384615384615,0.0769230769230769,0.0923076923076923,0.107692307692308,
0.123076923076923,0.138461538461538,0.153846153846154,0.169230769230769,
0.184615384615385,0.2,0.215384615384615,0.230769230769231,0.246153846153846,
0.261538461538462,0.276923076923077,0.292307692307692,0.307692307692308,
0.323076923076923,0.338461538461538,0.353846153846154,0.369230769230769,
0.384615384615385,0.4,0.415384615384615,0.430769230769231,0.446153846153846,
0.461538461538462,0.476923076923077,0.492307692307692,0.507692307692308,
0.523076923076923,0.538461538461538,0.553846153846154,0.569230769230769,
0.584615384615384,0.6,0.615384615384615,0.63076923076923,0.646153846153846,
0.661538461538461,0.676923076923076,0.692307692307692,0.707692307692307,
0.723076923076922,0.738461538461538,0.753846153846153,0.769230769230768,
0.784615384615384,0.799999999999999,0.815384615384614,0.83076923076923,
0.846153846153845,0.86153846153846,0.876923076923076,0.892307692307691,
0.907692307692306,0.923076923076922,0.938461538461537,0.953846153846152,
0.969230769230768,0.984615384615383,0.994228156739699),.UNSPECIFIED.)
CURVE()
GEOMETRIC_REPRESENTATION_ITEM()
RATIONAL_B_SPLINE_CURVE((1.,1.,1.,1.,1.,1.,1.,1.,1.,1.,1.,1.,1.,1.,1.,1.,
1.,1.,1.,1.,1.,1.,1.,1.,1.,1.,1.,1.,1.,1.,1.,1.,1.,1.,1.,1.,1.,1.,1.,1.,
1.,1.,1.,1.,1.,1.,1.,1.,1.,1.,1.,1.,1.,1.,1.,1.,1.,1.,1.,1.,1.,1.,1.,1.,
1.,1.,1.,1.,1.,1.))
REPRESENTATION_ITEM('')
);
#259=(
BOUNDED_CURVE()
B_SPLINE_CURVE(5,(#42285,#42286,#42287,#42288,#42289,#42290,#42291,#42292,
#42293,#42294,#42295,#42296,#42297,#42298,#42299,#42300,#42301,#42302,#42303,
#42304,#42305,#42306,#42307,#42308,#42309,#42310,#42311,#42312,#42313,#42314,
#42315,#42316,#42317,#42318,#42319,#42320,#42321,#42322,#42323,#42324,#42325,
#42326,#42327,#42328,#42329,#42330,#42331,#42332,#42333,#42334,#42335,#42336,
#42337,#42338,#42339,#42340,#42341,#42342,#42343,#42344,#42345,#42346,#42347,
#42348,#42349,#42350,#42351,#42352,#42353,#42354),.UNSPECIFIED.,.F.,.F.)
B_SPLINE_CURVE_WITH_KNOTS((6,1,1,1,1,1,1,1,1,1,1,1,1,1,1,1,1,1,1,1,1,1,
1,1,1,1,1,1,1,1,1,1,1,1,1,1,1,1,1,1,1,1,1,1,1,1,1,1,1,1,1,1,1,1,1,1,1,1,
1,1,1,1,1,1,1,6),(0.00577184337448657,0.0153846153846154,0.0307692307692308,
0.0461538461538462,0.0615384615384615,0.0769230769230769,0.0923076923076923,
0.107692307692308,0.123076923076923,0.138461538461538,0.153846153846154,
0.169230769230769,0.184615384615385,0.2,0.215384615384615,0.230769230769231,
0.246153846153846,0.261538461538462,0.276923076923077,0.292307692307692,
0.307692307692308,0.323076923076923,0.338461538461538,0.353846153846154,
0.369230769230769,0.384615384615385,0.4,0.415384615384615,0.430769230769231,
0.446153846153846,0.461538461538462,0.476923076923077,0.492307692307692,
0.507692307692308,0.523076923076923,0.538461538461538,0.553846153846154,
0.569230769230769,0.584615384615384,0.6,0.615384615384615,0.63076923076923,
0.646153846153846,0.661538461538461,0.676923076923076,0.692307692307692,
0.707692307692307,0.723076923076922,0.738461538461538,0.753846153846153,
0.769230769230768,0.784615384615384,0.799999999999999,0.815384615384614,
0.83076923076923,0.846153846153845,0.86153846153846,0.876923076923076,0.892307692307691,
0.907692307692306,0.923076923076922,0.938461538461537,0.953846153846152,
0.969230769230768,0.984615384615383,1.),.UNSPECIFIED.)
CURVE()
GEOMETRIC_REPRESENTATION_ITEM()
RATIONAL_B_SPLINE_CURVE((1.,1.,1.,1.,1.,1.,1.,1.,1.,1.,1.,1.,1.,1.,1.,1.,
1.,1.,1.,1.,1.,1.,1.,1.,1.,1.,1.,1.,1.,1.,1.,1.,1.,1.,1.,1.,1.,1.,1.,1.,
1.,1.,1.,1.,1.,1.,1.,1.,1.,1.,1.,1.,1.,1.,1.,1.,1.,1.,1.,1.,1.,1.,1.,1.,
1.,1.,1.,1.,1.,1.))
REPRESENTATION_ITEM('')
);
#260=(
BOUNDED_CURVE()
B_SPLINE_CURVE(5,(#42358,#42359,#42360,#42361,#42362,#42363,#42364,#42365,
#42366,#42367,#42368,#42369,#42370,#42371,#42372,#42373,#42374,#42375,#42376,
#42377,#42378,#42379,#42380,#42381,#42382,#42383,#42384,#42385,#42386,#42387,
#42388,#42389,#42390,#42391,#42392,#42393,#42394,#42395,#42396,#42397,#42398,
#42399,#42400,#42401,#42402,#42403,#42404,#42405,#42406,#42407,#42408,#42409,
#42410,#42411,#42412,#42413,#42414,#42415,#42416,#42417,#42418,#42419,#42420,
#42421,#42422,#42423,#42424,#42425,#42426,#42427),.UNSPECIFIED.,.F.,.F.)
B_SPLINE_CURVE_WITH_KNOTS((6,1,1,1,1,1,1,1,1,1,1,1,1,1,1,1,1,1,1,1,1,1,
1,1,1,1,1,1,1,1,1,1,1,1,1,1,1,1,1,1,1,1,1,1,1,1,1,1,1,1,1,1,1,1,1,1,1,1,
1,1,1,1,1,1,1,6),(0.,0.0153846153846154,0.0307692307692308,0.0461538461538462,
0.0615384615384615,0.0769230769230769,0.0923076923076923,0.107692307692308,
0.123076923076923,0.138461538461538,0.153846153846154,0.169230769230769,
0.184615384615385,0.2,0.215384615384615,0.230769230769231,0.246153846153846,
0.261538461538462,0.276923076923077,0.292307692307692,0.307692307692308,
0.323076923076923,0.338461538461538,0.353846153846154,0.369230769230769,
0.384615384615385,0.4,0.415384615384615,0.430769230769231,0.446153846153846,
0.461538461538462,0.476923076923077,0.492307692307692,0.507692307692308,
0.523076923076923,0.538461538461538,0.553846153846154,0.569230769230769,
0.584615384615384,0.6,0.615384615384615,0.63076923076923,0.646153846153846,
0.661538461538461,0.676923076923076,0.692307692307692,0.707692307692307,
0.723076923076922,0.738461538461538,0.753846153846153,0.769230769230768,
0.784615384615384,0.799999999999999,0.815384615384614,0.83076923076923,
0.846153846153845,0.86153846153846,0.876923076923076,0.892307692307691,
0.907692307692306,0.923076923076922,0.938461538461537,0.953846153846152,
0.969230769230768,0.984615384615383,0.994228156739709),.UNSPECIFIED.)
CURVE()
GEOMETRIC_REPRESENTATION_ITEM()
RATIONAL_B_SPLINE_CURVE((1.,1.,1.,1.,1.,1.,1.,1.,1.,1.,1.,1.,1.,1.,1.,1.,
1.,1.,1.,1.,1.,1.,1.,1.,1.,1.,1.,1.,1.,1.,1.,1.,1.,1.,1.,1.,1.,1.,1.,1.,
1.,1.,1.,1.,1.,1.,1.,1.,1.,1.,1.,1.,1.,1.,1.,1.,1.,1.,1.,1.,1.,1.,1.,1.,
1.,1.,1.,1.,1.,1.))
REPRESENTATION_ITEM('')
);
#261=(
BOUNDED_CURVE()
B_SPLINE_CURVE(5,(#42431,#42432,#42433,#42434,#42435,#42436,#42437,#42438,
#42439,#42440,#42441,#42442,#42443,#42444,#42445,#42446,#42447,#42448,#42449,
#42450,#42451,#42452,#42453,#42454,#42455,#42456,#42457,#42458,#42459,#42460,
#42461,#42462,#42463,#42464,#42465,#42466,#42467,#42468,#42469,#42470,#42471,
#42472,#42473,#42474,#42475,#42476,#42477,#42478,#42479,#42480,#42481,#42482,
#42483,#42484,#42485,#42486,#42487,#42488,#42489,#42490,#42491,#42492,#42493,
#42494,#42495,#42496,#42497,#42498,#42499,#42500),.UNSPECIFIED.,.F.,.F.)
B_SPLINE_CURVE_WITH_KNOTS((6,1,1,1,1,1,1,1,1,1,1,1,1,1,1,1,1,1,1,1,1,1,
1,1,1,1,1,1,1,1,1,1,1,1,1,1,1,1,1,1,1,1,1,1,1,1,1,1,1,1,1,1,1,1,1,1,1,1,
1,1,1,1,1,1,1,6),(0.00577184337451132,0.0153846153846154,0.0307692307692308,
0.0461538461538462,0.0615384615384615,0.0769230769230769,0.0923076923076923,
0.107692307692308,0.123076923076923,0.138461538461538,0.153846153846154,
0.169230769230769,0.184615384615385,0.2,0.215384615384615,0.230769230769231,
0.246153846153846,0.261538461538462,0.276923076923077,0.292307692307692,
0.307692307692308,0.323076923076923,0.338461538461538,0.353846153846154,
0.369230769230769,0.384615384615385,0.4,0.415384615384615,0.430769230769231,
0.446153846153846,0.461538461538462,0.476923076923077,0.492307692307692,
0.507692307692308,0.523076923076923,0.538461538461538,0.553846153846154,
0.569230769230769,0.584615384615384,0.6,0.615384615384615,0.63076923076923,
0.646153846153846,0.661538461538461,0.676923076923076,0.692307692307692,
0.707692307692307,0.723076923076922,0.738461538461538,0.753846153846153,
0.769230769230768,0.784615384615384,0.799999999999999,0.815384615384614,
0.83076923076923,0.846153846153845,0.86153846153846,0.876923076923076,0.892307692307691,
0.907692307692306,0.923076923076922,0.938461538461537,0.953846153846152,
0.969230769230768,0.984615384615383,1.),.UNSPECIFIED.)
CURVE()
GEOMETRIC_REPRESENTATION_ITEM()
RATIONAL_B_SPLINE_CURVE((1.,1.,1.,1.,1.,1.,1.,1.,1.,1.,1.,1.,1.,1.,1.,1.,
1.,1.,1.,1.,1.,1.,1.,1.,1.,1.,1.,1.,1.,1.,1.,1.,1.,1.,1.,1.,1.,1.,1.,1.,
1.,1.,1.,1.,1.,1.,1.,1.,1.,1.,1.,1.,1.,1.,1.,1.,1.,1.,1.,1.,1.,1.,1.,1.,
1.,1.,1.,1.,1.,1.))
REPRESENTATION_ITEM('')
);
#262=(
BOUNDED_CURVE()
B_SPLINE_CURVE(5,(#42504,#42505,#42506,#42507,#42508,#42509,#42510,#42511,
#42512,#42513,#42514,#42515,#42516,#42517,#42518,#42519,#42520,#42521,#42522,
#42523,#42524,#42525,#42526,#42527,#42528,#42529,#42530,#42531,#42532,#42533,
#42534,#42535,#42536,#42537,#42538,#42539,#42540,#42541,#42542,#42543,#42544,
#42545,#42546,#42547,#42548,#42549,#42550,#42551,#42552,#42553,#42554,#42555,
#42556,#42557,#42558,#42559,#42560,#42561,#42562,#42563,#42564,#42565,#42566,
#42567,#42568,#42569,#42570,#42571,#42572,#42573),.UNSPECIFIED.,.F.,.F.)
B_SPLINE_CURVE_WITH_KNOTS((6,1,1,1,1,1,1,1,1,1,1,1,1,1,1,1,1,1,1,1,1,1,
1,1,1,1,1,1,1,1,1,1,1,1,1,1,1,1,1,1,1,1,1,1,1,1,1,1,1,1,1,1,1,1,1,1,1,1,
1,1,1,1,1,1,1,6),(0.,0.0153846153846154,0.0307692307692308,0.0461538461538462,
0.0615384615384615,0.0769230769230769,0.0923076923076923,0.107692307692308,
0.123076923076923,0.138461538461538,0.153846153846154,0.169230769230769,
0.184615384615385,0.2,0.215384615384615,0.230769230769231,0.246153846153846,
0.261538461538462,0.276923076923077,0.292307692307692,0.307692307692308,
0.323076923076923,0.338461538461538,0.353846153846154,0.369230769230769,
0.384615384615385,0.4,0.415384615384615,0.430769230769231,0.446153846153846,
0.461538461538462,0.476923076923077,0.492307692307692,0.507692307692308,
0.523076923076923,0.538461538461538,0.553846153846154,0.569230769230769,
0.584615384615384,0.6,0.615384615384615,0.63076923076923,0.646153846153846,
0.661538461538461,0.676923076923076,0.692307692307692,0.707692307692307,
0.723076923076922,0.738461538461538,0.753846153846153,0.769230769230768,
0.784615384615384,0.799999999999999,0.815384615384614,0.83076923076923,
0.846153846153845,0.86153846153846,0.876923076923076,0.892307692307691,
0.907692307692306,0.923076923076922,0.938461538461537,0.953846153846152,
0.969230769230768,0.984615384615383,0.994228156739705),.UNSPECIFIED.)
CURVE()
GEOMETRIC_REPRESENTATION_ITEM()
RATIONAL_B_SPLINE_CURVE((1.,1.,1.,1.,1.,1.,1.,1.,1.,1.,1.,1.,1.,1.,1.,1.,
1.,1.,1.,1.,1.,1.,1.,1.,1.,1.,1.,1.,1.,1.,1.,1.,1.,1.,1.,1.,1.,1.,1.,1.,
1.,1.,1.,1.,1.,1.,1.,1.,1.,1.,1.,1.,1.,1.,1.,1.,1.,1.,1.,1.,1.,1.,1.,1.,
1.,1.,1.,1.,1.,1.))
REPRESENTATION_ITEM('')
);
#263=(
BOUNDED_CURVE()
B_SPLINE_CURVE(5,(#42577,#42578,#42579,#42580,#42581,#42582,#42583,#42584,
#42585,#42586,#42587,#42588,#42589,#42590,#42591,#42592,#42593,#42594,#42595,
#42596,#42597,#42598,#42599,#42600,#42601,#42602,#42603,#42604,#42605,#42606,
#42607,#42608,#42609,#42610,#42611,#42612,#42613,#42614,#42615,#42616,#42617,
#42618,#42619,#42620,#42621,#42622,#42623,#42624,#42625,#42626,#42627,#42628,
#42629,#42630,#42631,#42632,#42633,#42634,#42635,#42636,#42637,#42638,#42639,
#42640,#42641,#42642,#42643,#42644,#42645,#42646),.UNSPECIFIED.,.F.,.F.)
B_SPLINE_CURVE_WITH_KNOTS((6,1,1,1,1,1,1,1,1,1,1,1,1,1,1,1,1,1,1,1,1,1,
1,1,1,1,1,1,1,1,1,1,1,1,1,1,1,1,1,1,1,1,1,1,1,1,1,1,1,1,1,1,1,1,1,1,1,1,
1,1,1,1,1,1,1,6),(0.00577184337450072,0.0153846153846154,0.0307692307692308,
0.0461538461538462,0.0615384615384615,0.0769230769230769,0.0923076923076923,
0.107692307692308,0.123076923076923,0.138461538461538,0.153846153846154,
0.169230769230769,0.184615384615385,0.2,0.215384615384615,0.230769230769231,
0.246153846153846,0.261538461538462,0.276923076923077,0.292307692307692,
0.307692307692308,0.323076923076923,0.338461538461538,0.353846153846154,
0.369230769230769,0.384615384615385,0.4,0.415384615384615,0.430769230769231,
0.446153846153846,0.461538461538462,0.476923076923077,0.492307692307692,
0.507692307692308,0.523076923076923,0.538461538461538,0.553846153846154,
0.569230769230769,0.584615384615384,0.6,0.615384615384615,0.63076923076923,
0.646153846153846,0.661538461538461,0.676923076923076,0.692307692307692,
0.707692307692307,0.723076923076922,0.738461538461538,0.753846153846153,
0.769230769230768,0.784615384615384,0.799999999999999,0.815384615384614,
0.83076923076923,0.846153846153845,0.86153846153846,0.876923076923076,0.892307692307691,
0.907692307692306,0.923076923076922,0.938461538461537,0.953846153846152,
0.969230769230768,0.984615384615383,1.),.UNSPECIFIED.)
CURVE()
GEOMETRIC_REPRESENTATION_ITEM()
RATIONAL_B_SPLINE_CURVE((1.,1.,1.,1.,1.,1.,1.,1.,1.,1.,1.,1.,1.,1.,1.,1.,
1.,1.,1.,1.,1.,1.,1.,1.,1.,1.,1.,1.,1.,1.,1.,1.,1.,1.,1.,1.,1.,1.,1.,1.,
1.,1.,1.,1.,1.,1.,1.,1.,1.,1.,1.,1.,1.,1.,1.,1.,1.,1.,1.,1.,1.,1.,1.,1.,
1.,1.,1.,1.,1.,1.))
REPRESENTATION_ITEM('')
);
#264=(
BOUNDED_CURVE()
B_SPLINE_CURVE(5,(#42650,#42651,#42652,#42653,#42654,#42655,#42656,#42657,
#42658,#42659,#42660,#42661,#42662,#42663,#42664,#42665,#42666,#42667,#42668,
#42669,#42670,#42671,#42672,#42673,#42674,#42675,#42676,#42677,#42678,#42679,
#42680,#42681,#42682,#42683,#42684,#42685,#42686,#42687,#42688,#42689,#42690,
#42691,#42692,#42693,#42694,#42695,#42696,#42697,#42698,#42699,#42700,#42701,
#42702,#42703,#42704,#42705,#42706,#42707,#42708,#42709,#42710,#42711,#42712,
#42713,#42714,#42715,#42716,#42717,#42718,#42719),.UNSPECIFIED.,.F.,.F.)
B_SPLINE_CURVE_WITH_KNOTS((6,1,1,1,1,1,1,1,1,1,1,1,1,1,1,1,1,1,1,1,1,1,
1,1,1,1,1,1,1,1,1,1,1,1,1,1,1,1,1,1,1,1,1,1,1,1,1,1,1,1,1,1,1,1,1,1,1,1,
1,1,1,1,1,1,1,6),(0.,0.0153846153846154,0.0307692307692308,0.0461538461538462,
0.0615384615384615,0.0769230769230769,0.0923076923076923,0.107692307692308,
0.123076923076923,0.138461538461538,0.153846153846154,0.169230769230769,
0.184615384615385,0.2,0.215384615384615,0.230769230769231,0.246153846153846,
0.261538461538462,0.276923076923077,0.292307692307692,0.307692307692308,
0.323076923076923,0.338461538461538,0.353846153846154,0.369230769230769,
0.384615384615385,0.4,0.415384615384615,0.430769230769231,0.446153846153846,
0.461538461538462,0.476923076923077,0.492307692307692,0.507692307692308,
0.523076923076923,0.538461538461538,0.553846153846154,0.569230769230769,
0.584615384615384,0.6,0.615384615384615,0.63076923076923,0.646153846153846,
0.661538461538461,0.676923076923076,0.692307692307692,0.707692307692307,
0.723076923076922,0.738461538461538,0.753846153846153,0.769230769230768,
0.784615384615384,0.799999999999999,0.815384615384614,0.83076923076923,
0.846153846153845,0.86153846153846,0.876923076923076,0.892307692307691,
0.907692307692306,0.923076923076922,0.938461538461537,0.953846153846152,
0.969230769230768,0.984615384615383,0.994228156739706),.UNSPECIFIED.)
CURVE()
GEOMETRIC_REPRESENTATION_ITEM()
RATIONAL_B_SPLINE_CURVE((1.,1.,1.,1.,1.,1.,1.,1.,1.,1.,1.,1.,1.,1.,1.,1.,
1.,1.,1.,1.,1.,1.,1.,1.,1.,1.,1.,1.,1.,1.,1.,1.,1.,1.,1.,1.,1.,1.,1.,1.,
1.,1.,1.,1.,1.,1.,1.,1.,1.,1.,1.,1.,1.,1.,1.,1.,1.,1.,1.,1.,1.,1.,1.,1.,
1.,1.,1.,1.,1.,1.))
REPRESENTATION_ITEM('')
);
#265=(
BOUNDED_CURVE()
B_SPLINE_CURVE(5,(#42723,#42724,#42725,#42726,#42727,#42728,#42729,#42730,
#42731,#42732,#42733,#42734,#42735,#42736,#42737,#42738,#42739,#42740,#42741,
#42742,#42743,#42744,#42745,#42746,#42747,#42748,#42749,#42750,#42751,#42752,
#42753,#42754,#42755,#42756,#42757,#42758,#42759,#42760,#42761,#42762,#42763,
#42764,#42765,#42766,#42767,#42768,#42769,#42770,#42771,#42772,#42773,#42774,
#42775,#42776,#42777,#42778,#42779,#42780,#42781,#42782,#42783,#42784,#42785,
#42786,#42787,#42788,#42789,#42790,#42791,#42792),.UNSPECIFIED.,.F.,.F.)
B_SPLINE_CURVE_WITH_KNOTS((6,1,1,1,1,1,1,1,1,1,1,1,1,1,1,1,1,1,1,1,1,1,
1,1,1,1,1,1,1,1,1,1,1,1,1,1,1,1,1,1,1,1,1,1,1,1,1,1,1,1,1,1,1,1,1,1,1,1,
1,1,1,1,1,1,1,6),(0.00577184337450902,0.0153846153846154,0.0307692307692308,
0.0461538461538462,0.0615384615384615,0.0769230769230769,0.0923076923076923,
0.107692307692308,0.123076923076923,0.138461538461538,0.153846153846154,
0.169230769230769,0.184615384615385,0.2,0.215384615384615,0.230769230769231,
0.246153846153846,0.261538461538462,0.276923076923077,0.292307692307692,
0.307692307692308,0.323076923076923,0.338461538461538,0.353846153846154,
0.369230769230769,0.384615384615385,0.4,0.415384615384615,0.430769230769231,
0.446153846153846,0.461538461538462,0.476923076923077,0.492307692307692,
0.507692307692308,0.523076923076923,0.538461538461538,0.553846153846154,
0.569230769230769,0.584615384615384,0.6,0.615384615384615,0.63076923076923,
0.646153846153846,0.661538461538461,0.676923076923076,0.692307692307692,
0.707692307692307,0.723076923076922,0.738461538461538,0.753846153846153,
0.769230769230768,0.784615384615384,0.799999999999999,0.815384615384614,
0.83076923076923,0.846153846153845,0.86153846153846,0.876923076923076,0.892307692307691,
0.907692307692306,0.923076923076922,0.938461538461537,0.953846153846152,
0.969230769230768,0.984615384615383,1.),.UNSPECIFIED.)
CURVE()
GEOMETRIC_REPRESENTATION_ITEM()
RATIONAL_B_SPLINE_CURVE((1.,1.,1.,1.,1.,1.,1.,1.,1.,1.,1.,1.,1.,1.,1.,1.,
1.,1.,1.,1.,1.,1.,1.,1.,1.,1.,1.,1.,1.,1.,1.,1.,1.,1.,1.,1.,1.,1.,1.,1.,
1.,1.,1.,1.,1.,1.,1.,1.,1.,1.,1.,1.,1.,1.,1.,1.,1.,1.,1.,1.,1.,1.,1.,1.,
1.,1.,1.,1.,1.,1.))
REPRESENTATION_ITEM('')
);
#266=(
BOUNDED_CURVE()
B_SPLINE_CURVE(5,(#42796,#42797,#42798,#42799,#42800,#42801,#42802,#42803,
#42804,#42805,#42806,#42807,#42808,#42809,#42810,#42811,#42812,#42813,#42814,
#42815,#42816,#42817,#42818,#42819,#42820,#42821,#42822,#42823,#42824,#42825,
#42826,#42827,#42828,#42829,#42830,#42831,#42832,#42833,#42834,#42835,#42836,
#42837,#42838,#42839,#42840,#42841,#42842,#42843,#42844,#42845,#42846,#42847,
#42848,#42849,#42850,#42851,#42852,#42853,#42854,#42855,#42856,#42857,#42858,
#42859,#42860,#42861,#42862,#42863,#42864,#42865),.UNSPECIFIED.,.F.,.F.)
B_SPLINE_CURVE_WITH_KNOTS((6,1,1,1,1,1,1,1,1,1,1,1,1,1,1,1,1,1,1,1,1,1,
1,1,1,1,1,1,1,1,1,1,1,1,1,1,1,1,1,1,1,1,1,1,1,1,1,1,1,1,1,1,1,1,1,1,1,1,
1,1,1,1,1,1,1,6),(0.,0.0153846153846154,0.0307692307692308,0.0461538461538462,
0.0615384615384615,0.0769230769230769,0.0923076923076923,0.107692307692308,
0.123076923076923,0.138461538461538,0.153846153846154,0.169230769230769,
0.184615384615385,0.2,0.215384615384615,0.230769230769231,0.246153846153846,
0.261538461538462,0.276923076923077,0.292307692307692,0.307692307692308,
0.323076923076923,0.338461538461538,0.353846153846154,0.369230769230769,
0.384615384615385,0.4,0.415384615384615,0.430769230769231,0.446153846153846,
0.461538461538462,0.476923076923077,0.492307692307692,0.507692307692308,
0.523076923076923,0.538461538461538,0.553846153846154,0.569230769230769,
0.584615384615384,0.6,0.615384615384615,0.63076923076923,0.646153846153846,
0.661538461538461,0.676923076923076,0.692307692307692,0.707692307692307,
0.723076923076922,0.738461538461538,0.753846153846153,0.769230769230768,
0.784615384615384,0.799999999999999,0.815384615384614,0.83076923076923,
0.846153846153845,0.86153846153846,0.876923076923076,0.892307692307691,
0.907692307692306,0.923076923076922,0.938461538461537,0.953846153846152,
0.969230769230768,0.984615384615383,0.994228156739698),.UNSPECIFIED.)
CURVE()
GEOMETRIC_REPRESENTATION_ITEM()
RATIONAL_B_SPLINE_CURVE((1.,1.,1.,1.,1.,1.,1.,1.,1.,1.,1.,1.,1.,1.,1.,1.,
1.,1.,1.,1.,1.,1.,1.,1.,1.,1.,1.,1.,1.,1.,1.,1.,1.,1.,1.,1.,1.,1.,1.,1.,
1.,1.,1.,1.,1.,1.,1.,1.,1.,1.,1.,1.,1.,1.,1.,1.,1.,1.,1.,1.,1.,1.,1.,1.,
1.,1.,1.,1.,1.,1.))
REPRESENTATION_ITEM('')
);
#267=(
BOUNDED_CURVE()
B_SPLINE_CURVE(5,(#42869,#42870,#42871,#42872,#42873,#42874,#42875,#42876,
#42877,#42878,#42879,#42880,#42881,#42882,#42883,#42884,#42885,#42886,#42887,
#42888,#42889,#42890,#42891,#42892,#42893,#42894,#42895,#42896,#42897,#42898,
#42899,#42900,#42901,#42902,#42903,#42904,#42905,#42906,#42907,#42908,#42909,
#42910,#42911,#42912,#42913,#42914,#42915,#42916,#42917,#42918,#42919,#42920,
#42921,#42922,#42923,#42924,#42925,#42926,#42927,#42928,#42929,#42930,#42931,
#42932,#42933,#42934,#42935,#42936,#42937,#42938),.UNSPECIFIED.,.F.,.F.)
B_SPLINE_CURVE_WITH_KNOTS((6,1,1,1,1,1,1,1,1,1,1,1,1,1,1,1,1,1,1,1,1,1,
1,1,1,1,1,1,1,1,1,1,1,1,1,1,1,1,1,1,1,1,1,1,1,1,1,1,1,1,1,1,1,1,1,1,1,1,
1,1,1,1,1,1,1,6),(0.00577184337451611,0.0153846153846154,0.0307692307692308,
0.0461538461538462,0.0615384615384615,0.0769230769230769,0.0923076923076923,
0.107692307692308,0.123076923076923,0.138461538461538,0.153846153846154,
0.169230769230769,0.184615384615385,0.2,0.215384615384615,0.230769230769231,
0.246153846153846,0.261538461538462,0.276923076923077,0.292307692307692,
0.307692307692308,0.323076923076923,0.338461538461538,0.353846153846154,
0.369230769230769,0.384615384615385,0.4,0.415384615384615,0.430769230769231,
0.446153846153846,0.461538461538462,0.476923076923077,0.492307692307692,
0.507692307692308,0.523076923076923,0.538461538461538,0.553846153846154,
0.569230769230769,0.584615384615384,0.6,0.615384615384615,0.63076923076923,
0.646153846153846,0.661538461538461,0.676923076923076,0.692307692307692,
0.707692307692307,0.723076923076922,0.738461538461538,0.753846153846153,
0.769230769230768,0.784615384615384,0.799999999999999,0.815384615384614,
0.83076923076923,0.846153846153845,0.86153846153846,0.876923076923076,0.892307692307691,
0.907692307692306,0.923076923076922,0.938461538461537,0.953846153846152,
0.969230769230768,0.984615384615383,1.),.UNSPECIFIED.)
CURVE()
GEOMETRIC_REPRESENTATION_ITEM()
RATIONAL_B_SPLINE_CURVE((1.,1.,1.,1.,1.,1.,1.,1.,1.,1.,1.,1.,1.,1.,1.,1.,
1.,1.,1.,1.,1.,1.,1.,1.,1.,1.,1.,1.,1.,1.,1.,1.,1.,1.,1.,1.,1.,1.,1.,1.,
1.,1.,1.,1.,1.,1.,1.,1.,1.,1.,1.,1.,1.,1.,1.,1.,1.,1.,1.,1.,1.,1.,1.,1.,
1.,1.,1.,1.,1.,1.))
REPRESENTATION_ITEM('')
);
#268=(
BOUNDED_CURVE()
B_SPLINE_CURVE(5,(#42942,#42943,#42944,#42945,#42946,#42947,#42948,#42949,
#42950,#42951,#42952,#42953,#42954,#42955,#42956,#42957,#42958,#42959,#42960,
#42961,#42962,#42963,#42964,#42965,#42966,#42967,#42968,#42969,#42970,#42971,
#42972,#42973,#42974,#42975,#42976,#42977,#42978,#42979,#42980,#42981,#42982,
#42983,#42984,#42985,#42986,#42987,#42988,#42989,#42990,#42991,#42992,#42993,
#42994,#42995,#42996,#42997,#42998,#42999,#43000,#43001,#43002,#43003,#43004,
#43005,#43006,#43007,#43008,#43009,#43010,#43011),.UNSPECIFIED.,.F.,.F.)
B_SPLINE_CURVE_WITH_KNOTS((6,1,1,1,1,1,1,1,1,1,1,1,1,1,1,1,1,1,1,1,1,1,
1,1,1,1,1,1,1,1,1,1,1,1,1,1,1,1,1,1,1,1,1,1,1,1,1,1,1,1,1,1,1,1,1,1,1,1,
1,1,1,1,1,1,1,6),(0.,0.0153846153846154,0.0307692307692308,0.0461538461538462,
0.0615384615384615,0.0769230769230769,0.0923076923076923,0.107692307692308,
0.123076923076923,0.138461538461538,0.153846153846154,0.169230769230769,
0.184615384615385,0.2,0.215384615384615,0.230769230769231,0.246153846153846,
0.261538461538462,0.276923076923077,0.292307692307692,0.307692307692308,
0.323076923076923,0.338461538461538,0.353846153846154,0.369230769230769,
0.384615384615385,0.4,0.415384615384615,0.430769230769231,0.446153846153846,
0.461538461538462,0.476923076923077,0.492307692307692,0.507692307692308,
0.523076923076923,0.538461538461538,0.553846153846154,0.569230769230769,
0.584615384615384,0.6,0.615384615384615,0.63076923076923,0.646153846153846,
0.661538461538461,0.676923076923076,0.692307692307692,0.707692307692307,
0.723076923076922,0.738461538461538,0.753846153846153,0.769230769230768,
0.784615384615384,0.799999999999999,0.815384615384614,0.83076923076923,
0.846153846153845,0.86153846153846,0.876923076923076,0.892307692307691,
0.907692307692306,0.923076923076922,0.938461538461537,0.953846153846152,
0.969230769230768,0.984615384615383,0.994228156739704),.UNSPECIFIED.)
CURVE()
GEOMETRIC_REPRESENTATION_ITEM()
RATIONAL_B_SPLINE_CURVE((1.,1.,1.,1.,1.,1.,1.,1.,1.,1.,1.,1.,1.,1.,1.,1.,
1.,1.,1.,1.,1.,1.,1.,1.,1.,1.,1.,1.,1.,1.,1.,1.,1.,1.,1.,1.,1.,1.,1.,1.,
1.,1.,1.,1.,1.,1.,1.,1.,1.,1.,1.,1.,1.,1.,1.,1.,1.,1.,1.,1.,1.,1.,1.,1.,
1.,1.,1.,1.,1.,1.))
REPRESENTATION_ITEM('')
);
#269=(
BOUNDED_CURVE()
B_SPLINE_CURVE(5,(#43015,#43016,#43017,#43018,#43019,#43020,#43021,#43022,
#43023,#43024,#43025,#43026,#43027,#43028,#43029,#43030,#43031,#43032,#43033,
#43034,#43035,#43036,#43037,#43038,#43039,#43040,#43041,#43042,#43043,#43044,
#43045,#43046,#43047,#43048,#43049,#43050,#43051,#43052,#43053,#43054,#43055,
#43056,#43057,#43058,#43059,#43060,#43061,#43062,#43063,#43064,#43065,#43066,
#43067,#43068,#43069,#43070,#43071,#43072,#43073,#43074,#43075,#43076,#43077,
#43078,#43079,#43080,#43081,#43082,#43083,#43084),.UNSPECIFIED.,.F.,.F.)
B_SPLINE_CURVE_WITH_KNOTS((6,1,1,1,1,1,1,1,1,1,1,1,1,1,1,1,1,1,1,1,1,1,
1,1,1,1,1,1,1,1,1,1,1,1,1,1,1,1,1,1,1,1,1,1,1,1,1,1,1,1,1,1,1,1,1,1,1,1,
1,1,1,1,1,1,1,6),(0.00577184337449682,0.0153846153846154,0.0307692307692308,
0.0461538461538462,0.0615384615384615,0.0769230769230769,0.0923076923076923,
0.107692307692308,0.123076923076923,0.138461538461538,0.153846153846154,
0.169230769230769,0.184615384615385,0.2,0.215384615384615,0.230769230769231,
0.246153846153846,0.261538461538462,0.276923076923077,0.292307692307692,
0.307692307692308,0.323076923076923,0.338461538461538,0.353846153846154,
0.369230769230769,0.384615384615385,0.4,0.415384615384615,0.430769230769231,
0.446153846153846,0.461538461538462,0.476923076923077,0.492307692307692,
0.507692307692308,0.523076923076923,0.538461538461538,0.553846153846154,
0.569230769230769,0.584615384615384,0.6,0.615384615384615,0.63076923076923,
0.646153846153846,0.661538461538461,0.676923076923076,0.692307692307692,
0.707692307692307,0.723076923076922,0.738461538461538,0.753846153846153,
0.769230769230768,0.784615384615384,0.799999999999999,0.815384615384614,
0.83076923076923,0.846153846153845,0.86153846153846,0.876923076923076,0.892307692307691,
0.907692307692306,0.923076923076922,0.938461538461537,0.953846153846152,
0.969230769230768,0.984615384615383,1.),.UNSPECIFIED.)
CURVE()
GEOMETRIC_REPRESENTATION_ITEM()
RATIONAL_B_SPLINE_CURVE((1.,1.,1.,1.,1.,1.,1.,1.,1.,1.,1.,1.,1.,1.,1.,1.,
1.,1.,1.,1.,1.,1.,1.,1.,1.,1.,1.,1.,1.,1.,1.,1.,1.,1.,1.,1.,1.,1.,1.,1.,
1.,1.,1.,1.,1.,1.,1.,1.,1.,1.,1.,1.,1.,1.,1.,1.,1.,1.,1.,1.,1.,1.,1.,1.,
1.,1.,1.,1.,1.,1.))
REPRESENTATION_ITEM('')
);
#270=(
BOUNDED_CURVE()
B_SPLINE_CURVE(5,(#43088,#43089,#43090,#43091,#43092,#43093,#43094,#43095,
#43096,#43097,#43098,#43099,#43100,#43101,#43102,#43103,#43104,#43105,#43106,
#43107,#43108,#43109,#43110,#43111,#43112,#43113,#43114,#43115,#43116,#43117,
#43118,#43119,#43120,#43121,#43122,#43123,#43124,#43125,#43126,#43127,#43128,
#43129,#43130,#43131,#43132,#43133,#43134,#43135,#43136,#43137,#43138,#43139,
#43140,#43141,#43142,#43143,#43144,#43145,#43146,#43147,#43148,#43149,#43150,
#43151,#43152,#43153,#43154,#43155,#43156,#43157),.UNSPECIFIED.,.F.,.F.)
B_SPLINE_CURVE_WITH_KNOTS((6,1,1,1,1,1,1,1,1,1,1,1,1,1,1,1,1,1,1,1,1,1,
1,1,1,1,1,1,1,1,1,1,1,1,1,1,1,1,1,1,1,1,1,1,1,1,1,1,1,1,1,1,1,1,1,1,1,1,
1,1,1,1,1,1,1,6),(0.,0.0153846153846154,0.0307692307692308,0.0461538461538462,
0.0615384615384615,0.0769230769230769,0.0923076923076923,0.107692307692308,
0.123076923076923,0.138461538461538,0.153846153846154,0.169230769230769,
0.184615384615385,0.2,0.215384615384615,0.230769230769231,0.246153846153846,
0.261538461538462,0.276923076923077,0.292307692307692,0.307692307692308,
0.323076923076923,0.338461538461538,0.353846153846154,0.369230769230769,
0.384615384615385,0.4,0.415384615384615,0.430769230769231,0.446153846153846,
0.461538461538462,0.476923076923077,0.492307692307692,0.507692307692308,
0.523076923076923,0.538461538461538,0.553846153846154,0.569230769230769,
0.584615384615384,0.6,0.615384615384615,0.63076923076923,0.646153846153846,
0.661538461538461,0.676923076923076,0.692307692307692,0.707692307692307,
0.723076923076922,0.738461538461538,0.753846153846153,0.769230769230768,
0.784615384615384,0.799999999999999,0.815384615384614,0.83076923076923,
0.846153846153845,0.86153846153846,0.876923076923076,0.892307692307691,
0.907692307692306,0.923076923076922,0.938461538461537,0.953846153846152,
0.969230769230768,0.984615384615383,0.994228156739711),.UNSPECIFIED.)
CURVE()
GEOMETRIC_REPRESENTATION_ITEM()
RATIONAL_B_SPLINE_CURVE((1.,1.,1.,1.,1.,1.,1.,1.,1.,1.,1.,1.,1.,1.,1.,1.,
1.,1.,1.,1.,1.,1.,1.,1.,1.,1.,1.,1.,1.,1.,1.,1.,1.,1.,1.,1.,1.,1.,1.,1.,
1.,1.,1.,1.,1.,1.,1.,1.,1.,1.,1.,1.,1.,1.,1.,1.,1.,1.,1.,1.,1.,1.,1.,1.,
1.,1.,1.,1.,1.,1.))
REPRESENTATION_ITEM('')
);
#271=(
BOUNDED_CURVE()
B_SPLINE_CURVE(5,(#43161,#43162,#43163,#43164,#43165,#43166,#43167,#43168,
#43169,#43170,#43171,#43172,#43173,#43174,#43175,#43176,#43177,#43178,#43179,
#43180,#43181,#43182,#43183,#43184,#43185,#43186,#43187,#43188,#43189,#43190,
#43191,#43192,#43193,#43194,#43195,#43196,#43197,#43198,#43199,#43200,#43201,
#43202,#43203,#43204,#43205,#43206,#43207,#43208,#43209,#43210,#43211,#43212,
#43213,#43214,#43215,#43216,#43217,#43218,#43219,#43220,#43221,#43222,#43223,
#43224,#43225,#43226,#43227,#43228,#43229,#43230),.UNSPECIFIED.,.F.,.F.)
B_SPLINE_CURVE_WITH_KNOTS((6,1,1,1,1,1,1,1,1,1,1,1,1,1,1,1,1,1,1,1,1,1,
1,1,1,1,1,1,1,1,1,1,1,1,1,1,1,1,1,1,1,1,1,1,1,1,1,1,1,1,1,1,1,1,1,1,1,1,
1,1,1,1,1,1,1,6),(0.00577184337449159,0.0153846153846154,0.0307692307692308,
0.0461538461538462,0.0615384615384615,0.0769230769230769,0.0923076923076923,
0.107692307692308,0.123076923076923,0.138461538461538,0.153846153846154,
0.169230769230769,0.184615384615385,0.2,0.215384615384615,0.230769230769231,
0.246153846153846,0.261538461538462,0.276923076923077,0.292307692307692,
0.307692307692308,0.323076923076923,0.338461538461538,0.353846153846154,
0.369230769230769,0.384615384615385,0.4,0.415384615384615,0.430769230769231,
0.446153846153846,0.461538461538462,0.476923076923077,0.492307692307692,
0.507692307692308,0.523076923076923,0.538461538461538,0.553846153846154,
0.569230769230769,0.584615384615384,0.6,0.615384615384615,0.63076923076923,
0.646153846153846,0.661538461538461,0.676923076923076,0.692307692307692,
0.707692307692307,0.723076923076922,0.738461538461538,0.753846153846153,
0.769230769230768,0.784615384615384,0.799999999999999,0.815384615384614,
0.83076923076923,0.846153846153845,0.86153846153846,0.876923076923076,0.892307692307691,
0.907692307692306,0.923076923076922,0.938461538461537,0.953846153846152,
0.969230769230768,0.984615384615383,1.),.UNSPECIFIED.)
CURVE()
GEOMETRIC_REPRESENTATION_ITEM()
RATIONAL_B_SPLINE_CURVE((1.,1.,1.,1.,1.,1.,1.,1.,1.,1.,1.,1.,1.,1.,1.,1.,
1.,1.,1.,1.,1.,1.,1.,1.,1.,1.,1.,1.,1.,1.,1.,1.,1.,1.,1.,1.,1.,1.,1.,1.,
1.,1.,1.,1.,1.,1.,1.,1.,1.,1.,1.,1.,1.,1.,1.,1.,1.,1.,1.,1.,1.,1.,1.,1.,
1.,1.,1.,1.,1.,1.))
REPRESENTATION_ITEM('')
);
#272=(
BOUNDED_CURVE()
B_SPLINE_CURVE(5,(#43234,#43235,#43236,#43237,#43238,#43239,#43240,#43241,
#43242,#43243,#43244,#43245,#43246,#43247,#43248,#43249,#43250,#43251,#43252,
#43253,#43254,#43255,#43256,#43257,#43258,#43259,#43260,#43261,#43262,#43263,
#43264,#43265,#43266,#43267,#43268,#43269,#43270,#43271,#43272,#43273,#43274,
#43275,#43276,#43277,#43278,#43279,#43280,#43281,#43282,#43283,#43284,#43285,
#43286,#43287,#43288,#43289,#43290,#43291,#43292,#43293,#43294,#43295,#43296,
#43297,#43298,#43299,#43300,#43301,#43302,#43303),.UNSPECIFIED.,.F.,.F.)
B_SPLINE_CURVE_WITH_KNOTS((6,1,1,1,1,1,1,1,1,1,1,1,1,1,1,1,1,1,1,1,1,1,
1,1,1,1,1,1,1,1,1,1,1,1,1,1,1,1,1,1,1,1,1,1,1,1,1,1,1,1,1,1,1,1,1,1,1,1,
1,1,1,1,1,1,1,6),(0.,0.0153846153846154,0.0307692307692308,0.0461538461538462,
0.0615384615384615,0.0769230769230769,0.0923076923076923,0.107692307692308,
0.123076923076923,0.138461538461538,0.153846153846154,0.169230769230769,
0.184615384615385,0.2,0.215384615384615,0.230769230769231,0.246153846153846,
0.261538461538462,0.276923076923077,0.292307692307692,0.307692307692308,
0.323076923076923,0.338461538461538,0.353846153846154,0.369230769230769,
0.384615384615385,0.4,0.415384615384615,0.430769230769231,0.446153846153846,
0.461538461538462,0.476923076923077,0.492307692307692,0.507692307692308,
0.523076923076923,0.538461538461538,0.553846153846154,0.569230769230769,
0.584615384615384,0.6,0.615384615384615,0.63076923076923,0.646153846153846,
0.661538461538461,0.676923076923076,0.692307692307692,0.707692307692307,
0.723076923076922,0.738461538461538,0.753846153846153,0.769230769230768,
0.784615384615384,0.799999999999999,0.815384615384614,0.83076923076923,
0.846153846153845,0.86153846153846,0.876923076923076,0.892307692307691,
0.907692307692306,0.923076923076922,0.938461538461537,0.953846153846152,
0.969230769230768,0.984615384615383,0.994228156739723),.UNSPECIFIED.)
CURVE()
GEOMETRIC_REPRESENTATION_ITEM()
RATIONAL_B_SPLINE_CURVE((1.,1.,1.,1.,1.,1.,1.,1.,1.,1.,1.,1.,1.,1.,1.,1.,
1.,1.,1.,1.,1.,1.,1.,1.,1.,1.,1.,1.,1.,1.,1.,1.,1.,1.,1.,1.,1.,1.,1.,1.,
1.,1.,1.,1.,1.,1.,1.,1.,1.,1.,1.,1.,1.,1.,1.,1.,1.,1.,1.,1.,1.,1.,1.,1.,
1.,1.,1.,1.,1.,1.))
REPRESENTATION_ITEM('')
);
#273=(
BOUNDED_CURVE()
B_SPLINE_CURVE(5,(#43307,#43308,#43309,#43310,#43311,#43312,#43313,#43314,
#43315,#43316,#43317,#43318,#43319,#43320,#43321,#43322,#43323,#43324,#43325,
#43326,#43327,#43328,#43329,#43330,#43331,#43332,#43333,#43334,#43335,#43336,
#43337,#43338,#43339,#43340,#43341,#43342,#43343,#43344,#43345,#43346,#43347,
#43348,#43349,#43350,#43351,#43352,#43353,#43354,#43355,#43356,#43357,#43358,
#43359,#43360,#43361,#43362,#43363,#43364,#43365,#43366,#43367,#43368,#43369,
#43370,#43371,#43372,#43373,#43374,#43375,#43376),.UNSPECIFIED.,.F.,.F.)
B_SPLINE_CURVE_WITH_KNOTS((6,1,1,1,1,1,1,1,1,1,1,1,1,1,1,1,1,1,1,1,1,1,
1,1,1,1,1,1,1,1,1,1,1,1,1,1,1,1,1,1,1,1,1,1,1,1,1,1,1,1,1,1,1,1,1,1,1,1,
1,1,1,1,1,1,1,6),(0.00577184337450718,0.0153846153846154,0.0307692307692308,
0.0461538461538462,0.0615384615384615,0.0769230769230769,0.0923076923076923,
0.107692307692308,0.123076923076923,0.138461538461538,0.153846153846154,
0.169230769230769,0.184615384615385,0.2,0.215384615384615,0.230769230769231,
0.246153846153846,0.261538461538462,0.276923076923077,0.292307692307692,
0.307692307692308,0.323076923076923,0.338461538461538,0.353846153846154,
0.369230769230769,0.384615384615385,0.4,0.415384615384615,0.430769230769231,
0.446153846153846,0.461538461538462,0.476923076923077,0.492307692307692,
0.507692307692308,0.523076923076923,0.538461538461538,0.553846153846154,
0.569230769230769,0.584615384615384,0.6,0.615384615384615,0.63076923076923,
0.646153846153846,0.661538461538461,0.676923076923076,0.692307692307692,
0.707692307692307,0.723076923076922,0.738461538461538,0.753846153846153,
0.769230769230768,0.784615384615384,0.799999999999999,0.815384615384614,
0.83076923076923,0.846153846153845,0.86153846153846,0.876923076923076,0.892307692307691,
0.907692307692306,0.923076923076922,0.938461538461537,0.953846153846152,
0.969230769230768,0.984615384615383,1.),.UNSPECIFIED.)
CURVE()
GEOMETRIC_REPRESENTATION_ITEM()
RATIONAL_B_SPLINE_CURVE((1.,1.,1.,1.,1.,1.,1.,1.,1.,1.,1.,1.,1.,1.,1.,1.,
1.,1.,1.,1.,1.,1.,1.,1.,1.,1.,1.,1.,1.,1.,1.,1.,1.,1.,1.,1.,1.,1.,1.,1.,
1.,1.,1.,1.,1.,1.,1.,1.,1.,1.,1.,1.,1.,1.,1.,1.,1.,1.,1.,1.,1.,1.,1.,1.,
1.,1.,1.,1.,1.,1.))
REPRESENTATION_ITEM('')
);
#274=(
BOUNDED_CURVE()
B_SPLINE_CURVE(5,(#43380,#43381,#43382,#43383,#43384,#43385,#43386,#43387,
#43388,#43389,#43390,#43391,#43392,#43393,#43394,#43395,#43396,#43397,#43398,
#43399,#43400,#43401,#43402,#43403,#43404,#43405,#43406,#43407,#43408,#43409,
#43410,#43411,#43412,#43413,#43414,#43415,#43416,#43417,#43418,#43419,#43420,
#43421,#43422,#43423,#43424,#43425,#43426,#43427,#43428,#43429,#43430,#43431,
#43432,#43433,#43434,#43435,#43436,#43437,#43438,#43439,#43440,#43441,#43442,
#43443,#43444,#43445,#43446,#43447,#43448,#43449),.UNSPECIFIED.,.F.,.F.)
B_SPLINE_CURVE_WITH_KNOTS((6,1,1,1,1,1,1,1,1,1,1,1,1,1,1,1,1,1,1,1,1,1,
1,1,1,1,1,1,1,1,1,1,1,1,1,1,1,1,1,1,1,1,1,1,1,1,1,1,1,1,1,1,1,1,1,1,1,1,
1,1,1,1,1,1,1,6),(0.,0.0153846153846154,0.0307692307692308,0.0461538461538462,
0.0615384615384615,0.0769230769230769,0.0923076923076923,0.107692307692308,
0.123076923076923,0.138461538461538,0.153846153846154,0.169230769230769,
0.184615384615385,0.2,0.215384615384615,0.230769230769231,0.246153846153846,
0.261538461538462,0.276923076923077,0.292307692307692,0.307692307692308,
0.323076923076923,0.338461538461538,0.353846153846154,0.369230769230769,
0.384615384615385,0.4,0.415384615384615,0.430769230769231,0.446153846153846,
0.461538461538462,0.476923076923077,0.492307692307692,0.507692307692308,
0.523076923076923,0.538461538461538,0.553846153846154,0.569230769230769,
0.584615384615384,0.6,0.615384615384615,0.63076923076923,0.646153846153846,
0.661538461538461,0.676923076923076,0.692307692307692,0.707692307692307,
0.723076923076922,0.738461538461538,0.753846153846153,0.769230769230768,
0.784615384615384,0.799999999999999,0.815384615384614,0.83076923076923,
0.846153846153845,0.86153846153846,0.876923076923076,0.892307692307691,
0.907692307692306,0.923076923076922,0.938461538461537,0.953846153846152,
0.969230769230768,0.984615384615383,0.994228156739716),.UNSPECIFIED.)
CURVE()
GEOMETRIC_REPRESENTATION_ITEM()
RATIONAL_B_SPLINE_CURVE((1.,1.,1.,1.,1.,1.,1.,1.,1.,1.,1.,1.,1.,1.,1.,1.,
1.,1.,1.,1.,1.,1.,1.,1.,1.,1.,1.,1.,1.,1.,1.,1.,1.,1.,1.,1.,1.,1.,1.,1.,
1.,1.,1.,1.,1.,1.,1.,1.,1.,1.,1.,1.,1.,1.,1.,1.,1.,1.,1.,1.,1.,1.,1.,1.,
1.,1.,1.,1.,1.,1.))
REPRESENTATION_ITEM('')
);
#275=(
BOUNDED_CURVE()
B_SPLINE_CURVE(5,(#43453,#43454,#43455,#43456,#43457,#43458,#43459,#43460,
#43461,#43462,#43463,#43464,#43465,#43466,#43467,#43468,#43469,#43470,#43471,
#43472,#43473,#43474,#43475,#43476,#43477,#43478,#43479,#43480,#43481,#43482,
#43483,#43484,#43485,#43486,#43487,#43488,#43489,#43490,#43491,#43492,#43493,
#43494,#43495,#43496,#43497,#43498,#43499,#43500,#43501,#43502,#43503,#43504,
#43505,#43506,#43507,#43508,#43509,#43510,#43511,#43512,#43513,#43514,#43515,
#43516,#43517,#43518,#43519,#43520,#43521,#43522),.UNSPECIFIED.,.F.,.F.)
B_SPLINE_CURVE_WITH_KNOTS((6,1,1,1,1,1,1,1,1,1,1,1,1,1,1,1,1,1,1,1,1,1,
1,1,1,1,1,1,1,1,1,1,1,1,1,1,1,1,1,1,1,1,1,1,1,1,1,1,1,1,1,1,1,1,1,1,1,1,
1,1,1,1,1,1,1,6),(0.00577184337450174,0.0153846153846154,0.0307692307692308,
0.0461538461538462,0.0615384615384615,0.0769230769230769,0.0923076923076923,
0.107692307692308,0.123076923076923,0.138461538461538,0.153846153846154,
0.169230769230769,0.184615384615385,0.2,0.215384615384615,0.230769230769231,
0.246153846153846,0.261538461538462,0.276923076923077,0.292307692307692,
0.307692307692308,0.323076923076923,0.338461538461538,0.353846153846154,
0.369230769230769,0.384615384615385,0.4,0.415384615384615,0.430769230769231,
0.446153846153846,0.461538461538462,0.476923076923077,0.492307692307692,
0.507692307692308,0.523076923076923,0.538461538461538,0.553846153846154,
0.569230769230769,0.584615384615384,0.6,0.615384615384615,0.63076923076923,
0.646153846153846,0.661538461538461,0.676923076923076,0.692307692307692,
0.707692307692307,0.723076923076922,0.738461538461538,0.753846153846153,
0.769230769230768,0.784615384615384,0.799999999999999,0.815384615384614,
0.83076923076923,0.846153846153845,0.86153846153846,0.876923076923076,0.892307692307691,
0.907692307692306,0.923076923076922,0.938461538461537,0.953846153846152,
0.969230769230768,0.984615384615383,1.),.UNSPECIFIED.)
CURVE()
GEOMETRIC_REPRESENTATION_ITEM()
RATIONAL_B_SPLINE_CURVE((1.,1.,1.,1.,1.,1.,1.,1.,1.,1.,1.,1.,1.,1.,1.,1.,
1.,1.,1.,1.,1.,1.,1.,1.,1.,1.,1.,1.,1.,1.,1.,1.,1.,1.,1.,1.,1.,1.,1.,1.,
1.,1.,1.,1.,1.,1.,1.,1.,1.,1.,1.,1.,1.,1.,1.,1.,1.,1.,1.,1.,1.,1.,1.,1.,
1.,1.,1.,1.,1.,1.))
REPRESENTATION_ITEM('')
);
#276=(
BOUNDED_CURVE()
B_SPLINE_CURVE(5,(#43526,#43527,#43528,#43529,#43530,#43531,#43532,#43533,
#43534,#43535,#43536,#43537,#43538,#43539,#43540,#43541,#43542,#43543,#43544,
#43545,#43546,#43547,#43548,#43549,#43550,#43551,#43552,#43553,#43554,#43555,
#43556,#43557,#43558,#43559,#43560,#43561,#43562,#43563,#43564,#43565,#43566,
#43567,#43568,#43569,#43570,#43571,#43572,#43573,#43574,#43575,#43576,#43577,
#43578,#43579,#43580,#43581,#43582,#43583,#43584,#43585,#43586,#43587,#43588,
#43589,#43590,#43591,#43592,#43593,#43594,#43595),.UNSPECIFIED.,.F.,.F.)
B_SPLINE_CURVE_WITH_KNOTS((6,1,1,1,1,1,1,1,1,1,1,1,1,1,1,1,1,1,1,1,1,1,
1,1,1,1,1,1,1,1,1,1,1,1,1,1,1,1,1,1,1,1,1,1,1,1,1,1,1,1,1,1,1,1,1,1,1,1,
1,1,1,1,1,1,1,6),(0.,0.0153846153846154,0.0307692307692308,0.0461538461538462,
0.0615384615384615,0.0769230769230769,0.0923076923076923,0.107692307692308,
0.123076923076923,0.138461538461538,0.153846153846154,0.169230769230769,
0.184615384615385,0.2,0.215384615384615,0.230769230769231,0.246153846153846,
0.261538461538462,0.276923076923077,0.292307692307692,0.307692307692308,
0.323076923076923,0.338461538461538,0.353846153846154,0.369230769230769,
0.384615384615385,0.4,0.415384615384615,0.430769230769231,0.446153846153846,
0.461538461538462,0.476923076923077,0.492307692307692,0.507692307692308,
0.523076923076923,0.538461538461538,0.553846153846154,0.569230769230769,
0.584615384615384,0.6,0.615384615384615,0.63076923076923,0.646153846153846,
0.661538461538461,0.676923076923076,0.692307692307692,0.707692307692307,
0.723076923076922,0.738461538461538,0.753846153846153,0.769230769230768,
0.784615384615384,0.799999999999999,0.815384615384614,0.83076923076923,
0.846153846153845,0.86153846153846,0.876923076923076,0.892307692307691,
0.907692307692306,0.923076923076922,0.938461538461537,0.953846153846152,
0.969230769230768,0.984615384615383,0.994228156739722),.UNSPECIFIED.)
CURVE()
GEOMETRIC_REPRESENTATION_ITEM()
RATIONAL_B_SPLINE_CURVE((1.,1.,1.,1.,1.,1.,1.,1.,1.,1.,1.,1.,1.,1.,1.,1.,
1.,1.,1.,1.,1.,1.,1.,1.,1.,1.,1.,1.,1.,1.,1.,1.,1.,1.,1.,1.,1.,1.,1.,1.,
1.,1.,1.,1.,1.,1.,1.,1.,1.,1.,1.,1.,1.,1.,1.,1.,1.,1.,1.,1.,1.,1.,1.,1.,
1.,1.,1.,1.,1.,1.))
REPRESENTATION_ITEM('')
);
#277=(
BOUNDED_CURVE()
B_SPLINE_CURVE(5,(#43599,#43600,#43601,#43602,#43603,#43604,#43605,#43606,
#43607,#43608,#43609,#43610,#43611,#43612,#43613,#43614,#43615,#43616,#43617,
#43618,#43619,#43620,#43621,#43622,#43623,#43624,#43625,#43626,#43627,#43628,
#43629,#43630,#43631,#43632,#43633,#43634,#43635,#43636,#43637,#43638,#43639,
#43640,#43641,#43642,#43643,#43644,#43645,#43646,#43647,#43648,#43649,#43650,
#43651,#43652,#43653,#43654,#43655,#43656,#43657,#43658,#43659,#43660,#43661,
#43662,#43663,#43664,#43665,#43666,#43667,#43668),.UNSPECIFIED.,.F.,.F.)
B_SPLINE_CURVE_WITH_KNOTS((6,1,1,1,1,1,1,1,1,1,1,1,1,1,1,1,1,1,1,1,1,1,
1,1,1,1,1,1,1,1,1,1,1,1,1,1,1,1,1,1,1,1,1,1,1,1,1,1,1,1,1,1,1,1,1,1,1,1,
1,1,1,1,1,1,1,6),(0.00577184337450943,0.0153846153846154,0.0307692307692308,
0.0461538461538462,0.0615384615384615,0.0769230769230769,0.0923076923076923,
0.107692307692308,0.123076923076923,0.138461538461538,0.153846153846154,
0.169230769230769,0.184615384615385,0.2,0.215384615384615,0.230769230769231,
0.246153846153846,0.261538461538462,0.276923076923077,0.292307692307692,
0.307692307692308,0.323076923076923,0.338461538461538,0.353846153846154,
0.369230769230769,0.384615384615385,0.4,0.415384615384615,0.430769230769231,
0.446153846153846,0.461538461538462,0.476923076923077,0.492307692307692,
0.507692307692308,0.523076923076923,0.538461538461538,0.553846153846154,
0.569230769230769,0.584615384615384,0.6,0.615384615384615,0.63076923076923,
0.646153846153846,0.661538461538461,0.676923076923076,0.692307692307692,
0.707692307692307,0.723076923076922,0.738461538461538,0.753846153846153,
0.769230769230768,0.784615384615384,0.799999999999999,0.815384615384614,
0.83076923076923,0.846153846153845,0.86153846153846,0.876923076923076,0.892307692307691,
0.907692307692306,0.923076923076922,0.938461538461537,0.953846153846152,
0.969230769230768,0.984615384615383,1.),.UNSPECIFIED.)
CURVE()
GEOMETRIC_REPRESENTATION_ITEM()
RATIONAL_B_SPLINE_CURVE((1.,1.,1.,1.,1.,1.,1.,1.,1.,1.,1.,1.,1.,1.,1.,1.,
1.,1.,1.,1.,1.,1.,1.,1.,1.,1.,1.,1.,1.,1.,1.,1.,1.,1.,1.,1.,1.,1.,1.,1.,
1.,1.,1.,1.,1.,1.,1.,1.,1.,1.,1.,1.,1.,1.,1.,1.,1.,1.,1.,1.,1.,1.,1.,1.,
1.,1.,1.,1.,1.,1.))
REPRESENTATION_ITEM('')
);
#278=(
BOUNDED_CURVE()
B_SPLINE_CURVE(5,(#43672,#43673,#43674,#43675,#43676,#43677,#43678,#43679,
#43680,#43681,#43682,#43683,#43684,#43685,#43686,#43687,#43688,#43689,#43690,
#43691,#43692,#43693,#43694,#43695,#43696,#43697,#43698,#43699,#43700,#43701,
#43702,#43703,#43704,#43705,#43706,#43707,#43708,#43709,#43710,#43711,#43712,
#43713,#43714,#43715,#43716,#43717,#43718,#43719,#43720,#43721,#43722,#43723,
#43724,#43725,#43726,#43727,#43728,#43729,#43730,#43731,#43732,#43733,#43734,
#43735,#43736,#43737,#43738,#43739,#43740,#43741),.UNSPECIFIED.,.F.,.F.)
B_SPLINE_CURVE_WITH_KNOTS((6,1,1,1,1,1,1,1,1,1,1,1,1,1,1,1,1,1,1,1,1,1,
1,1,1,1,1,1,1,1,1,1,1,1,1,1,1,1,1,1,1,1,1,1,1,1,1,1,1,1,1,1,1,1,1,1,1,1,
1,1,1,1,1,1,1,6),(0.,0.0153846153846154,0.0307692307692308,0.0461538461538462,
0.0615384615384615,0.0769230769230769,0.0923076923076923,0.107692307692308,
0.123076923076923,0.138461538461538,0.153846153846154,0.169230769230769,
0.184615384615385,0.2,0.215384615384615,0.230769230769231,0.246153846153846,
0.261538461538462,0.276923076923077,0.292307692307692,0.307692307692308,
0.323076923076923,0.338461538461538,0.353846153846154,0.369230769230769,
0.384615384615385,0.4,0.415384615384615,0.430769230769231,0.446153846153846,
0.461538461538462,0.476923076923077,0.492307692307692,0.507692307692308,
0.523076923076923,0.538461538461538,0.553846153846154,0.569230769230769,
0.584615384615384,0.6,0.615384615384615,0.63076923076923,0.646153846153846,
0.661538461538461,0.676923076923076,0.692307692307692,0.707692307692307,
0.723076923076922,0.738461538461538,0.753846153846153,0.769230769230768,
0.784615384615384,0.799999999999999,0.815384615384614,0.83076923076923,
0.846153846153845,0.86153846153846,0.876923076923076,0.892307692307691,
0.907692307692306,0.923076923076922,0.938461538461537,0.953846153846152,
0.969230769230768,0.984615384615383,0.994228156739699),.UNSPECIFIED.)
CURVE()
GEOMETRIC_REPRESENTATION_ITEM()
RATIONAL_B_SPLINE_CURVE((1.,1.,1.,1.,1.,1.,1.,1.,1.,1.,1.,1.,1.,1.,1.,1.,
1.,1.,1.,1.,1.,1.,1.,1.,1.,1.,1.,1.,1.,1.,1.,1.,1.,1.,1.,1.,1.,1.,1.,1.,
1.,1.,1.,1.,1.,1.,1.,1.,1.,1.,1.,1.,1.,1.,1.,1.,1.,1.,1.,1.,1.,1.,1.,1.,
1.,1.,1.,1.,1.,1.))
REPRESENTATION_ITEM('')
);
#279=(
BOUNDED_CURVE()
B_SPLINE_CURVE(5,(#43745,#43746,#43747,#43748,#43749,#43750,#43751,#43752,
#43753,#43754,#43755,#43756,#43757,#43758,#43759,#43760,#43761,#43762,#43763,
#43764,#43765,#43766,#43767,#43768,#43769,#43770,#43771,#43772,#43773,#43774,
#43775,#43776,#43777,#43778,#43779,#43780,#43781,#43782,#43783,#43784,#43785,
#43786,#43787,#43788,#43789,#43790,#43791,#43792,#43793,#43794,#43795,#43796,
#43797,#43798,#43799,#43800,#43801,#43802,#43803,#43804,#43805,#43806,#43807,
#43808,#43809,#43810,#43811,#43812,#43813,#43814),.UNSPECIFIED.,.F.,.F.)
B_SPLINE_CURVE_WITH_KNOTS((6,1,1,1,1,1,1,1,1,1,1,1,1,1,1,1,1,1,1,1,1,1,
1,1,1,1,1,1,1,1,1,1,1,1,1,1,1,1,1,1,1,1,1,1,1,1,1,1,1,1,1,1,1,1,1,1,1,1,
1,1,1,1,1,1,1,6),(0.00577184337450665,0.0153846153846154,0.0307692307692308,
0.0461538461538462,0.0615384615384615,0.0769230769230769,0.0923076923076923,
0.107692307692308,0.123076923076923,0.138461538461538,0.153846153846154,
0.169230769230769,0.184615384615385,0.2,0.215384615384615,0.230769230769231,
0.246153846153846,0.261538461538462,0.276923076923077,0.292307692307692,
0.307692307692308,0.323076923076923,0.338461538461538,0.353846153846154,
0.369230769230769,0.384615384615385,0.4,0.415384615384615,0.430769230769231,
0.446153846153846,0.461538461538462,0.476923076923077,0.492307692307692,
0.507692307692308,0.523076923076923,0.538461538461538,0.553846153846154,
0.569230769230769,0.584615384615384,0.6,0.615384615384615,0.63076923076923,
0.646153846153846,0.661538461538461,0.676923076923076,0.692307692307692,
0.707692307692307,0.723076923076922,0.738461538461538,0.753846153846153,
0.769230769230768,0.784615384615384,0.799999999999999,0.815384615384614,
0.83076923076923,0.846153846153845,0.86153846153846,0.876923076923076,0.892307692307691,
0.907692307692306,0.923076923076922,0.938461538461537,0.953846153846152,
0.969230769230768,0.984615384615383,1.),.UNSPECIFIED.)
CURVE()
GEOMETRIC_REPRESENTATION_ITEM()
RATIONAL_B_SPLINE_CURVE((1.,1.,1.,1.,1.,1.,1.,1.,1.,1.,1.,1.,1.,1.,1.,1.,
1.,1.,1.,1.,1.,1.,1.,1.,1.,1.,1.,1.,1.,1.,1.,1.,1.,1.,1.,1.,1.,1.,1.,1.,
1.,1.,1.,1.,1.,1.,1.,1.,1.,1.,1.,1.,1.,1.,1.,1.,1.,1.,1.,1.,1.,1.,1.,1.,
1.,1.,1.,1.,1.,1.))
REPRESENTATION_ITEM('')
);
#280=(
BOUNDED_CURVE()
B_SPLINE_CURVE(5,(#43818,#43819,#43820,#43821,#43822,#43823,#43824,#43825,
#43826,#43827,#43828,#43829,#43830,#43831,#43832,#43833,#43834,#43835,#43836,
#43837,#43838,#43839,#43840,#43841,#43842,#43843,#43844,#43845,#43846,#43847,
#43848,#43849,#43850,#43851,#43852,#43853,#43854,#43855,#43856,#43857,#43858,
#43859,#43860,#43861,#43862,#43863,#43864,#43865,#43866,#43867,#43868,#43869,
#43870,#43871,#43872,#43873,#43874,#43875,#43876,#43877,#43878,#43879,#43880,
#43881,#43882,#43883,#43884,#43885,#43886,#43887),.UNSPECIFIED.,.F.,.F.)
B_SPLINE_CURVE_WITH_KNOTS((6,1,1,1,1,1,1,1,1,1,1,1,1,1,1,1,1,1,1,1,1,1,
1,1,1,1,1,1,1,1,1,1,1,1,1,1,1,1,1,1,1,1,1,1,1,1,1,1,1,1,1,1,1,1,1,1,1,1,
1,1,1,1,1,1,1,6),(0.,0.0153846153846154,0.0307692307692308,0.0461538461538462,
0.0615384615384615,0.0769230769230769,0.0923076923076923,0.107692307692308,
0.123076923076923,0.138461538461538,0.153846153846154,0.169230769230769,
0.184615384615385,0.2,0.215384615384615,0.230769230769231,0.246153846153846,
0.261538461538462,0.276923076923077,0.292307692307692,0.307692307692308,
0.323076923076923,0.338461538461538,0.353846153846154,0.369230769230769,
0.384615384615385,0.4,0.415384615384615,0.430769230769231,0.446153846153846,
0.461538461538462,0.476923076923077,0.492307692307692,0.507692307692308,
0.523076923076923,0.538461538461538,0.553846153846154,0.569230769230769,
0.584615384615384,0.6,0.615384615384615,0.63076923076923,0.646153846153846,
0.661538461538461,0.676923076923076,0.692307692307692,0.707692307692307,
0.723076923076922,0.738461538461538,0.753846153846153,0.769230769230768,
0.784615384615384,0.799999999999999,0.815384615384614,0.83076923076923,
0.846153846153845,0.86153846153846,0.876923076923076,0.892307692307691,
0.907692307692306,0.923076923076922,0.938461538461537,0.953846153846152,
0.969230769230768,0.984615384615383,0.994228156739691),.UNSPECIFIED.)
CURVE()
GEOMETRIC_REPRESENTATION_ITEM()
RATIONAL_B_SPLINE_CURVE((1.,1.,1.,1.,1.,1.,1.,1.,1.,1.,1.,1.,1.,1.,1.,1.,
1.,1.,1.,1.,1.,1.,1.,1.,1.,1.,1.,1.,1.,1.,1.,1.,1.,1.,1.,1.,1.,1.,1.,1.,
1.,1.,1.,1.,1.,1.,1.,1.,1.,1.,1.,1.,1.,1.,1.,1.,1.,1.,1.,1.,1.,1.,1.,1.,
1.,1.,1.,1.,1.,1.))
REPRESENTATION_ITEM('')
);
#281=(
BOUNDED_CURVE()
B_SPLINE_CURVE(5,(#43891,#43892,#43893,#43894,#43895,#43896,#43897,#43898,
#43899,#43900,#43901,#43902,#43903,#43904,#43905,#43906,#43907,#43908,#43909,
#43910,#43911,#43912,#43913,#43914,#43915,#43916,#43917,#43918,#43919,#43920,
#43921,#43922,#43923,#43924,#43925,#43926,#43927,#43928,#43929,#43930,#43931,
#43932,#43933,#43934,#43935,#43936,#43937,#43938,#43939,#43940,#43941,#43942,
#43943,#43944,#43945,#43946,#43947,#43948,#43949,#43950,#43951,#43952,#43953,
#43954,#43955,#43956,#43957,#43958,#43959,#43960),.UNSPECIFIED.,.F.,.F.)
B_SPLINE_CURVE_WITH_KNOTS((6,1,1,1,1,1,1,1,1,1,1,1,1,1,1,1,1,1,1,1,1,1,
1,1,1,1,1,1,1,1,1,1,1,1,1,1,1,1,1,1,1,1,1,1,1,1,1,1,1,1,1,1,1,1,1,1,1,1,
1,1,1,1,1,1,1,6),(0.00577184337450785,0.0153846153846154,0.0307692307692308,
0.0461538461538462,0.0615384615384615,0.0769230769230769,0.0923076923076923,
0.107692307692308,0.123076923076923,0.138461538461538,0.153846153846154,
0.169230769230769,0.184615384615385,0.2,0.215384615384615,0.230769230769231,
0.246153846153846,0.261538461538462,0.276923076923077,0.292307692307692,
0.307692307692308,0.323076923076923,0.338461538461538,0.353846153846154,
0.369230769230769,0.384615384615385,0.4,0.415384615384615,0.430769230769231,
0.446153846153846,0.461538461538462,0.476923076923077,0.492307692307692,
0.507692307692308,0.523076923076923,0.538461538461538,0.553846153846154,
0.569230769230769,0.584615384615384,0.6,0.615384615384615,0.63076923076923,
0.646153846153846,0.661538461538461,0.676923076923076,0.692307692307692,
0.707692307692307,0.723076923076922,0.738461538461538,0.753846153846153,
0.769230769230768,0.784615384615384,0.799999999999999,0.815384615384614,
0.83076923076923,0.846153846153845,0.86153846153846,0.876923076923076,0.892307692307691,
0.907692307692306,0.923076923076922,0.938461538461537,0.953846153846152,
0.969230769230768,0.984615384615383,1.),.UNSPECIFIED.)
CURVE()
GEOMETRIC_REPRESENTATION_ITEM()
RATIONAL_B_SPLINE_CURVE((1.,1.,1.,1.,1.,1.,1.,1.,1.,1.,1.,1.,1.,1.,1.,1.,
1.,1.,1.,1.,1.,1.,1.,1.,1.,1.,1.,1.,1.,1.,1.,1.,1.,1.,1.,1.,1.,1.,1.,1.,
1.,1.,1.,1.,1.,1.,1.,1.,1.,1.,1.,1.,1.,1.,1.,1.,1.,1.,1.,1.,1.,1.,1.,1.,
1.,1.,1.,1.,1.,1.))
REPRESENTATION_ITEM('')
);
#282=(
BOUNDED_CURVE()
B_SPLINE_CURVE(5,(#43964,#43965,#43966,#43967,#43968,#43969,#43970,#43971,
#43972,#43973,#43974,#43975,#43976,#43977,#43978,#43979,#43980,#43981,#43982,
#43983,#43984,#43985,#43986,#43987,#43988,#43989,#43990,#43991,#43992,#43993,
#43994,#43995,#43996,#43997,#43998,#43999,#44000,#44001,#44002,#44003,#44004,
#44005,#44006,#44007,#44008,#44009,#44010,#44011,#44012,#44013,#44014,#44015,
#44016,#44017,#44018,#44019,#44020,#44021,#44022,#44023,#44024,#44025,#44026,
#44027,#44028,#44029,#44030,#44031,#44032,#44033),.UNSPECIFIED.,.F.,.F.)
B_SPLINE_CURVE_WITH_KNOTS((6,1,1,1,1,1,1,1,1,1,1,1,1,1,1,1,1,1,1,1,1,1,
1,1,1,1,1,1,1,1,1,1,1,1,1,1,1,1,1,1,1,1,1,1,1,1,1,1,1,1,1,1,1,1,1,1,1,1,
1,1,1,1,1,1,1,6),(0.,0.0153846153846154,0.0307692307692308,0.0461538461538462,
0.0615384615384615,0.0769230769230769,0.0923076923076923,0.107692307692308,
0.123076923076923,0.138461538461538,0.153846153846154,0.169230769230769,
0.184615384615385,0.2,0.215384615384615,0.230769230769231,0.246153846153846,
0.261538461538462,0.276923076923077,0.292307692307692,0.307692307692308,
0.323076923076923,0.338461538461538,0.353846153846154,0.369230769230769,
0.384615384615385,0.4,0.415384615384615,0.430769230769231,0.446153846153846,
0.461538461538462,0.476923076923077,0.492307692307692,0.507692307692308,
0.523076923076923,0.538461538461538,0.553846153846154,0.569230769230769,
0.584615384615384,0.6,0.615384615384615,0.63076923076923,0.646153846153846,
0.661538461538461,0.676923076923076,0.692307692307692,0.707692307692307,
0.723076923076922,0.738461538461538,0.753846153846153,0.769230769230768,
0.784615384615384,0.799999999999999,0.815384615384614,0.83076923076923,
0.846153846153845,0.86153846153846,0.876923076923076,0.892307692307691,
0.907692307692306,0.923076923076922,0.938461538461537,0.953846153846152,
0.969230769230768,0.984615384615383,0.994228156739708),.UNSPECIFIED.)
CURVE()
GEOMETRIC_REPRESENTATION_ITEM()
RATIONAL_B_SPLINE_CURVE((1.,1.,1.,1.,1.,1.,1.,1.,1.,1.,1.,1.,1.,1.,1.,1.,
1.,1.,1.,1.,1.,1.,1.,1.,1.,1.,1.,1.,1.,1.,1.,1.,1.,1.,1.,1.,1.,1.,1.,1.,
1.,1.,1.,1.,1.,1.,1.,1.,1.,1.,1.,1.,1.,1.,1.,1.,1.,1.,1.,1.,1.,1.,1.,1.,
1.,1.,1.,1.,1.,1.))
REPRESENTATION_ITEM('')
);
#283=(
BOUNDED_CURVE()
B_SPLINE_CURVE(5,(#44037,#44038,#44039,#44040,#44041,#44042,#44043,#44044,
#44045,#44046,#44047,#44048,#44049,#44050,#44051,#44052,#44053,#44054,#44055,
#44056,#44057,#44058,#44059,#44060,#44061,#44062,#44063,#44064,#44065,#44066,
#44067,#44068,#44069,#44070,#44071,#44072,#44073,#44074,#44075,#44076,#44077,
#44078,#44079,#44080,#44081,#44082,#44083,#44084,#44085,#44086,#44087,#44088,
#44089,#44090,#44091,#44092,#44093,#44094,#44095,#44096,#44097,#44098,#44099,
#44100,#44101,#44102,#44103,#44104,#44105,#44106),.UNSPECIFIED.,.F.,.F.)
B_SPLINE_CURVE_WITH_KNOTS((6,1,1,1,1,1,1,1,1,1,1,1,1,1,1,1,1,1,1,1,1,1,
1,1,1,1,1,1,1,1,1,1,1,1,1,1,1,1,1,1,1,1,1,1,1,1,1,1,1,1,1,1,1,1,1,1,1,1,
1,1,1,1,1,1,1,6),(0.00577184337450072,0.0153846153846154,0.0307692307692308,
0.0461538461538462,0.0615384615384615,0.0769230769230769,0.0923076923076923,
0.107692307692308,0.123076923076923,0.138461538461538,0.153846153846154,
0.169230769230769,0.184615384615385,0.2,0.215384615384615,0.230769230769231,
0.246153846153846,0.261538461538462,0.276923076923077,0.292307692307692,
0.307692307692308,0.323076923076923,0.338461538461538,0.353846153846154,
0.369230769230769,0.384615384615385,0.4,0.415384615384615,0.430769230769231,
0.446153846153846,0.461538461538462,0.476923076923077,0.492307692307692,
0.507692307692308,0.523076923076923,0.538461538461538,0.553846153846154,
0.569230769230769,0.584615384615384,0.6,0.615384615384615,0.63076923076923,
0.646153846153846,0.661538461538461,0.676923076923076,0.692307692307692,
0.707692307692307,0.723076923076922,0.738461538461538,0.753846153846153,
0.769230769230768,0.784615384615384,0.799999999999999,0.815384615384614,
0.83076923076923,0.846153846153845,0.86153846153846,0.876923076923076,0.892307692307691,
0.907692307692306,0.923076923076922,0.938461538461537,0.953846153846152,
0.969230769230768,0.984615384615383,1.),.UNSPECIFIED.)
CURVE()
GEOMETRIC_REPRESENTATION_ITEM()
RATIONAL_B_SPLINE_CURVE((1.,1.,1.,1.,1.,1.,1.,1.,1.,1.,1.,1.,1.,1.,1.,1.,
1.,1.,1.,1.,1.,1.,1.,1.,1.,1.,1.,1.,1.,1.,1.,1.,1.,1.,1.,1.,1.,1.,1.,1.,
1.,1.,1.,1.,1.,1.,1.,1.,1.,1.,1.,1.,1.,1.,1.,1.,1.,1.,1.,1.,1.,1.,1.,1.,
1.,1.,1.,1.,1.,1.))
REPRESENTATION_ITEM('')
);
#284=(
BOUNDED_CURVE()
B_SPLINE_CURVE(5,(#44110,#44111,#44112,#44113,#44114,#44115,#44116,#44117,
#44118,#44119,#44120,#44121,#44122,#44123,#44124,#44125,#44126,#44127,#44128,
#44129,#44130,#44131,#44132,#44133,#44134,#44135,#44136,#44137,#44138,#44139,
#44140,#44141,#44142,#44143,#44144,#44145,#44146,#44147,#44148,#44149,#44150,
#44151,#44152,#44153,#44154,#44155,#44156,#44157,#44158,#44159,#44160,#44161,
#44162,#44163,#44164,#44165,#44166,#44167,#44168,#44169,#44170,#44171,#44172,
#44173,#44174,#44175,#44176,#44177,#44178,#44179),.UNSPECIFIED.,.F.,.F.)
B_SPLINE_CURVE_WITH_KNOTS((6,1,1,1,1,1,1,1,1,1,1,1,1,1,1,1,1,1,1,1,1,1,
1,1,1,1,1,1,1,1,1,1,1,1,1,1,1,1,1,1,1,1,1,1,1,1,1,1,1,1,1,1,1,1,1,1,1,1,
1,1,1,1,1,1,1,6),(0.,0.0153846153846154,0.0307692307692308,0.0461538461538462,
0.0615384615384615,0.0769230769230769,0.0923076923076923,0.107692307692308,
0.123076923076923,0.138461538461538,0.153846153846154,0.169230769230769,
0.184615384615385,0.2,0.215384615384615,0.230769230769231,0.246153846153846,
0.261538461538462,0.276923076923077,0.292307692307692,0.307692307692308,
0.323076923076923,0.338461538461538,0.353846153846154,0.369230769230769,
0.384615384615385,0.4,0.415384615384615,0.430769230769231,0.446153846153846,
0.461538461538462,0.476923076923077,0.492307692307692,0.507692307692308,
0.523076923076923,0.538461538461538,0.553846153846154,0.569230769230769,
0.584615384615384,0.6,0.615384615384615,0.63076923076923,0.646153846153846,
0.661538461538461,0.676923076923076,0.692307692307692,0.707692307692307,
0.723076923076922,0.738461538461538,0.753846153846153,0.769230769230768,
0.784615384615384,0.799999999999999,0.815384615384614,0.83076923076923,
0.846153846153845,0.86153846153846,0.876923076923076,0.892307692307691,
0.907692307692306,0.923076923076922,0.938461538461537,0.953846153846152,
0.969230769230768,0.984615384615383,0.994228156739706),.UNSPECIFIED.)
CURVE()
GEOMETRIC_REPRESENTATION_ITEM()
RATIONAL_B_SPLINE_CURVE((1.,1.,1.,1.,1.,1.,1.,1.,1.,1.,1.,1.,1.,1.,1.,1.,
1.,1.,1.,1.,1.,1.,1.,1.,1.,1.,1.,1.,1.,1.,1.,1.,1.,1.,1.,1.,1.,1.,1.,1.,
1.,1.,1.,1.,1.,1.,1.,1.,1.,1.,1.,1.,1.,1.,1.,1.,1.,1.,1.,1.,1.,1.,1.,1.,
1.,1.,1.,1.,1.,1.))
REPRESENTATION_ITEM('')
);
#285=(
BOUNDED_CURVE()
B_SPLINE_CURVE(5,(#44183,#44184,#44185,#44186,#44187,#44188,#44189,#44190,
#44191,#44192,#44193,#44194,#44195,#44196,#44197,#44198,#44199,#44200,#44201,
#44202,#44203,#44204,#44205,#44206,#44207,#44208,#44209,#44210,#44211,#44212,
#44213,#44214,#44215,#44216,#44217,#44218,#44219,#44220,#44221,#44222,#44223,
#44224,#44225,#44226,#44227,#44228,#44229,#44230,#44231,#44232,#44233,#44234,
#44235,#44236,#44237,#44238,#44239,#44240,#44241,#44242,#44243,#44244,#44245,
#44246,#44247,#44248,#44249,#44250,#44251,#44252),.UNSPECIFIED.,.F.,.F.)
B_SPLINE_CURVE_WITH_KNOTS((6,1,1,1,1,1,1,1,1,1,1,1,1,1,1,1,1,1,1,1,1,1,
1,1,1,1,1,1,1,1,1,1,1,1,1,1,1,1,1,1,1,1,1,1,1,1,1,1,1,1,1,1,1,1,1,1,1,1,
1,1,1,1,1,1,1,6),(0.00577184337450902,0.0153846153846154,0.0307692307692308,
0.0461538461538462,0.0615384615384615,0.0769230769230769,0.0923076923076923,
0.107692307692308,0.123076923076923,0.138461538461538,0.153846153846154,
0.169230769230769,0.184615384615385,0.2,0.215384615384615,0.230769230769231,
0.246153846153846,0.261538461538462,0.276923076923077,0.292307692307692,
0.307692307692308,0.323076923076923,0.338461538461538,0.353846153846154,
0.369230769230769,0.384615384615385,0.4,0.415384615384615,0.430769230769231,
0.446153846153846,0.461538461538462,0.476923076923077,0.492307692307692,
0.507692307692308,0.523076923076923,0.538461538461538,0.553846153846154,
0.569230769230769,0.584615384615384,0.6,0.615384615384615,0.63076923076923,
0.646153846153846,0.661538461538461,0.676923076923076,0.692307692307692,
0.707692307692307,0.723076923076922,0.738461538461538,0.753846153846153,
0.769230769230768,0.784615384615384,0.799999999999999,0.815384615384614,
0.83076923076923,0.846153846153845,0.86153846153846,0.876923076923076,0.892307692307691,
0.907692307692306,0.923076923076922,0.938461538461537,0.953846153846152,
0.969230769230768,0.984615384615383,1.),.UNSPECIFIED.)
CURVE()
GEOMETRIC_REPRESENTATION_ITEM()
RATIONAL_B_SPLINE_CURVE((1.,1.,1.,1.,1.,1.,1.,1.,1.,1.,1.,1.,1.,1.,1.,1.,
1.,1.,1.,1.,1.,1.,1.,1.,1.,1.,1.,1.,1.,1.,1.,1.,1.,1.,1.,1.,1.,1.,1.,1.,
1.,1.,1.,1.,1.,1.,1.,1.,1.,1.,1.,1.,1.,1.,1.,1.,1.,1.,1.,1.,1.,1.,1.,1.,
1.,1.,1.,1.,1.,1.))
REPRESENTATION_ITEM('')
);
#286=(
BOUNDED_CURVE()
B_SPLINE_CURVE(5,(#44256,#44257,#44258,#44259,#44260,#44261,#44262,#44263,
#44264,#44265,#44266,#44267,#44268,#44269,#44270,#44271,#44272,#44273,#44274,
#44275,#44276,#44277,#44278,#44279,#44280,#44281,#44282,#44283,#44284,#44285,
#44286,#44287,#44288,#44289,#44290,#44291,#44292,#44293,#44294,#44295,#44296,
#44297,#44298,#44299,#44300,#44301,#44302,#44303,#44304,#44305,#44306,#44307,
#44308,#44309,#44310,#44311,#44312,#44313,#44314,#44315,#44316,#44317,#44318,
#44319,#44320,#44321,#44322,#44323,#44324,#44325),.UNSPECIFIED.,.F.,.F.)
B_SPLINE_CURVE_WITH_KNOTS((6,1,1,1,1,1,1,1,1,1,1,1,1,1,1,1,1,1,1,1,1,1,
1,1,1,1,1,1,1,1,1,1,1,1,1,1,1,1,1,1,1,1,1,1,1,1,1,1,1,1,1,1,1,1,1,1,1,1,
1,1,1,1,1,1,1,6),(0.,0.0153846153846154,0.0307692307692308,0.0461538461538462,
0.0615384615384615,0.0769230769230769,0.0923076923076923,0.107692307692308,
0.123076923076923,0.138461538461538,0.153846153846154,0.169230769230769,
0.184615384615385,0.2,0.215384615384615,0.230769230769231,0.246153846153846,
0.261538461538462,0.276923076923077,0.292307692307692,0.307692307692308,
0.323076923076923,0.338461538461538,0.353846153846154,0.369230769230769,
0.384615384615385,0.4,0.415384615384615,0.430769230769231,0.446153846153846,
0.461538461538462,0.476923076923077,0.492307692307692,0.507692307692308,
0.523076923076923,0.538461538461538,0.553846153846154,0.569230769230769,
0.584615384615384,0.6,0.615384615384615,0.63076923076923,0.646153846153846,
0.661538461538461,0.676923076923076,0.692307692307692,0.707692307692307,
0.723076923076922,0.738461538461538,0.753846153846153,0.769230769230768,
0.784615384615384,0.799999999999999,0.815384615384614,0.83076923076923,
0.846153846153845,0.86153846153846,0.876923076923076,0.892307692307691,
0.907692307692306,0.923076923076922,0.938461538461537,0.953846153846152,
0.969230769230768,0.984615384615383,0.994228156739698),.UNSPECIFIED.)
CURVE()
GEOMETRIC_REPRESENTATION_ITEM()
RATIONAL_B_SPLINE_CURVE((1.,1.,1.,1.,1.,1.,1.,1.,1.,1.,1.,1.,1.,1.,1.,1.,
1.,1.,1.,1.,1.,1.,1.,1.,1.,1.,1.,1.,1.,1.,1.,1.,1.,1.,1.,1.,1.,1.,1.,1.,
1.,1.,1.,1.,1.,1.,1.,1.,1.,1.,1.,1.,1.,1.,1.,1.,1.,1.,1.,1.,1.,1.,1.,1.,
1.,1.,1.,1.,1.,1.))
REPRESENTATION_ITEM('')
);
#287=(
BOUNDED_CURVE()
B_SPLINE_CURVE(5,(#44329,#44330,#44331,#44332,#44333,#44334,#44335,#44336,
#44337,#44338,#44339,#44340,#44341,#44342,#44343,#44344,#44345,#44346,#44347,
#44348,#44349,#44350,#44351,#44352,#44353,#44354,#44355,#44356,#44357,#44358,
#44359,#44360,#44361,#44362,#44363,#44364,#44365,#44366,#44367,#44368,#44369,
#44370,#44371,#44372,#44373,#44374,#44375,#44376,#44377,#44378,#44379,#44380,
#44381,#44382,#44383,#44384,#44385,#44386,#44387,#44388,#44389,#44390,#44391,
#44392,#44393,#44394,#44395,#44396,#44397,#44398),.UNSPECIFIED.,.F.,.F.)
B_SPLINE_CURVE_WITH_KNOTS((6,1,1,1,1,1,1,1,1,1,1,1,1,1,1,1,1,1,1,1,1,1,
1,1,1,1,1,1,1,1,1,1,1,1,1,1,1,1,1,1,1,1,1,1,1,1,1,1,1,1,1,1,1,1,1,1,1,1,
1,1,1,1,1,1,1,6),(0.00577184337451611,0.0153846153846154,0.0307692307692308,
0.0461538461538462,0.0615384615384615,0.0769230769230769,0.0923076923076923,
0.107692307692308,0.123076923076923,0.138461538461538,0.153846153846154,
0.169230769230769,0.184615384615385,0.2,0.215384615384615,0.230769230769231,
0.246153846153846,0.261538461538462,0.276923076923077,0.292307692307692,
0.307692307692308,0.323076923076923,0.338461538461538,0.353846153846154,
0.369230769230769,0.384615384615385,0.4,0.415384615384615,0.430769230769231,
0.446153846153846,0.461538461538462,0.476923076923077,0.492307692307692,
0.507692307692308,0.523076923076923,0.538461538461538,0.553846153846154,
0.569230769230769,0.584615384615384,0.6,0.615384615384615,0.63076923076923,
0.646153846153846,0.661538461538461,0.676923076923076,0.692307692307692,
0.707692307692307,0.723076923076922,0.738461538461538,0.753846153846153,
0.769230769230768,0.784615384615384,0.799999999999999,0.815384615384614,
0.83076923076923,0.846153846153845,0.86153846153846,0.876923076923076,0.892307692307691,
0.907692307692306,0.923076923076922,0.938461538461537,0.953846153846152,
0.969230769230768,0.984615384615383,1.),.UNSPECIFIED.)
CURVE()
GEOMETRIC_REPRESENTATION_ITEM()
RATIONAL_B_SPLINE_CURVE((1.,1.,1.,1.,1.,1.,1.,1.,1.,1.,1.,1.,1.,1.,1.,1.,
1.,1.,1.,1.,1.,1.,1.,1.,1.,1.,1.,1.,1.,1.,1.,1.,1.,1.,1.,1.,1.,1.,1.,1.,
1.,1.,1.,1.,1.,1.,1.,1.,1.,1.,1.,1.,1.,1.,1.,1.,1.,1.,1.,1.,1.,1.,1.,1.,
1.,1.,1.,1.,1.,1.))
REPRESENTATION_ITEM('')
);
#288=(
BOUNDED_CURVE()
B_SPLINE_CURVE(5,(#44402,#44403,#44404,#44405,#44406,#44407,#44408,#44409,
#44410,#44411,#44412,#44413,#44414,#44415,#44416,#44417,#44418,#44419,#44420,
#44421,#44422,#44423,#44424,#44425,#44426,#44427,#44428,#44429,#44430,#44431,
#44432,#44433,#44434,#44435,#44436,#44437,#44438,#44439,#44440,#44441,#44442,
#44443,#44444,#44445,#44446,#44447,#44448,#44449,#44450,#44451,#44452,#44453,
#44454,#44455,#44456,#44457,#44458,#44459,#44460,#44461,#44462,#44463,#44464,
#44465,#44466,#44467,#44468,#44469,#44470,#44471),.UNSPECIFIED.,.F.,.F.)
B_SPLINE_CURVE_WITH_KNOTS((6,1,1,1,1,1,1,1,1,1,1,1,1,1,1,1,1,1,1,1,1,1,
1,1,1,1,1,1,1,1,1,1,1,1,1,1,1,1,1,1,1,1,1,1,1,1,1,1,1,1,1,1,1,1,1,1,1,1,
1,1,1,1,1,1,1,6),(0.,0.0153846153846154,0.0307692307692308,0.0461538461538462,
0.0615384615384615,0.0769230769230769,0.0923076923076923,0.107692307692308,
0.123076923076923,0.138461538461538,0.153846153846154,0.169230769230769,
0.184615384615385,0.2,0.215384615384615,0.230769230769231,0.246153846153846,
0.261538461538462,0.276923076923077,0.292307692307692,0.307692307692308,
0.323076923076923,0.338461538461538,0.353846153846154,0.369230769230769,
0.384615384615385,0.4,0.415384615384615,0.430769230769231,0.446153846153846,
0.461538461538462,0.476923076923077,0.492307692307692,0.507692307692308,
0.523076923076923,0.538461538461538,0.553846153846154,0.569230769230769,
0.584615384615384,0.6,0.615384615384615,0.63076923076923,0.646153846153846,
0.661538461538461,0.676923076923076,0.692307692307692,0.707692307692307,
0.723076923076922,0.738461538461538,0.753846153846153,0.769230769230768,
0.784615384615384,0.799999999999999,0.815384615384614,0.83076923076923,
0.846153846153845,0.86153846153846,0.876923076923076,0.892307692307691,
0.907692307692306,0.923076923076922,0.938461538461537,0.953846153846152,
0.969230769230768,0.984615384615383,0.994228156739704),.UNSPECIFIED.)
CURVE()
GEOMETRIC_REPRESENTATION_ITEM()
RATIONAL_B_SPLINE_CURVE((1.,1.,1.,1.,1.,1.,1.,1.,1.,1.,1.,1.,1.,1.,1.,1.,
1.,1.,1.,1.,1.,1.,1.,1.,1.,1.,1.,1.,1.,1.,1.,1.,1.,1.,1.,1.,1.,1.,1.,1.,
1.,1.,1.,1.,1.,1.,1.,1.,1.,1.,1.,1.,1.,1.,1.,1.,1.,1.,1.,1.,1.,1.,1.,1.,
1.,1.,1.,1.,1.,1.))
REPRESENTATION_ITEM('')
);
#289=(
BOUNDED_CURVE()
B_SPLINE_CURVE(5,(#44475,#44476,#44477,#44478,#44479,#44480,#44481,#44482,
#44483,#44484,#44485,#44486,#44487,#44488,#44489,#44490,#44491,#44492,#44493,
#44494,#44495,#44496,#44497,#44498,#44499,#44500,#44501,#44502,#44503,#44504,
#44505,#44506,#44507,#44508,#44509,#44510,#44511,#44512,#44513,#44514,#44515,
#44516,#44517,#44518,#44519,#44520,#44521,#44522,#44523,#44524,#44525,#44526,
#44527,#44528,#44529,#44530,#44531,#44532,#44533,#44534,#44535,#44536,#44537,
#44538,#44539,#44540,#44541,#44542,#44543,#44544),.UNSPECIFIED.,.F.,.F.)
B_SPLINE_CURVE_WITH_KNOTS((6,1,1,1,1,1,1,1,1,1,1,1,1,1,1,1,1,1,1,1,1,1,
1,1,1,1,1,1,1,1,1,1,1,1,1,1,1,1,1,1,1,1,1,1,1,1,1,1,1,1,1,1,1,1,1,1,1,1,
1,1,1,1,1,1,1,6),(0.00577184337449692,0.0153846153846154,0.0307692307692308,
0.0461538461538462,0.0615384615384615,0.0769230769230769,0.0923076923076923,
0.107692307692308,0.123076923076923,0.138461538461538,0.153846153846154,
0.169230769230769,0.184615384615385,0.2,0.215384615384615,0.230769230769231,
0.246153846153846,0.261538461538462,0.276923076923077,0.292307692307692,
0.307692307692308,0.323076923076923,0.338461538461538,0.353846153846154,
0.369230769230769,0.384615384615385,0.4,0.415384615384615,0.430769230769231,
0.446153846153846,0.461538461538462,0.476923076923077,0.492307692307692,
0.507692307692308,0.523076923076923,0.538461538461538,0.553846153846154,
0.569230769230769,0.584615384615384,0.6,0.615384615384615,0.63076923076923,
0.646153846153846,0.661538461538461,0.676923076923076,0.692307692307692,
0.707692307692307,0.723076923076922,0.738461538461538,0.753846153846153,
0.769230769230768,0.784615384615384,0.799999999999999,0.815384615384614,
0.83076923076923,0.846153846153845,0.86153846153846,0.876923076923076,0.892307692307691,
0.907692307692306,0.923076923076922,0.938461538461537,0.953846153846152,
0.969230769230768,0.984615384615383,1.),.UNSPECIFIED.)
CURVE()
GEOMETRIC_REPRESENTATION_ITEM()
RATIONAL_B_SPLINE_CURVE((1.,1.,1.,1.,1.,1.,1.,1.,1.,1.,1.,1.,1.,1.,1.,1.,
1.,1.,1.,1.,1.,1.,1.,1.,1.,1.,1.,1.,1.,1.,1.,1.,1.,1.,1.,1.,1.,1.,1.,1.,
1.,1.,1.,1.,1.,1.,1.,1.,1.,1.,1.,1.,1.,1.,1.,1.,1.,1.,1.,1.,1.,1.,1.,1.,
1.,1.,1.,1.,1.,1.))
REPRESENTATION_ITEM('')
);
#290=(
BOUNDED_CURVE()
B_SPLINE_CURVE(5,(#44547,#44548,#44549,#44550,#44551,#44552,#44553,#44554,
#44555,#44556,#44557,#44558,#44559,#44560,#44561,#44562,#44563,#44564,#44565,
#44566,#44567,#44568,#44569,#44570,#44571,#44572,#44573,#44574,#44575,#44576,
#44577,#44578,#44579,#44580,#44581,#44582,#44583,#44584,#44585,#44586,#44587,
#44588,#44589,#44590,#44591,#44592,#44593,#44594,#44595,#44596,#44597,#44598,
#44599,#44600,#44601,#44602,#44603,#44604,#44605,#44606,#44607,#44608,#44609,
#44610,#44611,#44612,#44613,#44614,#44615,#44616),.UNSPECIFIED.,.F.,.F.)
B_SPLINE_CURVE_WITH_KNOTS((6,1,1,1,1,1,1,1,1,1,1,1,1,1,1,1,1,1,1,1,1,1,
1,1,1,1,1,1,1,1,1,1,1,1,1,1,1,1,1,1,1,1,1,1,1,1,1,1,1,1,1,1,1,1,1,1,1,1,
1,1,1,1,1,1,1,6),(0.,0.0153846153846154,0.0307692307692308,0.0461538461538462,
0.0615384615384615,0.0769230769230769,0.0923076923076923,0.107692307692308,
0.123076923076923,0.138461538461538,0.153846153846154,0.169230769230769,
0.184615384615385,0.2,0.215384615384615,0.230769230769231,0.246153846153846,
0.261538461538462,0.276923076923077,0.292307692307692,0.307692307692308,
0.323076923076923,0.338461538461538,0.353846153846154,0.369230769230769,
0.384615384615385,0.4,0.415384615384615,0.430769230769231,0.446153846153846,
0.461538461538462,0.476923076923077,0.492307692307692,0.507692307692308,
0.523076923076923,0.538461538461538,0.553846153846154,0.569230769230769,
0.584615384615384,0.6,0.615384615384615,0.63076923076923,0.646153846153846,
0.661538461538461,0.676923076923076,0.692307692307692,0.707692307692307,
0.723076923076922,0.738461538461538,0.753846153846153,0.769230769230768,
0.784615384615384,0.799999999999999,0.815384615384614,0.83076923076923,
0.846153846153845,0.86153846153846,0.876923076923076,0.892307692307691,
0.907692307692306,0.923076923076922,0.938461538461537,0.953846153846152,
0.969230769230768,0.984615384615383,0.994228156739723),.UNSPECIFIED.)
CURVE()
GEOMETRIC_REPRESENTATION_ITEM()
RATIONAL_B_SPLINE_CURVE((1.,1.,1.,1.,1.,1.,1.,1.,1.,1.,1.,1.,1.,1.,1.,1.,
1.,1.,1.,1.,1.,1.,1.,1.,1.,1.,1.,1.,1.,1.,1.,1.,1.,1.,1.,1.,1.,1.,1.,1.,
1.,1.,1.,1.,1.,1.,1.,1.,1.,1.,1.,1.,1.,1.,1.,1.,1.,1.,1.,1.,1.,1.,1.,1.,
1.,1.,1.,1.,1.,1.))
REPRESENTATION_ITEM('')
);
#291=(
BOUNDED_CURVE()
B_SPLINE_CURVE(5,(#44775,#44776,#44777,#44778,#44779,#44780,#44781,#44782,
#44783,#44784,#44785,#44786,#44787,#44788,#44789,#44790,#44791,#44792,#44793,
#44794,#44795,#44796,#44797,#44798,#44799,#44800,#44801,#44802,#44803,#44804,
#44805,#44806,#44807,#44808,#44809,#44810,#44811,#44812,#44813,#44814,#44815,
#44816,#44817,#44818,#44819,#44820,#44821,#44822,#44823,#44824,#44825,#44826,
#44827,#44828,#44829,#44830,#44831,#44832,#44833,#44834,#44835,#44836,#44837,
#44838,#44839,#44840,#44841,#44842,#44843,#44844),.UNSPECIFIED.,.F.,.F.)
B_SPLINE_CURVE_WITH_KNOTS((6,1,1,1,1,1,1,1,1,1,1,1,1,1,1,1,1,1,1,1,1,1,
1,1,1,1,1,1,1,1,1,1,1,1,1,1,1,1,1,1,1,1,1,1,1,1,1,1,1,1,1,1,1,1,1,1,1,1,
1,1,1,1,1,1,1,6),(-1.,-0.984615384615383,-0.969230769230768,-0.953846153846152,
-0.938461538461537,-0.923076923076922,-0.907692307692306,-0.892307692307691,
-0.876923076923076,-0.86153846153846,-0.846153846153845,-0.83076923076923,
-0.815384615384614,-0.799999999999999,-0.784615384615384,-0.769230769230768,
-0.753846153846153,-0.738461538461538,-0.723076923076922,-0.707692307692307,
-0.692307692307692,-0.676923076923076,-0.661538461538461,-0.646153846153846,
-0.63076923076923,-0.615384615384615,-0.6,-0.584615384615384,-0.569230769230769,
-0.553846153846154,-0.538461538461538,-0.523076923076923,-0.507692307692308,
-0.492307692307692,-0.476923076923077,-0.461538461538462,-0.446153846153846,
-0.430769230769231,-0.415384615384615,-0.4,-0.384615384615385,-0.369230769230769,
-0.353846153846154,-0.338461538461538,-0.323076923076923,-0.307692307692308,
-0.292307692307692,-0.276923076923077,-0.261538461538462,-0.246153846153846,
-0.230769230769231,-0.215384615384615,-0.2,-0.184615384615385,-0.169230769230769,
-0.153846153846154,-0.138461538461538,-0.123076923076923,-0.107692307692308,
-0.0923076923076923,-0.0769230769230769,-0.0615384615384615,-0.0461538461538462,
-0.0307692307692308,-0.0153846153846154,-0.00577184337448906),
 .UNSPECIFIED.)
CURVE()
GEOMETRIC_REPRESENTATION_ITEM()
RATIONAL_B_SPLINE_CURVE((1.,1.,1.,1.,1.,1.,1.,1.,1.,1.,1.,1.,1.,1.,1.,1.,
1.,1.,1.,1.,1.,1.,1.,1.,1.,1.,1.,1.,1.,1.,1.,1.,1.,1.,1.,1.,1.,1.,1.,1.,
1.,1.,1.,1.,1.,1.,1.,1.,1.,1.,1.,1.,1.,1.,1.,1.,1.,1.,1.,1.,1.,1.,1.,1.,
1.,1.,1.,1.,1.,1.))
REPRESENTATION_ITEM('')
);
#292=(
BOUNDED_CURVE()
B_SPLINE_CURVE(5,(#44995,#44996,#44997,#44998,#44999,#45000,#45001,#45002,
#45003,#45004,#45005,#45006,#45007,#45008,#45009,#45010,#45011,#45012,#45013,
#45014,#45015,#45016,#45017,#45018,#45019,#45020,#45021,#45022,#45023,#45024,
#45025,#45026,#45027,#45028,#45029,#45030,#45031,#45032,#45033,#45034,#45035,
#45036,#45037,#45038,#45039,#45040,#45041,#45042,#45043,#45044,#45045,#45046,
#45047,#45048,#45049,#45050,#45051,#45052,#45053,#45054,#45055,#45056,#45057,
#45058,#45059,#45060,#45061,#45062,#45063,#45064),.UNSPECIFIED.,.F.,.F.)
B_SPLINE_CURVE_WITH_KNOTS((6,1,1,1,1,1,1,1,1,1,1,1,1,1,1,1,1,1,1,1,1,1,
1,1,1,1,1,1,1,1,1,1,1,1,1,1,1,1,1,1,1,1,1,1,1,1,1,1,1,1,1,1,1,1,1,1,1,1,
1,1,1,1,1,1,1,6),(-0.994228156739728,-0.984615384615383,-0.969230769230768,
-0.953846153846152,-0.938461538461537,-0.923076923076922,-0.907692307692306,
-0.892307692307691,-0.876923076923076,-0.86153846153846,-0.846153846153845,
-0.83076923076923,-0.815384615384614,-0.799999999999999,-0.784615384615384,
-0.769230769230768,-0.753846153846153,-0.738461538461538,-0.723076923076922,
-0.707692307692307,-0.692307692307692,-0.676923076923076,-0.661538461538461,
-0.646153846153846,-0.63076923076923,-0.615384615384615,-0.6,-0.584615384615384,
-0.569230769230769,-0.553846153846154,-0.538461538461538,-0.523076923076923,
-0.507692307692308,-0.492307692307692,-0.476923076923077,-0.461538461538462,
-0.446153846153846,-0.430769230769231,-0.415384615384615,-0.4,-0.384615384615385,
-0.369230769230769,-0.353846153846154,-0.338461538461538,-0.323076923076923,
-0.307692307692308,-0.292307692307692,-0.276923076923077,-0.261538461538462,
-0.246153846153846,-0.230769230769231,-0.215384615384615,-0.2,-0.184615384615385,
-0.169230769230769,-0.153846153846154,-0.138461538461538,-0.123076923076923,
-0.107692307692308,-0.0923076923076923,-0.0769230769230769,-0.0615384615384615,
-0.0461538461538462,-0.0307692307692308,-0.0153846153846154,0.),
 .UNSPECIFIED.)
CURVE()
GEOMETRIC_REPRESENTATION_ITEM()
RATIONAL_B_SPLINE_CURVE((1.,1.,1.,1.,1.,1.,1.,1.,1.,1.,1.,1.,1.,1.,1.,1.,
1.,1.,1.,1.,1.,1.,1.,1.,1.,1.,1.,1.,1.,1.,1.,1.,1.,1.,1.,1.,1.,1.,1.,1.,
1.,1.,1.,1.,1.,1.,1.,1.,1.,1.,1.,1.,1.,1.,1.,1.,1.,1.,1.,1.,1.,1.,1.,1.,
1.,1.,1.,1.,1.,1.))
REPRESENTATION_ITEM('')
);
#293=(
BOUNDED_CURVE()
B_SPLINE_CURVE(5,(#45217,#45218,#45219,#45220,#45221,#45222,#45223,#45224,
#45225,#45226,#45227,#45228,#45229,#45230,#45231,#45232,#45233,#45234,#45235,
#45236,#45237,#45238,#45239,#45240,#45241,#45242,#45243,#45244,#45245,#45246,
#45247,#45248,#45249,#45250,#45251,#45252,#45253,#45254,#45255,#45256,#45257,
#45258,#45259,#45260,#45261,#45262,#45263,#45264,#45265,#45266,#45267,#45268,
#45269,#45270,#45271,#45272,#45273,#45274,#45275,#45276,#45277,#45278,#45279,
#45280,#45281,#45282,#45283,#45284,#45285,#45286),.UNSPECIFIED.,.F.,.F.)
B_SPLINE_CURVE_WITH_KNOTS((6,1,1,1,1,1,1,1,1,1,1,1,1,1,1,1,1,1,1,1,1,1,
1,1,1,1,1,1,1,1,1,1,1,1,1,1,1,1,1,1,1,1,1,1,1,1,1,1,1,1,1,1,1,1,1,1,1,1,
1,1,1,1,1,1,1,6),(-1.,-0.984615384615383,-0.969230769230768,-0.953846153846152,
-0.938461538461537,-0.923076923076922,-0.907692307692306,-0.892307692307691,
-0.876923076923076,-0.86153846153846,-0.846153846153845,-0.83076923076923,
-0.815384615384614,-0.799999999999999,-0.784615384615384,-0.769230769230768,
-0.753846153846153,-0.738461538461538,-0.723076923076922,-0.707692307692307,
-0.692307692307692,-0.676923076923076,-0.661538461538461,-0.646153846153846,
-0.63076923076923,-0.615384615384615,-0.6,-0.584615384615384,-0.569230769230769,
-0.553846153846154,-0.538461538461538,-0.523076923076923,-0.507692307692308,
-0.492307692307692,-0.476923076923077,-0.461538461538462,-0.446153846153846,
-0.430769230769231,-0.415384615384615,-0.4,-0.384615384615385,-0.369230769230769,
-0.353846153846154,-0.338461538461538,-0.323076923076923,-0.307692307692308,
-0.292307692307692,-0.276923076923077,-0.261538461538462,-0.246153846153846,
-0.230769230769231,-0.215384615384615,-0.2,-0.184615384615385,-0.169230769230769,
-0.153846153846154,-0.138461538461538,-0.123076923076923,-0.107692307692308,
-0.0923076923076923,-0.0769230769230769,-0.0615384615384615,-0.0461538461538462,
-0.0307692307692308,-0.0153846153846154,-0.0057718433744926),
 .UNSPECIFIED.)
CURVE()
GEOMETRIC_REPRESENTATION_ITEM()
RATIONAL_B_SPLINE_CURVE((1.,1.,1.,1.,1.,1.,1.,1.,1.,1.,1.,1.,1.,1.,1.,1.,
1.,1.,1.,1.,1.,1.,1.,1.,1.,1.,1.,1.,1.,1.,1.,1.,1.,1.,1.,1.,1.,1.,1.,1.,
1.,1.,1.,1.,1.,1.,1.,1.,1.,1.,1.,1.,1.,1.,1.,1.,1.,1.,1.,1.,1.,1.,1.,1.,
1.,1.,1.,1.,1.,1.))
REPRESENTATION_ITEM('')
);
#294=(
BOUNDED_CURVE()
B_SPLINE_CURVE(5,(#45437,#45438,#45439,#45440,#45441,#45442,#45443,#45444,
#45445,#45446,#45447,#45448,#45449,#45450,#45451,#45452,#45453,#45454,#45455,
#45456,#45457,#45458,#45459,#45460,#45461,#45462,#45463,#45464,#45465,#45466,
#45467,#45468,#45469,#45470,#45471,#45472,#45473,#45474,#45475,#45476,#45477,
#45478,#45479,#45480,#45481,#45482,#45483,#45484,#45485,#45486,#45487,#45488,
#45489,#45490,#45491,#45492,#45493,#45494,#45495,#45496,#45497,#45498,#45499,
#45500,#45501,#45502,#45503,#45504,#45505,#45506),.UNSPECIFIED.,.F.,.F.)
B_SPLINE_CURVE_WITH_KNOTS((6,1,1,1,1,1,1,1,1,1,1,1,1,1,1,1,1,1,1,1,1,1,
1,1,1,1,1,1,1,1,1,1,1,1,1,1,1,1,1,1,1,1,1,1,1,1,1,1,1,1,1,1,1,1,1,1,1,1,
1,1,1,1,1,1,1,6),(-0.994228156739718,-0.984615384615383,-0.969230769230768,
-0.953846153846152,-0.938461538461537,-0.923076923076922,-0.907692307692306,
-0.892307692307691,-0.876923076923076,-0.86153846153846,-0.846153846153845,
-0.83076923076923,-0.815384615384614,-0.799999999999999,-0.784615384615384,
-0.769230769230768,-0.753846153846153,-0.738461538461538,-0.723076923076922,
-0.707692307692307,-0.692307692307692,-0.676923076923076,-0.661538461538461,
-0.646153846153846,-0.63076923076923,-0.615384615384615,-0.6,-0.584615384615384,
-0.569230769230769,-0.553846153846154,-0.538461538461538,-0.523076923076923,
-0.507692307692308,-0.492307692307692,-0.476923076923077,-0.461538461538462,
-0.446153846153846,-0.430769230769231,-0.415384615384615,-0.4,-0.384615384615385,
-0.369230769230769,-0.353846153846154,-0.338461538461538,-0.323076923076923,
-0.307692307692308,-0.292307692307692,-0.276923076923077,-0.261538461538462,
-0.246153846153846,-0.230769230769231,-0.215384615384615,-0.2,-0.184615384615385,
-0.169230769230769,-0.153846153846154,-0.138461538461538,-0.123076923076923,
-0.107692307692308,-0.0923076923076923,-0.0769230769230769,-0.0615384615384615,
-0.0461538461538462,-0.0307692307692308,-0.0153846153846154,0.),
 .UNSPECIFIED.)
CURVE()
GEOMETRIC_REPRESENTATION_ITEM()
RATIONAL_B_SPLINE_CURVE((1.,1.,1.,1.,1.,1.,1.,1.,1.,1.,1.,1.,1.,1.,1.,1.,
1.,1.,1.,1.,1.,1.,1.,1.,1.,1.,1.,1.,1.,1.,1.,1.,1.,1.,1.,1.,1.,1.,1.,1.,
1.,1.,1.,1.,1.,1.,1.,1.,1.,1.,1.,1.,1.,1.,1.,1.,1.,1.,1.,1.,1.,1.,1.,1.,
1.,1.,1.,1.,1.,1.))
REPRESENTATION_ITEM('')
);
#295=(
BOUNDED_CURVE()
B_SPLINE_CURVE(5,(#45659,#45660,#45661,#45662,#45663,#45664,#45665,#45666,
#45667,#45668,#45669,#45670,#45671,#45672,#45673,#45674,#45675,#45676,#45677,
#45678,#45679,#45680,#45681,#45682,#45683,#45684,#45685,#45686,#45687,#45688,
#45689,#45690,#45691,#45692,#45693,#45694,#45695,#45696,#45697,#45698,#45699,
#45700,#45701,#45702,#45703,#45704,#45705,#45706,#45707,#45708,#45709,#45710,
#45711,#45712,#45713,#45714,#45715,#45716,#45717,#45718,#45719,#45720,#45721,
#45722,#45723,#45724,#45725,#45726,#45727,#45728),.UNSPECIFIED.,.F.,.F.)
B_SPLINE_CURVE_WITH_KNOTS((6,1,1,1,1,1,1,1,1,1,1,1,1,1,1,1,1,1,1,1,1,1,
1,1,1,1,1,1,1,1,1,1,1,1,1,1,1,1,1,1,1,1,1,1,1,1,1,1,1,1,1,1,1,1,1,1,1,1,
1,1,1,1,1,1,1,6),(-1.,-0.984615384615383,-0.969230769230768,-0.953846153846152,
-0.938461538461537,-0.923076923076922,-0.907692307692306,-0.892307692307691,
-0.876923076923076,-0.86153846153846,-0.846153846153845,-0.83076923076923,
-0.815384615384614,-0.799999999999999,-0.784615384615384,-0.769230769230768,
-0.753846153846153,-0.738461538461538,-0.723076923076922,-0.707692307692307,
-0.692307692307692,-0.676923076923076,-0.661538461538461,-0.646153846153846,
-0.63076923076923,-0.615384615384615,-0.6,-0.584615384615384,-0.569230769230769,
-0.553846153846154,-0.538461538461538,-0.523076923076923,-0.507692307692308,
-0.492307692307692,-0.476923076923077,-0.461538461538462,-0.446153846153846,
-0.430769230769231,-0.415384615384615,-0.4,-0.384615384615385,-0.369230769230769,
-0.353846153846154,-0.338461538461538,-0.323076923076923,-0.307692307692308,
-0.292307692307692,-0.276923076923077,-0.261538461538462,-0.246153846153846,
-0.230769230769231,-0.215384615384615,-0.2,-0.184615384615385,-0.169230769230769,
-0.153846153846154,-0.138461538461538,-0.123076923076923,-0.107692307692308,
-0.0923076923076923,-0.0769230769230769,-0.0615384615384615,-0.0461538461538462,
-0.0307692307692308,-0.0153846153846154,-0.00577184337449396),
 .UNSPECIFIED.)
CURVE()
GEOMETRIC_REPRESENTATION_ITEM()
RATIONAL_B_SPLINE_CURVE((1.,1.,1.,1.,1.,1.,1.,1.,1.,1.,1.,1.,1.,1.,1.,1.,
1.,1.,1.,1.,1.,1.,1.,1.,1.,1.,1.,1.,1.,1.,1.,1.,1.,1.,1.,1.,1.,1.,1.,1.,
1.,1.,1.,1.,1.,1.,1.,1.,1.,1.,1.,1.,1.,1.,1.,1.,1.,1.,1.,1.,1.,1.,1.,1.,
1.,1.,1.,1.,1.,1.))
REPRESENTATION_ITEM('')
);
#296=(
BOUNDED_CURVE()
B_SPLINE_CURVE(5,(#45879,#45880,#45881,#45882,#45883,#45884,#45885,#45886,
#45887,#45888,#45889,#45890,#45891,#45892,#45893,#45894,#45895,#45896,#45897,
#45898,#45899,#45900,#45901,#45902,#45903,#45904,#45905,#45906,#45907,#45908,
#45909,#45910,#45911,#45912,#45913,#45914,#45915,#45916,#45917,#45918,#45919,
#45920,#45921,#45922,#45923,#45924,#45925,#45926,#45927,#45928,#45929,#45930,
#45931,#45932,#45933,#45934,#45935,#45936,#45937,#45938,#45939,#45940,#45941,
#45942,#45943,#45944,#45945,#45946,#45947,#45948),.UNSPECIFIED.,.F.,.F.)
B_SPLINE_CURVE_WITH_KNOTS((6,1,1,1,1,1,1,1,1,1,1,1,1,1,1,1,1,1,1,1,1,1,
1,1,1,1,1,1,1,1,1,1,1,1,1,1,1,1,1,1,1,1,1,1,1,1,1,1,1,1,1,1,1,1,1,1,1,1,
1,1,1,1,1,1,1,6),(-0.994228156739702,-0.984615384615383,-0.969230769230768,
-0.953846153846152,-0.938461538461537,-0.923076923076922,-0.907692307692306,
-0.892307692307691,-0.876923076923076,-0.86153846153846,-0.846153846153845,
-0.83076923076923,-0.815384615384614,-0.799999999999999,-0.784615384615384,
-0.769230769230768,-0.753846153846153,-0.738461538461538,-0.723076923076922,
-0.707692307692307,-0.692307692307692,-0.676923076923076,-0.661538461538461,
-0.646153846153846,-0.63076923076923,-0.615384615384615,-0.6,-0.584615384615384,
-0.569230769230769,-0.553846153846154,-0.538461538461538,-0.523076923076923,
-0.507692307692308,-0.492307692307692,-0.476923076923077,-0.461538461538462,
-0.446153846153846,-0.430769230769231,-0.415384615384615,-0.4,-0.384615384615385,
-0.369230769230769,-0.353846153846154,-0.338461538461538,-0.323076923076923,
-0.307692307692308,-0.292307692307692,-0.276923076923077,-0.261538461538462,
-0.246153846153846,-0.230769230769231,-0.215384615384615,-0.2,-0.184615384615385,
-0.169230769230769,-0.153846153846154,-0.138461538461538,-0.123076923076923,
-0.107692307692308,-0.0923076923076923,-0.0769230769230769,-0.0615384615384615,
-0.0461538461538462,-0.0307692307692308,-0.0153846153846154,0.),
 .UNSPECIFIED.)
CURVE()
GEOMETRIC_REPRESENTATION_ITEM()
RATIONAL_B_SPLINE_CURVE((1.,1.,1.,1.,1.,1.,1.,1.,1.,1.,1.,1.,1.,1.,1.,1.,
1.,1.,1.,1.,1.,1.,1.,1.,1.,1.,1.,1.,1.,1.,1.,1.,1.,1.,1.,1.,1.,1.,1.,1.,
1.,1.,1.,1.,1.,1.,1.,1.,1.,1.,1.,1.,1.,1.,1.,1.,1.,1.,1.,1.,1.,1.,1.,1.,
1.,1.,1.,1.,1.,1.))
REPRESENTATION_ITEM('')
);
#297=(
BOUNDED_CURVE()
B_SPLINE_CURVE(5,(#46101,#46102,#46103,#46104,#46105,#46106,#46107,#46108,
#46109,#46110,#46111,#46112,#46113,#46114,#46115,#46116,#46117,#46118,#46119,
#46120,#46121,#46122,#46123,#46124,#46125,#46126,#46127,#46128,#46129,#46130,
#46131,#46132,#46133,#46134,#46135,#46136,#46137,#46138,#46139,#46140,#46141,
#46142,#46143,#46144,#46145,#46146,#46147,#46148,#46149,#46150,#46151,#46152,
#46153,#46154,#46155,#46156,#46157,#46158,#46159,#46160,#46161,#46162,#46163,
#46164,#46165,#46166,#46167,#46168,#46169,#46170),.UNSPECIFIED.,.F.,.F.)
B_SPLINE_CURVE_WITH_KNOTS((6,1,1,1,1,1,1,1,1,1,1,1,1,1,1,1,1,1,1,1,1,1,
1,1,1,1,1,1,1,1,1,1,1,1,1,1,1,1,1,1,1,1,1,1,1,1,1,1,1,1,1,1,1,1,1,1,1,1,
1,1,1,1,1,1,1,6),(-1.,-0.984615384615383,-0.969230769230768,-0.953846153846152,
-0.938461538461537,-0.923076923076922,-0.907692307692306,-0.892307692307691,
-0.876923076923076,-0.86153846153846,-0.846153846153845,-0.83076923076923,
-0.815384615384614,-0.799999999999999,-0.784615384615384,-0.769230769230768,
-0.753846153846153,-0.738461538461538,-0.723076923076922,-0.707692307692307,
-0.692307692307692,-0.676923076923076,-0.661538461538461,-0.646153846153846,
-0.63076923076923,-0.615384615384615,-0.6,-0.584615384615384,-0.569230769230769,
-0.553846153846154,-0.538461538461538,-0.523076923076923,-0.507692307692308,
-0.492307692307692,-0.476923076923077,-0.461538461538462,-0.446153846153846,
-0.430769230769231,-0.415384615384615,-0.4,-0.384615384615385,-0.369230769230769,
-0.353846153846154,-0.338461538461538,-0.323076923076923,-0.307692307692308,
-0.292307692307692,-0.276923076923077,-0.261538461538462,-0.246153846153846,
-0.230769230769231,-0.215384615384615,-0.2,-0.184615384615385,-0.169230769230769,
-0.153846153846154,-0.138461538461538,-0.123076923076923,-0.107692307692308,
-0.0923076923076923,-0.0769230769230769,-0.0615384615384615,-0.0461538461538462,
-0.0307692307692308,-0.0153846153846154,-0.00577184337450989),
 .UNSPECIFIED.)
CURVE()
GEOMETRIC_REPRESENTATION_ITEM()
RATIONAL_B_SPLINE_CURVE((1.,1.,1.,1.,1.,1.,1.,1.,1.,1.,1.,1.,1.,1.,1.,1.,
1.,1.,1.,1.,1.,1.,1.,1.,1.,1.,1.,1.,1.,1.,1.,1.,1.,1.,1.,1.,1.,1.,1.,1.,
1.,1.,1.,1.,1.,1.,1.,1.,1.,1.,1.,1.,1.,1.,1.,1.,1.,1.,1.,1.,1.,1.,1.,1.,
1.,1.,1.,1.,1.,1.))
REPRESENTATION_ITEM('')
);
#298=(
BOUNDED_CURVE()
B_SPLINE_CURVE(5,(#46321,#46322,#46323,#46324,#46325,#46326,#46327,#46328,
#46329,#46330,#46331,#46332,#46333,#46334,#46335,#46336,#46337,#46338,#46339,
#46340,#46341,#46342,#46343,#46344,#46345,#46346,#46347,#46348,#46349,#46350,
#46351,#46352,#46353,#46354,#46355,#46356,#46357,#46358,#46359,#46360,#46361,
#46362,#46363,#46364,#46365,#46366,#46367,#46368,#46369,#46370,#46371,#46372,
#46373,#46374,#46375,#46376,#46377,#46378,#46379,#46380,#46381,#46382,#46383,
#46384,#46385,#46386,#46387,#46388,#46389,#46390),.UNSPECIFIED.,.F.,.F.)
B_SPLINE_CURVE_WITH_KNOTS((6,1,1,1,1,1,1,1,1,1,1,1,1,1,1,1,1,1,1,1,1,1,
1,1,1,1,1,1,1,1,1,1,1,1,1,1,1,1,1,1,1,1,1,1,1,1,1,1,1,1,1,1,1,1,1,1,1,1,
1,1,1,1,1,1,1,6),(-0.994228156739736,-0.984615384615383,-0.969230769230768,
-0.953846153846152,-0.938461538461537,-0.923076923076922,-0.907692307692306,
-0.892307692307691,-0.876923076923076,-0.86153846153846,-0.846153846153845,
-0.83076923076923,-0.815384615384614,-0.799999999999999,-0.784615384615384,
-0.769230769230768,-0.753846153846153,-0.738461538461538,-0.723076923076922,
-0.707692307692307,-0.692307692307692,-0.676923076923076,-0.661538461538461,
-0.646153846153846,-0.63076923076923,-0.615384615384615,-0.6,-0.584615384615384,
-0.569230769230769,-0.553846153846154,-0.538461538461538,-0.523076923076923,
-0.507692307692308,-0.492307692307692,-0.476923076923077,-0.461538461538462,
-0.446153846153846,-0.430769230769231,-0.415384615384615,-0.4,-0.384615384615385,
-0.369230769230769,-0.353846153846154,-0.338461538461538,-0.323076923076923,
-0.307692307692308,-0.292307692307692,-0.276923076923077,-0.261538461538462,
-0.246153846153846,-0.230769230769231,-0.215384615384615,-0.2,-0.184615384615385,
-0.169230769230769,-0.153846153846154,-0.138461538461538,-0.123076923076923,
-0.107692307692308,-0.0923076923076923,-0.0769230769230769,-0.0615384615384615,
-0.0461538461538462,-0.0307692307692308,-0.0153846153846154,0.),
 .UNSPECIFIED.)
CURVE()
GEOMETRIC_REPRESENTATION_ITEM()
RATIONAL_B_SPLINE_CURVE((1.,1.,1.,1.,1.,1.,1.,1.,1.,1.,1.,1.,1.,1.,1.,1.,
1.,1.,1.,1.,1.,1.,1.,1.,1.,1.,1.,1.,1.,1.,1.,1.,1.,1.,1.,1.,1.,1.,1.,1.,
1.,1.,1.,1.,1.,1.,1.,1.,1.,1.,1.,1.,1.,1.,1.,1.,1.,1.,1.,1.,1.,1.,1.,1.,
1.,1.,1.,1.,1.,1.))
REPRESENTATION_ITEM('')
);
#299=(
BOUNDED_CURVE()
B_SPLINE_CURVE(5,(#46543,#46544,#46545,#46546,#46547,#46548,#46549,#46550,
#46551,#46552,#46553,#46554,#46555,#46556,#46557,#46558,#46559,#46560,#46561,
#46562,#46563,#46564,#46565,#46566,#46567,#46568,#46569,#46570,#46571,#46572,
#46573,#46574,#46575,#46576,#46577,#46578,#46579,#46580,#46581,#46582,#46583,
#46584,#46585,#46586,#46587,#46588,#46589,#46590,#46591,#46592,#46593,#46594,
#46595,#46596,#46597,#46598,#46599,#46600,#46601,#46602,#46603,#46604,#46605,
#46606,#46607,#46608,#46609,#46610,#46611,#46612),.UNSPECIFIED.,.F.,.F.)
B_SPLINE_CURVE_WITH_KNOTS((6,1,1,1,1,1,1,1,1,1,1,1,1,1,1,1,1,1,1,1,1,1,
1,1,1,1,1,1,1,1,1,1,1,1,1,1,1,1,1,1,1,1,1,1,1,1,1,1,1,1,1,1,1,1,1,1,1,1,
1,1,1,1,1,1,1,6),(-1.,-0.984615384615383,-0.969230769230768,-0.953846153846152,
-0.938461538461537,-0.923076923076922,-0.907692307692306,-0.892307692307691,
-0.876923076923076,-0.86153846153846,-0.846153846153845,-0.83076923076923,
-0.815384615384614,-0.799999999999999,-0.784615384615384,-0.769230769230768,
-0.753846153846153,-0.738461538461538,-0.723076923076922,-0.707692307692307,
-0.692307692307692,-0.676923076923076,-0.661538461538461,-0.646153846153846,
-0.63076923076923,-0.615384615384615,-0.6,-0.584615384615384,-0.569230769230769,
-0.553846153846154,-0.538461538461538,-0.523076923076923,-0.507692307692308,
-0.492307692307692,-0.476923076923077,-0.461538461538462,-0.446153846153846,
-0.430769230769231,-0.415384615384615,-0.4,-0.384615384615385,-0.369230769230769,
-0.353846153846154,-0.338461538461538,-0.323076923076923,-0.307692307692308,
-0.292307692307692,-0.276923076923077,-0.261538461538462,-0.246153846153846,
-0.230769230769231,-0.215384615384615,-0.2,-0.184615384615385,-0.169230769230769,
-0.153846153846154,-0.138461538461538,-0.123076923076923,-0.107692307692308,
-0.0923076923076923,-0.0769230769230769,-0.0615384615384615,-0.0461538461538462,
-0.0307692307692308,-0.0153846153846154,-0.00577184337452469),
 .UNSPECIFIED.)
CURVE()
GEOMETRIC_REPRESENTATION_ITEM()
RATIONAL_B_SPLINE_CURVE((1.,1.,1.,1.,1.,1.,1.,1.,1.,1.,1.,1.,1.,1.,1.,1.,
1.,1.,1.,1.,1.,1.,1.,1.,1.,1.,1.,1.,1.,1.,1.,1.,1.,1.,1.,1.,1.,1.,1.,1.,
1.,1.,1.,1.,1.,1.,1.,1.,1.,1.,1.,1.,1.,1.,1.,1.,1.,1.,1.,1.,1.,1.,1.,1.,
1.,1.,1.,1.,1.,1.))
REPRESENTATION_ITEM('')
);
#300=(
BOUNDED_CURVE()
B_SPLINE_CURVE(5,(#46763,#46764,#46765,#46766,#46767,#46768,#46769,#46770,
#46771,#46772,#46773,#46774,#46775,#46776,#46777,#46778,#46779,#46780,#46781,
#46782,#46783,#46784,#46785,#46786,#46787,#46788,#46789,#46790,#46791,#46792,
#46793,#46794,#46795,#46796,#46797,#46798,#46799,#46800,#46801,#46802,#46803,
#46804,#46805,#46806,#46807,#46808,#46809,#46810,#46811,#46812,#46813,#46814,
#46815,#46816,#46817,#46818,#46819,#46820,#46821,#46822,#46823,#46824,#46825,
#46826,#46827,#46828,#46829,#46830,#46831,#46832),.UNSPECIFIED.,.F.,.F.)
B_SPLINE_CURVE_WITH_KNOTS((6,1,1,1,1,1,1,1,1,1,1,1,1,1,1,1,1,1,1,1,1,1,
1,1,1,1,1,1,1,1,1,1,1,1,1,1,1,1,1,1,1,1,1,1,1,1,1,1,1,1,1,1,1,1,1,1,1,1,
1,1,1,1,1,1,1,6),(-0.994228156739717,-0.984615384615383,-0.969230769230768,
-0.953846153846152,-0.938461538461537,-0.923076923076922,-0.907692307692306,
-0.892307692307691,-0.876923076923076,-0.86153846153846,-0.846153846153845,
-0.83076923076923,-0.815384615384614,-0.799999999999999,-0.784615384615384,
-0.769230769230768,-0.753846153846153,-0.738461538461538,-0.723076923076922,
-0.707692307692307,-0.692307692307692,-0.676923076923076,-0.661538461538461,
-0.646153846153846,-0.63076923076923,-0.615384615384615,-0.6,-0.584615384615384,
-0.569230769230769,-0.553846153846154,-0.538461538461538,-0.523076923076923,
-0.507692307692308,-0.492307692307692,-0.476923076923077,-0.461538461538462,
-0.446153846153846,-0.430769230769231,-0.415384615384615,-0.4,-0.384615384615385,
-0.369230769230769,-0.353846153846154,-0.338461538461538,-0.323076923076923,
-0.307692307692308,-0.292307692307692,-0.276923076923077,-0.261538461538462,
-0.246153846153846,-0.230769230769231,-0.215384615384615,-0.2,-0.184615384615385,
-0.169230769230769,-0.153846153846154,-0.138461538461538,-0.123076923076923,
-0.107692307692308,-0.0923076923076923,-0.0769230769230769,-0.0615384615384615,
-0.0461538461538462,-0.0307692307692308,-0.0153846153846154,0.),
 .UNSPECIFIED.)
CURVE()
GEOMETRIC_REPRESENTATION_ITEM()
RATIONAL_B_SPLINE_CURVE((1.,1.,1.,1.,1.,1.,1.,1.,1.,1.,1.,1.,1.,1.,1.,1.,
1.,1.,1.,1.,1.,1.,1.,1.,1.,1.,1.,1.,1.,1.,1.,1.,1.,1.,1.,1.,1.,1.,1.,1.,
1.,1.,1.,1.,1.,1.,1.,1.,1.,1.,1.,1.,1.,1.,1.,1.,1.,1.,1.,1.,1.,1.,1.,1.,
1.,1.,1.,1.,1.,1.))
REPRESENTATION_ITEM('')
);
#301=(
BOUNDED_CURVE()
B_SPLINE_CURVE(5,(#46985,#46986,#46987,#46988,#46989,#46990,#46991,#46992,
#46993,#46994,#46995,#46996,#46997,#46998,#46999,#47000,#47001,#47002,#47003,
#47004,#47005,#47006,#47007,#47008,#47009,#47010,#47011,#47012,#47013,#47014,
#47015,#47016,#47017,#47018,#47019,#47020,#47021,#47022,#47023,#47024,#47025,
#47026,#47027,#47028,#47029,#47030,#47031,#47032,#47033,#47034,#47035,#47036,
#47037,#47038,#47039,#47040,#47041,#47042,#47043,#47044,#47045,#47046,#47047,
#47048,#47049,#47050,#47051,#47052,#47053,#47054),.UNSPECIFIED.,.F.,.F.)
B_SPLINE_CURVE_WITH_KNOTS((6,1,1,1,1,1,1,1,1,1,1,1,1,1,1,1,1,1,1,1,1,1,
1,1,1,1,1,1,1,1,1,1,1,1,1,1,1,1,1,1,1,1,1,1,1,1,1,1,1,1,1,1,1,1,1,1,1,1,
1,1,1,1,1,1,1,6),(-1.,-0.984615384615383,-0.969230769230768,-0.953846153846152,
-0.938461538461537,-0.923076923076922,-0.907692307692306,-0.892307692307691,
-0.876923076923076,-0.86153846153846,-0.846153846153845,-0.83076923076923,
-0.815384615384614,-0.799999999999999,-0.784615384615384,-0.769230769230768,
-0.753846153846153,-0.738461538461538,-0.723076923076922,-0.707692307692307,
-0.692307692307692,-0.676923076923076,-0.661538461538461,-0.646153846153846,
-0.63076923076923,-0.615384615384615,-0.6,-0.584615384615384,-0.569230769230769,
-0.553846153846154,-0.538461538461538,-0.523076923076923,-0.507692307692308,
-0.492307692307692,-0.476923076923077,-0.461538461538462,-0.446153846153846,
-0.430769230769231,-0.415384615384615,-0.4,-0.384615384615385,-0.369230769230769,
-0.353846153846154,-0.338461538461538,-0.323076923076923,-0.307692307692308,
-0.292307692307692,-0.276923076923077,-0.261538461538462,-0.246153846153846,
-0.230769230769231,-0.215384615384615,-0.2,-0.184615384615385,-0.169230769230769,
-0.153846153846154,-0.138461538461538,-0.123076923076923,-0.107692307692308,
-0.0923076923076923,-0.0769230769230769,-0.0615384615384615,-0.0461538461538462,
-0.0307692307692308,-0.0153846153846154,-0.00577184337453472),
 .UNSPECIFIED.)
CURVE()
GEOMETRIC_REPRESENTATION_ITEM()
RATIONAL_B_SPLINE_CURVE((1.,1.,1.,1.,1.,1.,1.,1.,1.,1.,1.,1.,1.,1.,1.,1.,
1.,1.,1.,1.,1.,1.,1.,1.,1.,1.,1.,1.,1.,1.,1.,1.,1.,1.,1.,1.,1.,1.,1.,1.,
1.,1.,1.,1.,1.,1.,1.,1.,1.,1.,1.,1.,1.,1.,1.,1.,1.,1.,1.,1.,1.,1.,1.,1.,
1.,1.,1.,1.,1.,1.))
REPRESENTATION_ITEM('')
);
#302=(
BOUNDED_CURVE()
B_SPLINE_CURVE(5,(#47205,#47206,#47207,#47208,#47209,#47210,#47211,#47212,
#47213,#47214,#47215,#47216,#47217,#47218,#47219,#47220,#47221,#47222,#47223,
#47224,#47225,#47226,#47227,#47228,#47229,#47230,#47231,#47232,#47233,#47234,
#47235,#47236,#47237,#47238,#47239,#47240,#47241,#47242,#47243,#47244,#47245,
#47246,#47247,#47248,#47249,#47250,#47251,#47252,#47253,#47254,#47255,#47256,
#47257,#47258,#47259,#47260,#47261,#47262,#47263,#47264,#47265,#47266,#47267,
#47268,#47269,#47270,#47271,#47272,#47273,#47274),.UNSPECIFIED.,.F.,.F.)
B_SPLINE_CURVE_WITH_KNOTS((6,1,1,1,1,1,1,1,1,1,1,1,1,1,1,1,1,1,1,1,1,1,
1,1,1,1,1,1,1,1,1,1,1,1,1,1,1,1,1,1,1,1,1,1,1,1,1,1,1,1,1,1,1,1,1,1,1,1,
1,1,1,1,1,1,1,6),(-0.994228156739652,-0.984615384615383,-0.969230769230768,
-0.953846153846152,-0.938461538461537,-0.923076923076922,-0.907692307692306,
-0.892307692307691,-0.876923076923076,-0.86153846153846,-0.846153846153845,
-0.83076923076923,-0.815384615384614,-0.799999999999999,-0.784615384615384,
-0.769230769230768,-0.753846153846153,-0.738461538461538,-0.723076923076922,
-0.707692307692307,-0.692307692307692,-0.676923076923076,-0.661538461538461,
-0.646153846153846,-0.63076923076923,-0.615384615384615,-0.6,-0.584615384615384,
-0.569230769230769,-0.553846153846154,-0.538461538461538,-0.523076923076923,
-0.507692307692308,-0.492307692307692,-0.476923076923077,-0.461538461538462,
-0.446153846153846,-0.430769230769231,-0.415384615384615,-0.4,-0.384615384615385,
-0.369230769230769,-0.353846153846154,-0.338461538461538,-0.323076923076923,
-0.307692307692308,-0.292307692307692,-0.276923076923077,-0.261538461538462,
-0.246153846153846,-0.230769230769231,-0.215384615384615,-0.2,-0.184615384615385,
-0.169230769230769,-0.153846153846154,-0.138461538461538,-0.123076923076923,
-0.107692307692308,-0.0923076923076923,-0.0769230769230769,-0.0615384615384615,
-0.0461538461538462,-0.0307692307692308,-0.0153846153846154,0.),
 .UNSPECIFIED.)
CURVE()
GEOMETRIC_REPRESENTATION_ITEM()
RATIONAL_B_SPLINE_CURVE((1.,1.,1.,1.,1.,1.,1.,1.,1.,1.,1.,1.,1.,1.,1.,1.,
1.,1.,1.,1.,1.,1.,1.,1.,1.,1.,1.,1.,1.,1.,1.,1.,1.,1.,1.,1.,1.,1.,1.,1.,
1.,1.,1.,1.,1.,1.,1.,1.,1.,1.,1.,1.,1.,1.,1.,1.,1.,1.,1.,1.,1.,1.,1.,1.,
1.,1.,1.,1.,1.,1.))
REPRESENTATION_ITEM('')
);
#303=(
BOUNDED_CURVE()
B_SPLINE_CURVE(5,(#47427,#47428,#47429,#47430,#47431,#47432,#47433,#47434,
#47435,#47436,#47437,#47438,#47439,#47440,#47441,#47442,#47443,#47444,#47445,
#47446,#47447,#47448,#47449,#47450,#47451,#47452,#47453,#47454,#47455,#47456,
#47457,#47458,#47459,#47460,#47461,#47462,#47463,#47464,#47465,#47466,#47467,
#47468,#47469,#47470,#47471,#47472,#47473,#47474,#47475,#47476,#47477,#47478,
#47479,#47480,#47481,#47482,#47483,#47484,#47485,#47486,#47487,#47488,#47489,
#47490,#47491,#47492,#47493,#47494,#47495,#47496),.UNSPECIFIED.,.F.,.F.)
B_SPLINE_CURVE_WITH_KNOTS((6,1,1,1,1,1,1,1,1,1,1,1,1,1,1,1,1,1,1,1,1,1,
1,1,1,1,1,1,1,1,1,1,1,1,1,1,1,1,1,1,1,1,1,1,1,1,1,1,1,1,1,1,1,1,1,1,1,1,
1,1,1,1,1,1,1,6),(-1.,-0.984615384615383,-0.969230769230768,-0.953846153846152,
-0.938461538461537,-0.923076923076922,-0.907692307692306,-0.892307692307691,
-0.876923076923076,-0.86153846153846,-0.846153846153845,-0.83076923076923,
-0.815384615384614,-0.799999999999999,-0.784615384615384,-0.769230769230768,
-0.753846153846153,-0.738461538461538,-0.723076923076922,-0.707692307692307,
-0.692307692307692,-0.676923076923076,-0.661538461538461,-0.646153846153846,
-0.63076923076923,-0.615384615384615,-0.6,-0.584615384615384,-0.569230769230769,
-0.553846153846154,-0.538461538461538,-0.523076923076923,-0.507692307692308,
-0.492307692307692,-0.476923076923077,-0.461538461538462,-0.446153846153846,
-0.430769230769231,-0.415384615384615,-0.4,-0.384615384615385,-0.369230769230769,
-0.353846153846154,-0.338461538461538,-0.323076923076923,-0.307692307692308,
-0.292307692307692,-0.276923076923077,-0.261538461538462,-0.246153846153846,
-0.230769230769231,-0.215384615384615,-0.2,-0.184615384615385,-0.169230769230769,
-0.153846153846154,-0.138461538461538,-0.123076923076923,-0.107692307692308,
-0.0923076923076923,-0.0769230769230769,-0.0615384615384615,-0.0461538461538462,
-0.0307692307692308,-0.0153846153846154,-0.00577184337450876),
 .UNSPECIFIED.)
CURVE()
GEOMETRIC_REPRESENTATION_ITEM()
RATIONAL_B_SPLINE_CURVE((1.,1.,1.,1.,1.,1.,1.,1.,1.,1.,1.,1.,1.,1.,1.,1.,
1.,1.,1.,1.,1.,1.,1.,1.,1.,1.,1.,1.,1.,1.,1.,1.,1.,1.,1.,1.,1.,1.,1.,1.,
1.,1.,1.,1.,1.,1.,1.,1.,1.,1.,1.,1.,1.,1.,1.,1.,1.,1.,1.,1.,1.,1.,1.,1.,
1.,1.,1.,1.,1.,1.))
REPRESENTATION_ITEM('')
);
#304=(
BOUNDED_CURVE()
B_SPLINE_CURVE(5,(#47647,#47648,#47649,#47650,#47651,#47652,#47653,#47654,
#47655,#47656,#47657,#47658,#47659,#47660,#47661,#47662,#47663,#47664,#47665,
#47666,#47667,#47668,#47669,#47670,#47671,#47672,#47673,#47674,#47675,#47676,
#47677,#47678,#47679,#47680,#47681,#47682,#47683,#47684,#47685,#47686,#47687,
#47688,#47689,#47690,#47691,#47692,#47693,#47694,#47695,#47696,#47697,#47698,
#47699,#47700,#47701,#47702,#47703,#47704,#47705,#47706,#47707,#47708,#47709,
#47710,#47711,#47712,#47713,#47714,#47715,#47716),.UNSPECIFIED.,.F.,.F.)
B_SPLINE_CURVE_WITH_KNOTS((6,1,1,1,1,1,1,1,1,1,1,1,1,1,1,1,1,1,1,1,1,1,
1,1,1,1,1,1,1,1,1,1,1,1,1,1,1,1,1,1,1,1,1,1,1,1,1,1,1,1,1,1,1,1,1,1,1,1,
1,1,1,1,1,1,1,6),(-0.994228156739683,-0.984615384615383,-0.969230769230768,
-0.953846153846152,-0.938461538461537,-0.923076923076922,-0.907692307692306,
-0.892307692307691,-0.876923076923076,-0.86153846153846,-0.846153846153845,
-0.83076923076923,-0.815384615384614,-0.799999999999999,-0.784615384615384,
-0.769230769230768,-0.753846153846153,-0.738461538461538,-0.723076923076922,
-0.707692307692307,-0.692307692307692,-0.676923076923076,-0.661538461538461,
-0.646153846153846,-0.63076923076923,-0.615384615384615,-0.6,-0.584615384615384,
-0.569230769230769,-0.553846153846154,-0.538461538461538,-0.523076923076923,
-0.507692307692308,-0.492307692307692,-0.476923076923077,-0.461538461538462,
-0.446153846153846,-0.430769230769231,-0.415384615384615,-0.4,-0.384615384615385,
-0.369230769230769,-0.353846153846154,-0.338461538461538,-0.323076923076923,
-0.307692307692308,-0.292307692307692,-0.276923076923077,-0.261538461538462,
-0.246153846153846,-0.230769230769231,-0.215384615384615,-0.2,-0.184615384615385,
-0.169230769230769,-0.153846153846154,-0.138461538461538,-0.123076923076923,
-0.107692307692308,-0.0923076923076923,-0.0769230769230769,-0.0615384615384615,
-0.0461538461538462,-0.0307692307692308,-0.0153846153846154,0.),
 .UNSPECIFIED.)
CURVE()
GEOMETRIC_REPRESENTATION_ITEM()
RATIONAL_B_SPLINE_CURVE((1.,1.,1.,1.,1.,1.,1.,1.,1.,1.,1.,1.,1.,1.,1.,1.,
1.,1.,1.,1.,1.,1.,1.,1.,1.,1.,1.,1.,1.,1.,1.,1.,1.,1.,1.,1.,1.,1.,1.,1.,
1.,1.,1.,1.,1.,1.,1.,1.,1.,1.,1.,1.,1.,1.,1.,1.,1.,1.,1.,1.,1.,1.,1.,1.,
1.,1.,1.,1.,1.,1.))
REPRESENTATION_ITEM('')
);
#305=(
BOUNDED_CURVE()
B_SPLINE_CURVE(5,(#47869,#47870,#47871,#47872,#47873,#47874,#47875,#47876,
#47877,#47878,#47879,#47880,#47881,#47882,#47883,#47884,#47885,#47886,#47887,
#47888,#47889,#47890,#47891,#47892,#47893,#47894,#47895,#47896,#47897,#47898,
#47899,#47900,#47901,#47902,#47903,#47904,#47905,#47906,#47907,#47908,#47909,
#47910,#47911,#47912,#47913,#47914,#47915,#47916,#47917,#47918,#47919,#47920,
#47921,#47922,#47923,#47924,#47925,#47926,#47927,#47928,#47929,#47930,#47931,
#47932,#47933,#47934,#47935,#47936,#47937,#47938),.UNSPECIFIED.,.F.,.F.)
B_SPLINE_CURVE_WITH_KNOTS((6,1,1,1,1,1,1,1,1,1,1,1,1,1,1,1,1,1,1,1,1,1,
1,1,1,1,1,1,1,1,1,1,1,1,1,1,1,1,1,1,1,1,1,1,1,1,1,1,1,1,1,1,1,1,1,1,1,1,
1,1,1,1,1,1,1,6),(-1.,-0.984615384615383,-0.969230769230768,-0.953846153846152,
-0.938461538461537,-0.923076923076922,-0.907692307692306,-0.892307692307691,
-0.876923076923076,-0.86153846153846,-0.846153846153845,-0.83076923076923,
-0.815384615384614,-0.799999999999999,-0.784615384615384,-0.769230769230768,
-0.753846153846153,-0.738461538461538,-0.723076923076922,-0.707692307692307,
-0.692307692307692,-0.676923076923076,-0.661538461538461,-0.646153846153846,
-0.63076923076923,-0.615384615384615,-0.6,-0.584615384615384,-0.569230769230769,
-0.553846153846154,-0.538461538461538,-0.523076923076923,-0.507692307692308,
-0.492307692307692,-0.476923076923077,-0.461538461538462,-0.446153846153846,
-0.430769230769231,-0.415384615384615,-0.4,-0.384615384615385,-0.369230769230769,
-0.353846153846154,-0.338461538461538,-0.323076923076923,-0.307692307692308,
-0.292307692307692,-0.276923076923077,-0.261538461538462,-0.246153846153846,
-0.230769230769231,-0.215384615384615,-0.2,-0.184615384615385,-0.169230769230769,
-0.153846153846154,-0.138461538461538,-0.123076923076923,-0.107692307692308,
-0.0923076923076923,-0.0769230769230769,-0.0615384615384615,-0.0461538461538462,
-0.0307692307692308,-0.0153846153846154,-0.00577184337450277),
 .UNSPECIFIED.)
CURVE()
GEOMETRIC_REPRESENTATION_ITEM()
RATIONAL_B_SPLINE_CURVE((1.,1.,1.,1.,1.,1.,1.,1.,1.,1.,1.,1.,1.,1.,1.,1.,
1.,1.,1.,1.,1.,1.,1.,1.,1.,1.,1.,1.,1.,1.,1.,1.,1.,1.,1.,1.,1.,1.,1.,1.,
1.,1.,1.,1.,1.,1.,1.,1.,1.,1.,1.,1.,1.,1.,1.,1.,1.,1.,1.,1.,1.,1.,1.,1.,
1.,1.,1.,1.,1.,1.))
REPRESENTATION_ITEM('')
);
#306=(
BOUNDED_CURVE()
B_SPLINE_CURVE(5,(#48089,#48090,#48091,#48092,#48093,#48094,#48095,#48096,
#48097,#48098,#48099,#48100,#48101,#48102,#48103,#48104,#48105,#48106,#48107,
#48108,#48109,#48110,#48111,#48112,#48113,#48114,#48115,#48116,#48117,#48118,
#48119,#48120,#48121,#48122,#48123,#48124,#48125,#48126,#48127,#48128,#48129,
#48130,#48131,#48132,#48133,#48134,#48135,#48136,#48137,#48138,#48139,#48140,
#48141,#48142,#48143,#48144,#48145,#48146,#48147,#48148,#48149,#48150,#48151,
#48152,#48153,#48154,#48155,#48156,#48157,#48158),.UNSPECIFIED.,.F.,.F.)
B_SPLINE_CURVE_WITH_KNOTS((6,1,1,1,1,1,1,1,1,1,1,1,1,1,1,1,1,1,1,1,1,1,
1,1,1,1,1,1,1,1,1,1,1,1,1,1,1,1,1,1,1,1,1,1,1,1,1,1,1,1,1,1,1,1,1,1,1,1,
1,1,1,1,1,1,1,6),(-0.994228156739689,-0.984615384615383,-0.969230769230768,
-0.953846153846152,-0.938461538461537,-0.923076923076922,-0.907692307692306,
-0.892307692307691,-0.876923076923076,-0.86153846153846,-0.846153846153845,
-0.83076923076923,-0.815384615384614,-0.799999999999999,-0.784615384615384,
-0.769230769230768,-0.753846153846153,-0.738461538461538,-0.723076923076922,
-0.707692307692307,-0.692307692307692,-0.676923076923076,-0.661538461538461,
-0.646153846153846,-0.63076923076923,-0.615384615384615,-0.6,-0.584615384615384,
-0.569230769230769,-0.553846153846154,-0.538461538461538,-0.523076923076923,
-0.507692307692308,-0.492307692307692,-0.476923076923077,-0.461538461538462,
-0.446153846153846,-0.430769230769231,-0.415384615384615,-0.4,-0.384615384615385,
-0.369230769230769,-0.353846153846154,-0.338461538461538,-0.323076923076923,
-0.307692307692308,-0.292307692307692,-0.276923076923077,-0.261538461538462,
-0.246153846153846,-0.230769230769231,-0.215384615384615,-0.2,-0.184615384615385,
-0.169230769230769,-0.153846153846154,-0.138461538461538,-0.123076923076923,
-0.107692307692308,-0.0923076923076923,-0.0769230769230769,-0.0615384615384615,
-0.0461538461538462,-0.0307692307692308,-0.0153846153846154,0.),
 .UNSPECIFIED.)
CURVE()
GEOMETRIC_REPRESENTATION_ITEM()
RATIONAL_B_SPLINE_CURVE((1.,1.,1.,1.,1.,1.,1.,1.,1.,1.,1.,1.,1.,1.,1.,1.,
1.,1.,1.,1.,1.,1.,1.,1.,1.,1.,1.,1.,1.,1.,1.,1.,1.,1.,1.,1.,1.,1.,1.,1.,
1.,1.,1.,1.,1.,1.,1.,1.,1.,1.,1.,1.,1.,1.,1.,1.,1.,1.,1.,1.,1.,1.,1.,1.,
1.,1.,1.,1.,1.,1.))
REPRESENTATION_ITEM('')
);
#307=(
BOUNDED_CURVE()
B_SPLINE_CURVE(5,(#48311,#48312,#48313,#48314,#48315,#48316,#48317,#48318,
#48319,#48320,#48321,#48322,#48323,#48324,#48325,#48326,#48327,#48328,#48329,
#48330,#48331,#48332,#48333,#48334,#48335,#48336,#48337,#48338,#48339,#48340,
#48341,#48342,#48343,#48344,#48345,#48346,#48347,#48348,#48349,#48350,#48351,
#48352,#48353,#48354,#48355,#48356,#48357,#48358,#48359,#48360,#48361,#48362,
#48363,#48364,#48365,#48366,#48367,#48368,#48369,#48370,#48371,#48372,#48373,
#48374,#48375,#48376,#48377,#48378,#48379,#48380),.UNSPECIFIED.,.F.,.F.)
B_SPLINE_CURVE_WITH_KNOTS((6,1,1,1,1,1,1,1,1,1,1,1,1,1,1,1,1,1,1,1,1,1,
1,1,1,1,1,1,1,1,1,1,1,1,1,1,1,1,1,1,1,1,1,1,1,1,1,1,1,1,1,1,1,1,1,1,1,1,
1,1,1,1,1,1,1,6),(-1.,-0.984615384615383,-0.969230769230768,-0.953846153846152,
-0.938461538461537,-0.923076923076922,-0.907692307692306,-0.892307692307691,
-0.876923076923076,-0.86153846153846,-0.846153846153845,-0.83076923076923,
-0.815384615384614,-0.799999999999999,-0.784615384615384,-0.769230769230768,
-0.753846153846153,-0.738461538461538,-0.723076923076922,-0.707692307692307,
-0.692307692307692,-0.676923076923076,-0.661538461538461,-0.646153846153846,
-0.63076923076923,-0.615384615384615,-0.6,-0.584615384615384,-0.569230769230769,
-0.553846153846154,-0.538461538461538,-0.523076923076923,-0.507692307692308,
-0.492307692307692,-0.476923076923077,-0.461538461538462,-0.446153846153846,
-0.430769230769231,-0.415384615384615,-0.4,-0.384615384615385,-0.369230769230769,
-0.353846153846154,-0.338461538461538,-0.323076923076923,-0.307692307692308,
-0.292307692307692,-0.276923076923077,-0.261538461538462,-0.246153846153846,
-0.230769230769231,-0.215384615384615,-0.2,-0.184615384615385,-0.169230769230769,
-0.153846153846154,-0.138461538461538,-0.123076923076923,-0.107692307692308,
-0.0923076923076923,-0.0769230769230769,-0.0615384615384615,-0.0461538461538462,
-0.0307692307692308,-0.0153846153846154,-0.00577184337451766),
 .UNSPECIFIED.)
CURVE()
GEOMETRIC_REPRESENTATION_ITEM()
RATIONAL_B_SPLINE_CURVE((1.,1.,1.,1.,1.,1.,1.,1.,1.,1.,1.,1.,1.,1.,1.,1.,
1.,1.,1.,1.,1.,1.,1.,1.,1.,1.,1.,1.,1.,1.,1.,1.,1.,1.,1.,1.,1.,1.,1.,1.,
1.,1.,1.,1.,1.,1.,1.,1.,1.,1.,1.,1.,1.,1.,1.,1.,1.,1.,1.,1.,1.,1.,1.,1.,
1.,1.,1.,1.,1.,1.))
REPRESENTATION_ITEM('')
);
#308=(
BOUNDED_CURVE()
B_SPLINE_CURVE(5,(#48531,#48532,#48533,#48534,#48535,#48536,#48537,#48538,
#48539,#48540,#48541,#48542,#48543,#48544,#48545,#48546,#48547,#48548,#48549,
#48550,#48551,#48552,#48553,#48554,#48555,#48556,#48557,#48558,#48559,#48560,
#48561,#48562,#48563,#48564,#48565,#48566,#48567,#48568,#48569,#48570,#48571,
#48572,#48573,#48574,#48575,#48576,#48577,#48578,#48579,#48580,#48581,#48582,
#48583,#48584,#48585,#48586,#48587,#48588,#48589,#48590,#48591,#48592,#48593,
#48594,#48595,#48596,#48597,#48598,#48599,#48600),.UNSPECIFIED.,.F.,.F.)
B_SPLINE_CURVE_WITH_KNOTS((6,1,1,1,1,1,1,1,1,1,1,1,1,1,1,1,1,1,1,1,1,1,
1,1,1,1,1,1,1,1,1,1,1,1,1,1,1,1,1,1,1,1,1,1,1,1,1,1,1,1,1,1,1,1,1,1,1,1,
1,1,1,1,1,1,1,6),(-0.994228156739687,-0.984615384615383,-0.969230769230768,
-0.953846153846152,-0.938461538461537,-0.923076923076922,-0.907692307692306,
-0.892307692307691,-0.876923076923076,-0.86153846153846,-0.846153846153845,
-0.83076923076923,-0.815384615384614,-0.799999999999999,-0.784615384615384,
-0.769230769230768,-0.753846153846153,-0.738461538461538,-0.723076923076922,
-0.707692307692307,-0.692307692307692,-0.676923076923076,-0.661538461538461,
-0.646153846153846,-0.63076923076923,-0.615384615384615,-0.6,-0.584615384615384,
-0.569230769230769,-0.553846153846154,-0.538461538461538,-0.523076923076923,
-0.507692307692308,-0.492307692307692,-0.476923076923077,-0.461538461538462,
-0.446153846153846,-0.430769230769231,-0.415384615384615,-0.4,-0.384615384615385,
-0.369230769230769,-0.353846153846154,-0.338461538461538,-0.323076923076923,
-0.307692307692308,-0.292307692307692,-0.276923076923077,-0.261538461538462,
-0.246153846153846,-0.230769230769231,-0.215384615384615,-0.2,-0.184615384615385,
-0.169230769230769,-0.153846153846154,-0.138461538461538,-0.123076923076923,
-0.107692307692308,-0.0923076923076923,-0.0769230769230769,-0.0615384615384615,
-0.0461538461538462,-0.0307692307692308,-0.0153846153846154,0.),
 .UNSPECIFIED.)
CURVE()
GEOMETRIC_REPRESENTATION_ITEM()
RATIONAL_B_SPLINE_CURVE((1.,1.,1.,1.,1.,1.,1.,1.,1.,1.,1.,1.,1.,1.,1.,1.,
1.,1.,1.,1.,1.,1.,1.,1.,1.,1.,1.,1.,1.,1.,1.,1.,1.,1.,1.,1.,1.,1.,1.,1.,
1.,1.,1.,1.,1.,1.,1.,1.,1.,1.,1.,1.,1.,1.,1.,1.,1.,1.,1.,1.,1.,1.,1.,1.,
1.,1.,1.,1.,1.,1.))
REPRESENTATION_ITEM('')
);
#309=(
BOUNDED_CURVE()
B_SPLINE_CURVE(5,(#48753,#48754,#48755,#48756,#48757,#48758,#48759,#48760,
#48761,#48762,#48763,#48764,#48765,#48766,#48767,#48768,#48769,#48770,#48771,
#48772,#48773,#48774,#48775,#48776,#48777,#48778,#48779,#48780,#48781,#48782,
#48783,#48784,#48785,#48786,#48787,#48788,#48789,#48790,#48791,#48792,#48793,
#48794,#48795,#48796,#48797,#48798,#48799,#48800,#48801,#48802,#48803,#48804,
#48805,#48806,#48807,#48808,#48809,#48810,#48811,#48812,#48813,#48814,#48815,
#48816,#48817,#48818,#48819,#48820,#48821,#48822),.UNSPECIFIED.,.F.,.F.)
B_SPLINE_CURVE_WITH_KNOTS((6,1,1,1,1,1,1,1,1,1,1,1,1,1,1,1,1,1,1,1,1,1,
1,1,1,1,1,1,1,1,1,1,1,1,1,1,1,1,1,1,1,1,1,1,1,1,1,1,1,1,1,1,1,1,1,1,1,1,
1,1,1,1,1,1,1,6),(-1.,-0.984615384615383,-0.969230769230768,-0.953846153846152,
-0.938461538461537,-0.923076923076922,-0.907692307692306,-0.892307692307691,
-0.876923076923076,-0.86153846153846,-0.846153846153845,-0.83076923076923,
-0.815384615384614,-0.799999999999999,-0.784615384615384,-0.769230769230768,
-0.753846153846153,-0.738461538461538,-0.723076923076922,-0.707692307692307,
-0.692307692307692,-0.676923076923076,-0.661538461538461,-0.646153846153846,
-0.63076923076923,-0.615384615384615,-0.6,-0.584615384615384,-0.569230769230769,
-0.553846153846154,-0.538461538461538,-0.523076923076923,-0.507692307692308,
-0.492307692307692,-0.476923076923077,-0.461538461538462,-0.446153846153846,
-0.430769230769231,-0.415384615384615,-0.4,-0.384615384615385,-0.369230769230769,
-0.353846153846154,-0.338461538461538,-0.323076923076923,-0.307692307692308,
-0.292307692307692,-0.276923076923077,-0.261538461538462,-0.246153846153846,
-0.230769230769231,-0.215384615384615,-0.2,-0.184615384615385,-0.169230769230769,
-0.153846153846154,-0.138461538461538,-0.123076923076923,-0.107692307692308,
-0.0923076923076923,-0.0769230769230769,-0.0615384615384615,-0.0461538461538462,
-0.0307692307692308,-0.0153846153846154,-0.00577184337452512),
 .UNSPECIFIED.)
CURVE()
GEOMETRIC_REPRESENTATION_ITEM()
RATIONAL_B_SPLINE_CURVE((1.,1.,1.,1.,1.,1.,1.,1.,1.,1.,1.,1.,1.,1.,1.,1.,
1.,1.,1.,1.,1.,1.,1.,1.,1.,1.,1.,1.,1.,1.,1.,1.,1.,1.,1.,1.,1.,1.,1.,1.,
1.,1.,1.,1.,1.,1.,1.,1.,1.,1.,1.,1.,1.,1.,1.,1.,1.,1.,1.,1.,1.,1.,1.,1.,
1.,1.,1.,1.,1.,1.))
REPRESENTATION_ITEM('')
);
#310=(
BOUNDED_CURVE()
B_SPLINE_CURVE(5,(#48973,#48974,#48975,#48976,#48977,#48978,#48979,#48980,
#48981,#48982,#48983,#48984,#48985,#48986,#48987,#48988,#48989,#48990,#48991,
#48992,#48993,#48994,#48995,#48996,#48997,#48998,#48999,#49000,#49001,#49002,
#49003,#49004,#49005,#49006,#49007,#49008,#49009,#49010,#49011,#49012,#49013,
#49014,#49015,#49016,#49017,#49018,#49019,#49020,#49021,#49022,#49023,#49024,
#49025,#49026,#49027,#49028,#49029,#49030,#49031,#49032,#49033,#49034,#49035,
#49036,#49037,#49038,#49039,#49040,#49041,#49042),.UNSPECIFIED.,.F.,.F.)
B_SPLINE_CURVE_WITH_KNOTS((6,1,1,1,1,1,1,1,1,1,1,1,1,1,1,1,1,1,1,1,1,1,
1,1,1,1,1,1,1,1,1,1,1,1,1,1,1,1,1,1,1,1,1,1,1,1,1,1,1,1,1,1,1,1,1,1,1,1,
1,1,1,1,1,1,1,6),(-0.994228156739691,-0.984615384615383,-0.969230769230768,
-0.953846153846152,-0.938461538461537,-0.923076923076922,-0.907692307692306,
-0.892307692307691,-0.876923076923076,-0.86153846153846,-0.846153846153845,
-0.83076923076923,-0.815384615384614,-0.799999999999999,-0.784615384615384,
-0.769230769230768,-0.753846153846153,-0.738461538461538,-0.723076923076922,
-0.707692307692307,-0.692307692307692,-0.676923076923076,-0.661538461538461,
-0.646153846153846,-0.63076923076923,-0.615384615384615,-0.6,-0.584615384615384,
-0.569230769230769,-0.553846153846154,-0.538461538461538,-0.523076923076923,
-0.507692307692308,-0.492307692307692,-0.476923076923077,-0.461538461538462,
-0.446153846153846,-0.430769230769231,-0.415384615384615,-0.4,-0.384615384615385,
-0.369230769230769,-0.353846153846154,-0.338461538461538,-0.323076923076923,
-0.307692307692308,-0.292307692307692,-0.276923076923077,-0.261538461538462,
-0.246153846153846,-0.230769230769231,-0.215384615384615,-0.2,-0.184615384615385,
-0.169230769230769,-0.153846153846154,-0.138461538461538,-0.123076923076923,
-0.107692307692308,-0.0923076923076923,-0.0769230769230769,-0.0615384615384615,
-0.0461538461538462,-0.0307692307692308,-0.0153846153846154,0.),
 .UNSPECIFIED.)
CURVE()
GEOMETRIC_REPRESENTATION_ITEM()
RATIONAL_B_SPLINE_CURVE((1.,1.,1.,1.,1.,1.,1.,1.,1.,1.,1.,1.,1.,1.,1.,1.,
1.,1.,1.,1.,1.,1.,1.,1.,1.,1.,1.,1.,1.,1.,1.,1.,1.,1.,1.,1.,1.,1.,1.,1.,
1.,1.,1.,1.,1.,1.,1.,1.,1.,1.,1.,1.,1.,1.,1.,1.,1.,1.,1.,1.,1.,1.,1.,1.,
1.,1.,1.,1.,1.,1.))
REPRESENTATION_ITEM('')
);
#311=(
BOUNDED_CURVE()
B_SPLINE_CURVE(5,(#49195,#49196,#49197,#49198,#49199,#49200,#49201,#49202,
#49203,#49204,#49205,#49206,#49207,#49208,#49209,#49210,#49211,#49212,#49213,
#49214,#49215,#49216,#49217,#49218,#49219,#49220,#49221,#49222,#49223,#49224,
#49225,#49226,#49227,#49228,#49229,#49230,#49231,#49232,#49233,#49234,#49235,
#49236,#49237,#49238,#49239,#49240,#49241,#49242,#49243,#49244,#49245,#49246,
#49247,#49248,#49249,#49250,#49251,#49252,#49253,#49254,#49255,#49256,#49257,
#49258,#49259,#49260,#49261,#49262,#49263,#49264),.UNSPECIFIED.,.F.,.F.)
B_SPLINE_CURVE_WITH_KNOTS((6,1,1,1,1,1,1,1,1,1,1,1,1,1,1,1,1,1,1,1,1,1,
1,1,1,1,1,1,1,1,1,1,1,1,1,1,1,1,1,1,1,1,1,1,1,1,1,1,1,1,1,1,1,1,1,1,1,1,
1,1,1,1,1,1,1,6),(-1.,-0.984615384615383,-0.969230769230768,-0.953846153846152,
-0.938461538461537,-0.923076923076922,-0.907692307692306,-0.892307692307691,
-0.876923076923076,-0.86153846153846,-0.846153846153845,-0.83076923076923,
-0.815384615384614,-0.799999999999999,-0.784615384615384,-0.769230769230768,
-0.753846153846153,-0.738461538461538,-0.723076923076922,-0.707692307692307,
-0.692307692307692,-0.676923076923076,-0.661538461538461,-0.646153846153846,
-0.63076923076923,-0.615384615384615,-0.6,-0.584615384615384,-0.569230769230769,
-0.553846153846154,-0.538461538461538,-0.523076923076923,-0.507692307692308,
-0.492307692307692,-0.476923076923077,-0.461538461538462,-0.446153846153846,
-0.430769230769231,-0.415384615384615,-0.4,-0.384615384615385,-0.369230769230769,
-0.353846153846154,-0.338461538461538,-0.323076923076923,-0.307692307692308,
-0.292307692307692,-0.276923076923077,-0.261538461538462,-0.246153846153846,
-0.230769230769231,-0.215384615384615,-0.2,-0.184615384615385,-0.169230769230769,
-0.153846153846154,-0.138461538461538,-0.123076923076923,-0.107692307692308,
-0.0923076923076923,-0.0769230769230769,-0.0615384615384615,-0.0461538461538462,
-0.0307692307692308,-0.0153846153846154,-0.00577184337448448),
 .UNSPECIFIED.)
CURVE()
GEOMETRIC_REPRESENTATION_ITEM()
RATIONAL_B_SPLINE_CURVE((1.,1.,1.,1.,1.,1.,1.,1.,1.,1.,1.,1.,1.,1.,1.,1.,
1.,1.,1.,1.,1.,1.,1.,1.,1.,1.,1.,1.,1.,1.,1.,1.,1.,1.,1.,1.,1.,1.,1.,1.,
1.,1.,1.,1.,1.,1.,1.,1.,1.,1.,1.,1.,1.,1.,1.,1.,1.,1.,1.,1.,1.,1.,1.,1.,
1.,1.,1.,1.,1.,1.))
REPRESENTATION_ITEM('')
);
#312=(
BOUNDED_CURVE()
B_SPLINE_CURVE(5,(#49415,#49416,#49417,#49418,#49419,#49420,#49421,#49422,
#49423,#49424,#49425,#49426,#49427,#49428,#49429,#49430,#49431,#49432,#49433,
#49434,#49435,#49436,#49437,#49438,#49439,#49440,#49441,#49442,#49443,#49444,
#49445,#49446,#49447,#49448,#49449,#49450,#49451,#49452,#49453,#49454,#49455,
#49456,#49457,#49458,#49459,#49460,#49461,#49462,#49463,#49464,#49465,#49466,
#49467,#49468,#49469,#49470,#49471,#49472,#49473,#49474,#49475,#49476,#49477,
#49478,#49479,#49480,#49481,#49482,#49483,#49484),.UNSPECIFIED.,.F.,.F.)
B_SPLINE_CURVE_WITH_KNOTS((6,1,1,1,1,1,1,1,1,1,1,1,1,1,1,1,1,1,1,1,1,1,
1,1,1,1,1,1,1,1,1,1,1,1,1,1,1,1,1,1,1,1,1,1,1,1,1,1,1,1,1,1,1,1,1,1,1,1,
1,1,1,1,1,1,1,6),(-0.99422815673972,-0.984615384615383,-0.969230769230768,
-0.953846153846152,-0.938461538461537,-0.923076923076922,-0.907692307692306,
-0.892307692307691,-0.876923076923076,-0.86153846153846,-0.846153846153845,
-0.83076923076923,-0.815384615384614,-0.799999999999999,-0.784615384615384,
-0.769230769230768,-0.753846153846153,-0.738461538461538,-0.723076923076922,
-0.707692307692307,-0.692307692307692,-0.676923076923076,-0.661538461538461,
-0.646153846153846,-0.63076923076923,-0.615384615384615,-0.6,-0.584615384615384,
-0.569230769230769,-0.553846153846154,-0.538461538461538,-0.523076923076923,
-0.507692307692308,-0.492307692307692,-0.476923076923077,-0.461538461538462,
-0.446153846153846,-0.430769230769231,-0.415384615384615,-0.4,-0.384615384615385,
-0.369230769230769,-0.353846153846154,-0.338461538461538,-0.323076923076923,
-0.307692307692308,-0.292307692307692,-0.276923076923077,-0.261538461538462,
-0.246153846153846,-0.230769230769231,-0.215384615384615,-0.2,-0.184615384615385,
-0.169230769230769,-0.153846153846154,-0.138461538461538,-0.123076923076923,
-0.107692307692308,-0.0923076923076923,-0.0769230769230769,-0.0615384615384615,
-0.0461538461538462,-0.0307692307692308,-0.0153846153846154,0.),
 .UNSPECIFIED.)
CURVE()
GEOMETRIC_REPRESENTATION_ITEM()
RATIONAL_B_SPLINE_CURVE((1.,1.,1.,1.,1.,1.,1.,1.,1.,1.,1.,1.,1.,1.,1.,1.,
1.,1.,1.,1.,1.,1.,1.,1.,1.,1.,1.,1.,1.,1.,1.,1.,1.,1.,1.,1.,1.,1.,1.,1.,
1.,1.,1.,1.,1.,1.,1.,1.,1.,1.,1.,1.,1.,1.,1.,1.,1.,1.,1.,1.,1.,1.,1.,1.,
1.,1.,1.,1.,1.,1.))
REPRESENTATION_ITEM('')
);
#313=(
BOUNDED_CURVE()
B_SPLINE_CURVE(5,(#49637,#49638,#49639,#49640,#49641,#49642,#49643,#49644,
#49645,#49646,#49647,#49648,#49649,#49650,#49651,#49652,#49653,#49654,#49655,
#49656,#49657,#49658,#49659,#49660,#49661,#49662,#49663,#49664,#49665,#49666,
#49667,#49668,#49669,#49670,#49671,#49672,#49673,#49674,#49675,#49676,#49677,
#49678,#49679,#49680,#49681,#49682,#49683,#49684,#49685,#49686,#49687,#49688,
#49689,#49690,#49691,#49692,#49693,#49694,#49695,#49696,#49697,#49698,#49699,
#49700,#49701,#49702,#49703,#49704,#49705,#49706),.UNSPECIFIED.,.F.,.F.)
B_SPLINE_CURVE_WITH_KNOTS((6,1,1,1,1,1,1,1,1,1,1,1,1,1,1,1,1,1,1,1,1,1,
1,1,1,1,1,1,1,1,1,1,1,1,1,1,1,1,1,1,1,1,1,1,1,1,1,1,1,1,1,1,1,1,1,1,1,1,
1,1,1,1,1,1,1,6),(-1.,-0.984615384615383,-0.969230769230768,-0.953846153846152,
-0.938461538461537,-0.923076923076922,-0.907692307692306,-0.892307692307691,
-0.876923076923076,-0.86153846153846,-0.846153846153845,-0.83076923076923,
-0.815384615384614,-0.799999999999999,-0.784615384615384,-0.769230769230768,
-0.753846153846153,-0.738461538461538,-0.723076923076922,-0.707692307692307,
-0.692307692307692,-0.676923076923076,-0.661538461538461,-0.646153846153846,
-0.63076923076923,-0.615384615384615,-0.6,-0.584615384615384,-0.569230769230769,
-0.553846153846154,-0.538461538461538,-0.523076923076923,-0.507692307692308,
-0.492307692307692,-0.476923076923077,-0.461538461538462,-0.446153846153846,
-0.430769230769231,-0.415384615384615,-0.4,-0.384615384615385,-0.369230769230769,
-0.353846153846154,-0.338461538461538,-0.323076923076923,-0.307692307692308,
-0.292307692307692,-0.276923076923077,-0.261538461538462,-0.246153846153846,
-0.230769230769231,-0.215384615384615,-0.2,-0.184615384615385,-0.169230769230769,
-0.153846153846154,-0.138461538461538,-0.123076923076923,-0.107692307692308,
-0.0923076923076923,-0.0769230769230769,-0.0615384615384615,-0.0461538461538462,
-0.0307692307692308,-0.0153846153846154,-0.00577184337448251),
 .UNSPECIFIED.)
CURVE()
GEOMETRIC_REPRESENTATION_ITEM()
RATIONAL_B_SPLINE_CURVE((1.,1.,1.,1.,1.,1.,1.,1.,1.,1.,1.,1.,1.,1.,1.,1.,
1.,1.,1.,1.,1.,1.,1.,1.,1.,1.,1.,1.,1.,1.,1.,1.,1.,1.,1.,1.,1.,1.,1.,1.,
1.,1.,1.,1.,1.,1.,1.,1.,1.,1.,1.,1.,1.,1.,1.,1.,1.,1.,1.,1.,1.,1.,1.,1.,
1.,1.,1.,1.,1.,1.))
REPRESENTATION_ITEM('')
);
#314=(
BOUNDED_CURVE()
B_SPLINE_CURVE(5,(#49857,#49858,#49859,#49860,#49861,#49862,#49863,#49864,
#49865,#49866,#49867,#49868,#49869,#49870,#49871,#49872,#49873,#49874,#49875,
#49876,#49877,#49878,#49879,#49880,#49881,#49882,#49883,#49884,#49885,#49886,
#49887,#49888,#49889,#49890,#49891,#49892,#49893,#49894,#49895,#49896,#49897,
#49898,#49899,#49900,#49901,#49902,#49903,#49904,#49905,#49906,#49907,#49908,
#49909,#49910,#49911,#49912,#49913,#49914,#49915,#49916,#49917,#49918,#49919,
#49920,#49921,#49922,#49923,#49924,#49925,#49926),.UNSPECIFIED.,.F.,.F.)
B_SPLINE_CURVE_WITH_KNOTS((6,1,1,1,1,1,1,1,1,1,1,1,1,1,1,1,1,1,1,1,1,1,
1,1,1,1,1,1,1,1,1,1,1,1,1,1,1,1,1,1,1,1,1,1,1,1,1,1,1,1,1,1,1,1,1,1,1,1,
1,1,1,1,1,1,1,6),(-0.994228156739703,-0.984615384615383,-0.969230769230768,
-0.953846153846152,-0.938461538461537,-0.923076923076922,-0.907692307692306,
-0.892307692307691,-0.876923076923076,-0.86153846153846,-0.846153846153845,
-0.83076923076923,-0.815384615384614,-0.799999999999999,-0.784615384615384,
-0.769230769230768,-0.753846153846153,-0.738461538461538,-0.723076923076922,
-0.707692307692307,-0.692307692307692,-0.676923076923076,-0.661538461538461,
-0.646153846153846,-0.63076923076923,-0.615384615384615,-0.6,-0.584615384615384,
-0.569230769230769,-0.553846153846154,-0.538461538461538,-0.523076923076923,
-0.507692307692308,-0.492307692307692,-0.476923076923077,-0.461538461538462,
-0.446153846153846,-0.430769230769231,-0.415384615384615,-0.4,-0.384615384615385,
-0.369230769230769,-0.353846153846154,-0.338461538461538,-0.323076923076923,
-0.307692307692308,-0.292307692307692,-0.276923076923077,-0.261538461538462,
-0.246153846153846,-0.230769230769231,-0.215384615384615,-0.2,-0.184615384615385,
-0.169230769230769,-0.153846153846154,-0.138461538461538,-0.123076923076923,
-0.107692307692308,-0.0923076923076923,-0.0769230769230769,-0.0615384615384615,
-0.0461538461538462,-0.0307692307692308,-0.0153846153846154,0.),
 .UNSPECIFIED.)
CURVE()
GEOMETRIC_REPRESENTATION_ITEM()
RATIONAL_B_SPLINE_CURVE((1.,1.,1.,1.,1.,1.,1.,1.,1.,1.,1.,1.,1.,1.,1.,1.,
1.,1.,1.,1.,1.,1.,1.,1.,1.,1.,1.,1.,1.,1.,1.,1.,1.,1.,1.,1.,1.,1.,1.,1.,
1.,1.,1.,1.,1.,1.,1.,1.,1.,1.,1.,1.,1.,1.,1.,1.,1.,1.,1.,1.,1.,1.,1.,1.,
1.,1.,1.,1.,1.,1.))
REPRESENTATION_ITEM('')
);
#315=(
BOUNDED_CURVE()
B_SPLINE_CURVE(5,(#50079,#50080,#50081,#50082,#50083,#50084,#50085,#50086,
#50087,#50088,#50089,#50090,#50091,#50092,#50093,#50094,#50095,#50096,#50097,
#50098,#50099,#50100,#50101,#50102,#50103,#50104,#50105,#50106,#50107,#50108,
#50109,#50110,#50111,#50112,#50113,#50114,#50115,#50116,#50117,#50118,#50119,
#50120,#50121,#50122,#50123,#50124,#50125,#50126,#50127,#50128,#50129,#50130,
#50131,#50132,#50133,#50134,#50135,#50136,#50137,#50138,#50139,#50140,#50141,
#50142,#50143,#50144,#50145,#50146,#50147,#50148),.UNSPECIFIED.,.F.,.F.)
B_SPLINE_CURVE_WITH_KNOTS((6,1,1,1,1,1,1,1,1,1,1,1,1,1,1,1,1,1,1,1,1,1,
1,1,1,1,1,1,1,1,1,1,1,1,1,1,1,1,1,1,1,1,1,1,1,1,1,1,1,1,1,1,1,1,1,1,1,1,
1,1,1,1,1,1,1,6),(-1.,-0.984615384615383,-0.969230769230768,-0.953846153846152,
-0.938461538461537,-0.923076923076922,-0.907692307692306,-0.892307692307691,
-0.876923076923076,-0.86153846153846,-0.846153846153845,-0.83076923076923,
-0.815384615384614,-0.799999999999999,-0.784615384615384,-0.769230769230768,
-0.753846153846153,-0.738461538461538,-0.723076923076922,-0.707692307692307,
-0.692307692307692,-0.676923076923076,-0.661538461538461,-0.646153846153846,
-0.63076923076923,-0.615384615384615,-0.6,-0.584615384615384,-0.569230769230769,
-0.553846153846154,-0.538461538461538,-0.523076923076923,-0.507692307692308,
-0.492307692307692,-0.476923076923077,-0.461538461538462,-0.446153846153846,
-0.430769230769231,-0.415384615384615,-0.4,-0.384615384615385,-0.369230769230769,
-0.353846153846154,-0.338461538461538,-0.323076923076923,-0.307692307692308,
-0.292307692307692,-0.276923076923077,-0.261538461538462,-0.246153846153846,
-0.230769230769231,-0.215384615384615,-0.2,-0.184615384615385,-0.169230769230769,
-0.153846153846154,-0.138461538461538,-0.123076923076923,-0.107692307692308,
-0.0923076923076923,-0.0769230769230769,-0.0615384615384615,-0.0461538461538462,
-0.0307692307692308,-0.0153846153846154,-0.00577184337449602),
 .UNSPECIFIED.)
CURVE()
GEOMETRIC_REPRESENTATION_ITEM()
RATIONAL_B_SPLINE_CURVE((1.,1.,1.,1.,1.,1.,1.,1.,1.,1.,1.,1.,1.,1.,1.,1.,
1.,1.,1.,1.,1.,1.,1.,1.,1.,1.,1.,1.,1.,1.,1.,1.,1.,1.,1.,1.,1.,1.,1.,1.,
1.,1.,1.,1.,1.,1.,1.,1.,1.,1.,1.,1.,1.,1.,1.,1.,1.,1.,1.,1.,1.,1.,1.,1.,
1.,1.,1.,1.,1.,1.))
REPRESENTATION_ITEM('')
);
#316=(
BOUNDED_CURVE()
B_SPLINE_CURVE(5,(#50299,#50300,#50301,#50302,#50303,#50304,#50305,#50306,
#50307,#50308,#50309,#50310,#50311,#50312,#50313,#50314,#50315,#50316,#50317,
#50318,#50319,#50320,#50321,#50322,#50323,#50324,#50325,#50326,#50327,#50328,
#50329,#50330,#50331,#50332,#50333,#50334,#50335,#50336,#50337,#50338,#50339,
#50340,#50341,#50342,#50343,#50344,#50345,#50346,#50347,#50348,#50349,#50350,
#50351,#50352,#50353,#50354,#50355,#50356,#50357,#50358,#50359,#50360,#50361,
#50362,#50363,#50364,#50365,#50366,#50367,#50368),.UNSPECIFIED.,.F.,.F.)
B_SPLINE_CURVE_WITH_KNOTS((6,1,1,1,1,1,1,1,1,1,1,1,1,1,1,1,1,1,1,1,1,1,
1,1,1,1,1,1,1,1,1,1,1,1,1,1,1,1,1,1,1,1,1,1,1,1,1,1,1,1,1,1,1,1,1,1,1,1,
1,1,1,1,1,1,1,6),(-0.994228156739695,-0.984615384615383,-0.969230769230768,
-0.953846153846152,-0.938461538461537,-0.923076923076922,-0.907692307692306,
-0.892307692307691,-0.876923076923076,-0.86153846153846,-0.846153846153845,
-0.83076923076923,-0.815384615384614,-0.799999999999999,-0.784615384615384,
-0.769230769230768,-0.753846153846153,-0.738461538461538,-0.723076923076922,
-0.707692307692307,-0.692307692307692,-0.676923076923076,-0.661538461538461,
-0.646153846153846,-0.63076923076923,-0.615384615384615,-0.6,-0.584615384615384,
-0.569230769230769,-0.553846153846154,-0.538461538461538,-0.523076923076923,
-0.507692307692308,-0.492307692307692,-0.476923076923077,-0.461538461538462,
-0.446153846153846,-0.430769230769231,-0.415384615384615,-0.4,-0.384615384615385,
-0.369230769230769,-0.353846153846154,-0.338461538461538,-0.323076923076923,
-0.307692307692308,-0.292307692307692,-0.276923076923077,-0.261538461538462,
-0.246153846153846,-0.230769230769231,-0.215384615384615,-0.2,-0.184615384615385,
-0.169230769230769,-0.153846153846154,-0.138461538461538,-0.123076923076923,
-0.107692307692308,-0.0923076923076923,-0.0769230769230769,-0.0615384615384615,
-0.0461538461538462,-0.0307692307692308,-0.0153846153846154,0.),
 .UNSPECIFIED.)
CURVE()
GEOMETRIC_REPRESENTATION_ITEM()
RATIONAL_B_SPLINE_CURVE((1.,1.,1.,1.,1.,1.,1.,1.,1.,1.,1.,1.,1.,1.,1.,1.,
1.,1.,1.,1.,1.,1.,1.,1.,1.,1.,1.,1.,1.,1.,1.,1.,1.,1.,1.,1.,1.,1.,1.,1.,
1.,1.,1.,1.,1.,1.,1.,1.,1.,1.,1.,1.,1.,1.,1.,1.,1.,1.,1.,1.,1.,1.,1.,1.,
1.,1.,1.,1.,1.,1.))
REPRESENTATION_ITEM('')
);
#317=(
BOUNDED_CURVE()
B_SPLINE_CURVE(5,(#50521,#50522,#50523,#50524,#50525,#50526,#50527,#50528,
#50529,#50530,#50531,#50532,#50533,#50534,#50535,#50536,#50537,#50538,#50539,
#50540,#50541,#50542,#50543,#50544,#50545,#50546,#50547,#50548,#50549,#50550,
#50551,#50552,#50553,#50554,#50555,#50556,#50557,#50558,#50559,#50560,#50561,
#50562,#50563,#50564,#50565,#50566,#50567,#50568,#50569,#50570,#50571,#50572,
#50573,#50574,#50575,#50576,#50577,#50578,#50579,#50580,#50581,#50582,#50583,
#50584,#50585,#50586,#50587,#50588,#50589,#50590),.UNSPECIFIED.,.F.,.F.)
B_SPLINE_CURVE_WITH_KNOTS((6,1,1,1,1,1,1,1,1,1,1,1,1,1,1,1,1,1,1,1,1,1,
1,1,1,1,1,1,1,1,1,1,1,1,1,1,1,1,1,1,1,1,1,1,1,1,1,1,1,1,1,1,1,1,1,1,1,1,
1,1,1,1,1,1,1,6),(-1.,-0.984615384615383,-0.969230769230768,-0.953846153846152,
-0.938461538461537,-0.923076923076922,-0.907692307692306,-0.892307692307691,
-0.876923076923076,-0.86153846153846,-0.846153846153845,-0.83076923076923,
-0.815384615384614,-0.799999999999999,-0.784615384615384,-0.769230769230768,
-0.753846153846153,-0.738461538461538,-0.723076923076922,-0.707692307692307,
-0.692307692307692,-0.676923076923076,-0.661538461538461,-0.646153846153846,
-0.63076923076923,-0.615384615384615,-0.6,-0.584615384615384,-0.569230769230769,
-0.553846153846154,-0.538461538461538,-0.523076923076923,-0.507692307692308,
-0.492307692307692,-0.476923076923077,-0.461538461538462,-0.446153846153846,
-0.430769230769231,-0.415384615384615,-0.4,-0.384615384615385,-0.369230769230769,
-0.353846153846154,-0.338461538461538,-0.323076923076923,-0.307692307692308,
-0.292307692307692,-0.276923076923077,-0.261538461538462,-0.246153846153846,
-0.230769230769231,-0.215384615384615,-0.2,-0.184615384615385,-0.169230769230769,
-0.153846153846154,-0.138461538461538,-0.123076923076923,-0.107692307692308,
-0.0923076923076923,-0.0769230769230769,-0.0615384615384615,-0.0461538461538462,
-0.0307692307692308,-0.0153846153846154,-0.00577184337450911),
 .UNSPECIFIED.)
CURVE()
GEOMETRIC_REPRESENTATION_ITEM()
RATIONAL_B_SPLINE_CURVE((1.,1.,1.,1.,1.,1.,1.,1.,1.,1.,1.,1.,1.,1.,1.,1.,
1.,1.,1.,1.,1.,1.,1.,1.,1.,1.,1.,1.,1.,1.,1.,1.,1.,1.,1.,1.,1.,1.,1.,1.,
1.,1.,1.,1.,1.,1.,1.,1.,1.,1.,1.,1.,1.,1.,1.,1.,1.,1.,1.,1.,1.,1.,1.,1.,
1.,1.,1.,1.,1.,1.))
REPRESENTATION_ITEM('')
);
#318=(
BOUNDED_CURVE()
B_SPLINE_CURVE(5,(#50741,#50742,#50743,#50744,#50745,#50746,#50747,#50748,
#50749,#50750,#50751,#50752,#50753,#50754,#50755,#50756,#50757,#50758,#50759,
#50760,#50761,#50762,#50763,#50764,#50765,#50766,#50767,#50768,#50769,#50770,
#50771,#50772,#50773,#50774,#50775,#50776,#50777,#50778,#50779,#50780,#50781,
#50782,#50783,#50784,#50785,#50786,#50787,#50788,#50789,#50790,#50791,#50792,
#50793,#50794,#50795,#50796,#50797,#50798,#50799,#50800,#50801,#50802,#50803,
#50804,#50805,#50806,#50807,#50808,#50809,#50810),.UNSPECIFIED.,.F.,.F.)
B_SPLINE_CURVE_WITH_KNOTS((6,1,1,1,1,1,1,1,1,1,1,1,1,1,1,1,1,1,1,1,1,1,
1,1,1,1,1,1,1,1,1,1,1,1,1,1,1,1,1,1,1,1,1,1,1,1,1,1,1,1,1,1,1,1,1,1,1,1,
1,1,1,1,1,1,1,6),(-0.994228156739712,-0.984615384615383,-0.969230769230768,
-0.953846153846152,-0.938461538461537,-0.923076923076922,-0.907692307692306,
-0.892307692307691,-0.876923076923076,-0.86153846153846,-0.846153846153845,
-0.83076923076923,-0.815384615384614,-0.799999999999999,-0.784615384615384,
-0.769230769230768,-0.753846153846153,-0.738461538461538,-0.723076923076922,
-0.707692307692307,-0.692307692307692,-0.676923076923076,-0.661538461538461,
-0.646153846153846,-0.63076923076923,-0.615384615384615,-0.6,-0.584615384615384,
-0.569230769230769,-0.553846153846154,-0.538461538461538,-0.523076923076923,
-0.507692307692308,-0.492307692307692,-0.476923076923077,-0.461538461538462,
-0.446153846153846,-0.430769230769231,-0.415384615384615,-0.4,-0.384615384615385,
-0.369230769230769,-0.353846153846154,-0.338461538461538,-0.323076923076923,
-0.307692307692308,-0.292307692307692,-0.276923076923077,-0.261538461538462,
-0.246153846153846,-0.230769230769231,-0.215384615384615,-0.2,-0.184615384615385,
-0.169230769230769,-0.153846153846154,-0.138461538461538,-0.123076923076923,
-0.107692307692308,-0.0923076923076923,-0.0769230769230769,-0.0615384615384615,
-0.0461538461538462,-0.0307692307692308,-0.0153846153846154,0.),
 .UNSPECIFIED.)
CURVE()
GEOMETRIC_REPRESENTATION_ITEM()
RATIONAL_B_SPLINE_CURVE((1.,1.,1.,1.,1.,1.,1.,1.,1.,1.,1.,1.,1.,1.,1.,1.,
1.,1.,1.,1.,1.,1.,1.,1.,1.,1.,1.,1.,1.,1.,1.,1.,1.,1.,1.,1.,1.,1.,1.,1.,
1.,1.,1.,1.,1.,1.,1.,1.,1.,1.,1.,1.,1.,1.,1.,1.,1.,1.,1.,1.,1.,1.,1.,1.,
1.,1.,1.,1.,1.,1.))
REPRESENTATION_ITEM('')
);
#319=(
BOUNDED_CURVE()
B_SPLINE_CURVE(5,(#50963,#50964,#50965,#50966,#50967,#50968,#50969,#50970,
#50971,#50972,#50973,#50974,#50975,#50976,#50977,#50978,#50979,#50980,#50981,
#50982,#50983,#50984,#50985,#50986,#50987,#50988,#50989,#50990,#50991,#50992,
#50993,#50994,#50995,#50996,#50997,#50998,#50999,#51000,#51001,#51002,#51003,
#51004,#51005,#51006,#51007,#51008,#51009,#51010,#51011,#51012,#51013,#51014,
#51015,#51016,#51017,#51018,#51019,#51020,#51021,#51022,#51023,#51024,#51025,
#51026,#51027,#51028,#51029,#51030,#51031,#51032),.UNSPECIFIED.,.F.,.F.)
B_SPLINE_CURVE_WITH_KNOTS((6,1,1,1,1,1,1,1,1,1,1,1,1,1,1,1,1,1,1,1,1,1,
1,1,1,1,1,1,1,1,1,1,1,1,1,1,1,1,1,1,1,1,1,1,1,1,1,1,1,1,1,1,1,1,1,1,1,1,
1,1,1,1,1,1,1,6),(-1.,-0.984615384615383,-0.969230769230768,-0.953846153846152,
-0.938461538461537,-0.923076923076922,-0.907692307692306,-0.892307692307691,
-0.876923076923076,-0.86153846153846,-0.846153846153845,-0.83076923076923,
-0.815384615384614,-0.799999999999999,-0.784615384615384,-0.769230769230768,
-0.753846153846153,-0.738461538461538,-0.723076923076922,-0.707692307692307,
-0.692307692307692,-0.676923076923076,-0.661538461538461,-0.646153846153846,
-0.63076923076923,-0.615384615384615,-0.6,-0.584615384615384,-0.569230769230769,
-0.553846153846154,-0.538461538461538,-0.523076923076923,-0.507692307692308,
-0.492307692307692,-0.476923076923077,-0.461538461538462,-0.446153846153846,
-0.430769230769231,-0.415384615384615,-0.4,-0.384615384615385,-0.369230769230769,
-0.353846153846154,-0.338461538461538,-0.323076923076923,-0.307692307692308,
-0.292307692307692,-0.276923076923077,-0.261538461538462,-0.246153846153846,
-0.230769230769231,-0.215384615384615,-0.2,-0.184615384615385,-0.169230769230769,
-0.153846153846154,-0.138461538461538,-0.123076923076923,-0.107692307692308,
-0.0923076923076923,-0.0769230769230769,-0.0615384615384615,-0.0461538461538462,
-0.0307692307692308,-0.0153846153846154,-0.00577184337451206),
 .UNSPECIFIED.)
CURVE()
GEOMETRIC_REPRESENTATION_ITEM()
RATIONAL_B_SPLINE_CURVE((1.,1.,1.,1.,1.,1.,1.,1.,1.,1.,1.,1.,1.,1.,1.,1.,
1.,1.,1.,1.,1.,1.,1.,1.,1.,1.,1.,1.,1.,1.,1.,1.,1.,1.,1.,1.,1.,1.,1.,1.,
1.,1.,1.,1.,1.,1.,1.,1.,1.,1.,1.,1.,1.,1.,1.,1.,1.,1.,1.,1.,1.,1.,1.,1.,
1.,1.,1.,1.,1.,1.))
REPRESENTATION_ITEM('')
);
#320=(
BOUNDED_CURVE()
B_SPLINE_CURVE(5,(#51183,#51184,#51185,#51186,#51187,#51188,#51189,#51190,
#51191,#51192,#51193,#51194,#51195,#51196,#51197,#51198,#51199,#51200,#51201,
#51202,#51203,#51204,#51205,#51206,#51207,#51208,#51209,#51210,#51211,#51212,
#51213,#51214,#51215,#51216,#51217,#51218,#51219,#51220,#51221,#51222,#51223,
#51224,#51225,#51226,#51227,#51228,#51229,#51230,#51231,#51232,#51233,#51234,
#51235,#51236,#51237,#51238,#51239,#51240,#51241,#51242,#51243,#51244,#51245,
#51246,#51247,#51248,#51249,#51250,#51251,#51252),.UNSPECIFIED.,.F.,.F.)
B_SPLINE_CURVE_WITH_KNOTS((6,1,1,1,1,1,1,1,1,1,1,1,1,1,1,1,1,1,1,1,1,1,
1,1,1,1,1,1,1,1,1,1,1,1,1,1,1,1,1,1,1,1,1,1,1,1,1,1,1,1,1,1,1,1,1,1,1,1,
1,1,1,1,1,1,1,6),(-0.994228156739717,-0.984615384615383,-0.969230769230768,
-0.953846153846152,-0.938461538461537,-0.923076923076922,-0.907692307692306,
-0.892307692307691,-0.876923076923076,-0.86153846153846,-0.846153846153845,
-0.83076923076923,-0.815384615384614,-0.799999999999999,-0.784615384615384,
-0.769230769230768,-0.753846153846153,-0.738461538461538,-0.723076923076922,
-0.707692307692307,-0.692307692307692,-0.676923076923076,-0.661538461538461,
-0.646153846153846,-0.63076923076923,-0.615384615384615,-0.6,-0.584615384615384,
-0.569230769230769,-0.553846153846154,-0.538461538461538,-0.523076923076923,
-0.507692307692308,-0.492307692307692,-0.476923076923077,-0.461538461538462,
-0.446153846153846,-0.430769230769231,-0.415384615384615,-0.4,-0.384615384615385,
-0.369230769230769,-0.353846153846154,-0.338461538461538,-0.323076923076923,
-0.307692307692308,-0.292307692307692,-0.276923076923077,-0.261538461538462,
-0.246153846153846,-0.230769230769231,-0.215384615384615,-0.2,-0.184615384615385,
-0.169230769230769,-0.153846153846154,-0.138461538461538,-0.123076923076923,
-0.107692307692308,-0.0923076923076923,-0.0769230769230769,-0.0615384615384615,
-0.0461538461538462,-0.0307692307692308,-0.0153846153846154,0.),
 .UNSPECIFIED.)
CURVE()
GEOMETRIC_REPRESENTATION_ITEM()
RATIONAL_B_SPLINE_CURVE((1.,1.,1.,1.,1.,1.,1.,1.,1.,1.,1.,1.,1.,1.,1.,1.,
1.,1.,1.,1.,1.,1.,1.,1.,1.,1.,1.,1.,1.,1.,1.,1.,1.,1.,1.,1.,1.,1.,1.,1.,
1.,1.,1.,1.,1.,1.,1.,1.,1.,1.,1.,1.,1.,1.,1.,1.,1.,1.,1.,1.,1.,1.,1.,1.,
1.,1.,1.,1.,1.,1.))
REPRESENTATION_ITEM('')
);
#321=(
BOUNDED_CURVE()
B_SPLINE_CURVE(5,(#51405,#51406,#51407,#51408,#51409,#51410,#51411,#51412,
#51413,#51414,#51415,#51416,#51417,#51418,#51419,#51420,#51421,#51422,#51423,
#51424,#51425,#51426,#51427,#51428,#51429,#51430,#51431,#51432,#51433,#51434,
#51435,#51436,#51437,#51438,#51439,#51440,#51441,#51442,#51443,#51444,#51445,
#51446,#51447,#51448,#51449,#51450,#51451,#51452,#51453,#51454,#51455,#51456,
#51457,#51458,#51459,#51460,#51461,#51462,#51463,#51464,#51465,#51466,#51467,
#51468,#51469,#51470,#51471,#51472,#51473,#51474),.UNSPECIFIED.,.F.,.F.)
B_SPLINE_CURVE_WITH_KNOTS((6,1,1,1,1,1,1,1,1,1,1,1,1,1,1,1,1,1,1,1,1,1,
1,1,1,1,1,1,1,1,1,1,1,1,1,1,1,1,1,1,1,1,1,1,1,1,1,1,1,1,1,1,1,1,1,1,1,1,
1,1,1,1,1,1,1,6),(-1.,-0.984615384615383,-0.969230769230768,-0.953846153846152,
-0.938461538461537,-0.923076923076922,-0.907692307692306,-0.892307692307691,
-0.876923076923076,-0.86153846153846,-0.846153846153845,-0.83076923076923,
-0.815384615384614,-0.799999999999999,-0.784615384615384,-0.769230769230768,
-0.753846153846153,-0.738461538461538,-0.723076923076922,-0.707692307692307,
-0.692307692307692,-0.676923076923076,-0.661538461538461,-0.646153846153846,
-0.63076923076923,-0.615384615384615,-0.6,-0.584615384615384,-0.569230769230769,
-0.553846153846154,-0.538461538461538,-0.523076923076923,-0.507692307692308,
-0.492307692307692,-0.476923076923077,-0.461538461538462,-0.446153846153846,
-0.430769230769231,-0.415384615384615,-0.4,-0.384615384615385,-0.369230769230769,
-0.353846153846154,-0.338461538461538,-0.323076923076923,-0.307692307692308,
-0.292307692307692,-0.276923076923077,-0.261538461538462,-0.246153846153846,
-0.230769230769231,-0.215384615384615,-0.2,-0.184615384615385,-0.169230769230769,
-0.153846153846154,-0.138461538461538,-0.123076923076923,-0.107692307692308,
-0.0923076923076923,-0.0769230769230769,-0.0615384615384615,-0.0461538461538462,
-0.0307692307692308,-0.0153846153846154,-0.00577184337448646),
 .UNSPECIFIED.)
CURVE()
GEOMETRIC_REPRESENTATION_ITEM()
RATIONAL_B_SPLINE_CURVE((1.,1.,1.,1.,1.,1.,1.,1.,1.,1.,1.,1.,1.,1.,1.,1.,
1.,1.,1.,1.,1.,1.,1.,1.,1.,1.,1.,1.,1.,1.,1.,1.,1.,1.,1.,1.,1.,1.,1.,1.,
1.,1.,1.,1.,1.,1.,1.,1.,1.,1.,1.,1.,1.,1.,1.,1.,1.,1.,1.,1.,1.,1.,1.,1.,
1.,1.,1.,1.,1.,1.))
REPRESENTATION_ITEM('')
);
#322=(
BOUNDED_CURVE()
B_SPLINE_CURVE(5,(#51625,#51626,#51627,#51628,#51629,#51630,#51631,#51632,
#51633,#51634,#51635,#51636,#51637,#51638,#51639,#51640,#51641,#51642,#51643,
#51644,#51645,#51646,#51647,#51648,#51649,#51650,#51651,#51652,#51653,#51654,
#51655,#51656,#51657,#51658,#51659,#51660,#51661,#51662,#51663,#51664,#51665,
#51666,#51667,#51668,#51669,#51670,#51671,#51672,#51673,#51674,#51675,#51676,
#51677,#51678,#51679,#51680,#51681,#51682,#51683,#51684,#51685,#51686,#51687,
#51688,#51689,#51690,#51691,#51692,#51693,#51694),.UNSPECIFIED.,.F.,.F.)
B_SPLINE_CURVE_WITH_KNOTS((6,1,1,1,1,1,1,1,1,1,1,1,1,1,1,1,1,1,1,1,1,1,
1,1,1,1,1,1,1,1,1,1,1,1,1,1,1,1,1,1,1,1,1,1,1,1,1,1,1,1,1,1,1,1,1,1,1,1,
1,1,1,1,1,1,1,6),(-0.994228156739708,-0.984615384615383,-0.969230769230768,
-0.953846153846152,-0.938461538461537,-0.923076923076922,-0.907692307692306,
-0.892307692307691,-0.876923076923076,-0.86153846153846,-0.846153846153845,
-0.83076923076923,-0.815384615384614,-0.799999999999999,-0.784615384615384,
-0.769230769230768,-0.753846153846153,-0.738461538461538,-0.723076923076922,
-0.707692307692307,-0.692307692307692,-0.676923076923076,-0.661538461538461,
-0.646153846153846,-0.63076923076923,-0.615384615384615,-0.6,-0.584615384615384,
-0.569230769230769,-0.553846153846154,-0.538461538461538,-0.523076923076923,
-0.507692307692308,-0.492307692307692,-0.476923076923077,-0.461538461538462,
-0.446153846153846,-0.430769230769231,-0.415384615384615,-0.4,-0.384615384615385,
-0.369230769230769,-0.353846153846154,-0.338461538461538,-0.323076923076923,
-0.307692307692308,-0.292307692307692,-0.276923076923077,-0.261538461538462,
-0.246153846153846,-0.230769230769231,-0.215384615384615,-0.2,-0.184615384615385,
-0.169230769230769,-0.153846153846154,-0.138461538461538,-0.123076923076923,
-0.107692307692308,-0.0923076923076923,-0.0769230769230769,-0.0615384615384615,
-0.0461538461538462,-0.0307692307692308,-0.0153846153846154,0.),
 .UNSPECIFIED.)
CURVE()
GEOMETRIC_REPRESENTATION_ITEM()
RATIONAL_B_SPLINE_CURVE((1.,1.,1.,1.,1.,1.,1.,1.,1.,1.,1.,1.,1.,1.,1.,1.,
1.,1.,1.,1.,1.,1.,1.,1.,1.,1.,1.,1.,1.,1.,1.,1.,1.,1.,1.,1.,1.,1.,1.,1.,
1.,1.,1.,1.,1.,1.,1.,1.,1.,1.,1.,1.,1.,1.,1.,1.,1.,1.,1.,1.,1.,1.,1.,1.,
1.,1.,1.,1.,1.,1.))
REPRESENTATION_ITEM('')
);
#323=(
BOUNDED_CURVE()
B_SPLINE_CURVE(5,(#51847,#51848,#51849,#51850,#51851,#51852,#51853,#51854,
#51855,#51856,#51857,#51858,#51859,#51860,#51861,#51862,#51863,#51864,#51865,
#51866,#51867,#51868,#51869,#51870,#51871,#51872,#51873,#51874,#51875,#51876,
#51877,#51878,#51879,#51880,#51881,#51882,#51883,#51884,#51885,#51886,#51887,
#51888,#51889,#51890,#51891,#51892,#51893,#51894,#51895,#51896,#51897,#51898,
#51899,#51900,#51901,#51902,#51903,#51904,#51905,#51906,#51907,#51908,#51909,
#51910,#51911,#51912,#51913,#51914,#51915,#51916),.UNSPECIFIED.,.F.,.F.)
B_SPLINE_CURVE_WITH_KNOTS((6,1,1,1,1,1,1,1,1,1,1,1,1,1,1,1,1,1,1,1,1,1,
1,1,1,1,1,1,1,1,1,1,1,1,1,1,1,1,1,1,1,1,1,1,1,1,1,1,1,1,1,1,1,1,1,1,1,1,
1,1,1,1,1,1,1,6),(-1.,-0.984615384615383,-0.969230769230768,-0.953846153846152,
-0.938461538461537,-0.923076923076922,-0.907692307692306,-0.892307692307691,
-0.876923076923076,-0.86153846153846,-0.846153846153845,-0.83076923076923,
-0.815384615384614,-0.799999999999999,-0.784615384615384,-0.769230769230768,
-0.753846153846153,-0.738461538461538,-0.723076923076922,-0.707692307692307,
-0.692307692307692,-0.676923076923076,-0.661538461538461,-0.646153846153846,
-0.63076923076923,-0.615384615384615,-0.6,-0.584615384615384,-0.569230769230769,
-0.553846153846154,-0.538461538461538,-0.523076923076923,-0.507692307692308,
-0.492307692307692,-0.476923076923077,-0.461538461538462,-0.446153846153846,
-0.430769230769231,-0.415384615384615,-0.4,-0.384615384615385,-0.369230769230769,
-0.353846153846154,-0.338461538461538,-0.323076923076923,-0.307692307692308,
-0.292307692307692,-0.276923076923077,-0.261538461538462,-0.246153846153846,
-0.230769230769231,-0.215384615384615,-0.2,-0.184615384615385,-0.169230769230769,
-0.153846153846154,-0.138461538461538,-0.123076923076923,-0.107692307692308,
-0.0923076923076923,-0.0769230769230769,-0.0615384615384615,-0.0461538461538462,
-0.0307692307692308,-0.0153846153846154,-0.00577184337451626),
 .UNSPECIFIED.)
CURVE()
GEOMETRIC_REPRESENTATION_ITEM()
RATIONAL_B_SPLINE_CURVE((1.,1.,1.,1.,1.,1.,1.,1.,1.,1.,1.,1.,1.,1.,1.,1.,
1.,1.,1.,1.,1.,1.,1.,1.,1.,1.,1.,1.,1.,1.,1.,1.,1.,1.,1.,1.,1.,1.,1.,1.,
1.,1.,1.,1.,1.,1.,1.,1.,1.,1.,1.,1.,1.,1.,1.,1.,1.,1.,1.,1.,1.,1.,1.,1.,
1.,1.,1.,1.,1.,1.))
REPRESENTATION_ITEM('')
);
#324=(
BOUNDED_CURVE()
B_SPLINE_CURVE(5,(#52067,#52068,#52069,#52070,#52071,#52072,#52073,#52074,
#52075,#52076,#52077,#52078,#52079,#52080,#52081,#52082,#52083,#52084,#52085,
#52086,#52087,#52088,#52089,#52090,#52091,#52092,#52093,#52094,#52095,#52096,
#52097,#52098,#52099,#52100,#52101,#52102,#52103,#52104,#52105,#52106,#52107,
#52108,#52109,#52110,#52111,#52112,#52113,#52114,#52115,#52116,#52117,#52118,
#52119,#52120,#52121,#52122,#52123,#52124,#52125,#52126,#52127,#52128,#52129,
#52130,#52131,#52132,#52133,#52134,#52135,#52136),.UNSPECIFIED.,.F.,.F.)
B_SPLINE_CURVE_WITH_KNOTS((6,1,1,1,1,1,1,1,1,1,1,1,1,1,1,1,1,1,1,1,1,1,
1,1,1,1,1,1,1,1,1,1,1,1,1,1,1,1,1,1,1,1,1,1,1,1,1,1,1,1,1,1,1,1,1,1,1,1,
1,1,1,1,1,1,1,6),(-0.994228156739708,-0.984615384615383,-0.969230769230768,
-0.953846153846152,-0.938461538461537,-0.923076923076922,-0.907692307692306,
-0.892307692307691,-0.876923076923076,-0.86153846153846,-0.846153846153845,
-0.83076923076923,-0.815384615384614,-0.799999999999999,-0.784615384615384,
-0.769230769230768,-0.753846153846153,-0.738461538461538,-0.723076923076922,
-0.707692307692307,-0.692307692307692,-0.676923076923076,-0.661538461538461,
-0.646153846153846,-0.63076923076923,-0.615384615384615,-0.6,-0.584615384615384,
-0.569230769230769,-0.553846153846154,-0.538461538461538,-0.523076923076923,
-0.507692307692308,-0.492307692307692,-0.476923076923077,-0.461538461538462,
-0.446153846153846,-0.430769230769231,-0.415384615384615,-0.4,-0.384615384615385,
-0.369230769230769,-0.353846153846154,-0.338461538461538,-0.323076923076923,
-0.307692307692308,-0.292307692307692,-0.276923076923077,-0.261538461538462,
-0.246153846153846,-0.230769230769231,-0.215384615384615,-0.2,-0.184615384615385,
-0.169230769230769,-0.153846153846154,-0.138461538461538,-0.123076923076923,
-0.107692307692308,-0.0923076923076923,-0.0769230769230769,-0.0615384615384615,
-0.0461538461538462,-0.0307692307692308,-0.0153846153846154,0.),
 .UNSPECIFIED.)
CURVE()
GEOMETRIC_REPRESENTATION_ITEM()
RATIONAL_B_SPLINE_CURVE((1.,1.,1.,1.,1.,1.,1.,1.,1.,1.,1.,1.,1.,1.,1.,1.,
1.,1.,1.,1.,1.,1.,1.,1.,1.,1.,1.,1.,1.,1.,1.,1.,1.,1.,1.,1.,1.,1.,1.,1.,
1.,1.,1.,1.,1.,1.,1.,1.,1.,1.,1.,1.,1.,1.,1.,1.,1.,1.,1.,1.,1.,1.,1.,1.,
1.,1.,1.,1.,1.,1.))
REPRESENTATION_ITEM('')
);
#325=(
BOUNDED_CURVE()
B_SPLINE_CURVE(5,(#52289,#52290,#52291,#52292,#52293,#52294,#52295,#52296,
#52297,#52298,#52299,#52300,#52301,#52302,#52303,#52304,#52305,#52306,#52307,
#52308,#52309,#52310,#52311,#52312,#52313,#52314,#52315,#52316,#52317,#52318,
#52319,#52320,#52321,#52322,#52323,#52324,#52325,#52326,#52327,#52328,#52329,
#52330,#52331,#52332,#52333,#52334,#52335,#52336,#52337,#52338,#52339,#52340,
#52341,#52342,#52343,#52344,#52345,#52346,#52347,#52348,#52349,#52350,#52351,
#52352,#52353,#52354,#52355,#52356,#52357,#52358),.UNSPECIFIED.,.F.,.F.)
B_SPLINE_CURVE_WITH_KNOTS((6,1,1,1,1,1,1,1,1,1,1,1,1,1,1,1,1,1,1,1,1,1,
1,1,1,1,1,1,1,1,1,1,1,1,1,1,1,1,1,1,1,1,1,1,1,1,1,1,1,1,1,1,1,1,1,1,1,1,
1,1,1,1,1,1,1,6),(-1.,-0.984615384615383,-0.969230769230768,-0.953846153846152,
-0.938461538461537,-0.923076923076922,-0.907692307692306,-0.892307692307691,
-0.876923076923076,-0.86153846153846,-0.846153846153845,-0.83076923076923,
-0.815384615384614,-0.799999999999999,-0.784615384615384,-0.769230769230768,
-0.753846153846153,-0.738461538461538,-0.723076923076922,-0.707692307692307,
-0.692307692307692,-0.676923076923076,-0.661538461538461,-0.646153846153846,
-0.63076923076923,-0.615384615384615,-0.6,-0.584615384615384,-0.569230769230769,
-0.553846153846154,-0.538461538461538,-0.523076923076923,-0.507692307692308,
-0.492307692307692,-0.476923076923077,-0.461538461538462,-0.446153846153846,
-0.430769230769231,-0.415384615384615,-0.4,-0.384615384615385,-0.369230769230769,
-0.353846153846154,-0.338461538461538,-0.323076923076923,-0.307692307692308,
-0.292307692307692,-0.276923076923077,-0.261538461538462,-0.246153846153846,
-0.230769230769231,-0.215384615384615,-0.2,-0.184615384615385,-0.169230769230769,
-0.153846153846154,-0.138461538461538,-0.123076923076923,-0.107692307692308,
-0.0923076923076923,-0.0769230769230769,-0.0615384615384615,-0.0461538461538462,
-0.0307692307692308,-0.0153846153846154,-0.00577184337451372),
 .UNSPECIFIED.)
CURVE()
GEOMETRIC_REPRESENTATION_ITEM()
RATIONAL_B_SPLINE_CURVE((1.,1.,1.,1.,1.,1.,1.,1.,1.,1.,1.,1.,1.,1.,1.,1.,
1.,1.,1.,1.,1.,1.,1.,1.,1.,1.,1.,1.,1.,1.,1.,1.,1.,1.,1.,1.,1.,1.,1.,1.,
1.,1.,1.,1.,1.,1.,1.,1.,1.,1.,1.,1.,1.,1.,1.,1.,1.,1.,1.,1.,1.,1.,1.,1.,
1.,1.,1.,1.,1.,1.))
REPRESENTATION_ITEM('')
);
#326=(
BOUNDED_CURVE()
B_SPLINE_CURVE(5,(#52509,#52510,#52511,#52512,#52513,#52514,#52515,#52516,
#52517,#52518,#52519,#52520,#52521,#52522,#52523,#52524,#52525,#52526,#52527,
#52528,#52529,#52530,#52531,#52532,#52533,#52534,#52535,#52536,#52537,#52538,
#52539,#52540,#52541,#52542,#52543,#52544,#52545,#52546,#52547,#52548,#52549,
#52550,#52551,#52552,#52553,#52554,#52555,#52556,#52557,#52558,#52559,#52560,
#52561,#52562,#52563,#52564,#52565,#52566,#52567,#52568,#52569,#52570,#52571,
#52572,#52573,#52574,#52575,#52576,#52577,#52578),.UNSPECIFIED.,.F.,.F.)
B_SPLINE_CURVE_WITH_KNOTS((6,1,1,1,1,1,1,1,1,1,1,1,1,1,1,1,1,1,1,1,1,1,
1,1,1,1,1,1,1,1,1,1,1,1,1,1,1,1,1,1,1,1,1,1,1,1,1,1,1,1,1,1,1,1,1,1,1,1,
1,1,1,1,1,1,1,6),(-0.994228156739703,-0.984615384615383,-0.969230769230768,
-0.953846153846152,-0.938461538461537,-0.923076923076922,-0.907692307692306,
-0.892307692307691,-0.876923076923076,-0.86153846153846,-0.846153846153845,
-0.83076923076923,-0.815384615384614,-0.799999999999999,-0.784615384615384,
-0.769230769230768,-0.753846153846153,-0.738461538461538,-0.723076923076922,
-0.707692307692307,-0.692307692307692,-0.676923076923076,-0.661538461538461,
-0.646153846153846,-0.63076923076923,-0.615384615384615,-0.6,-0.584615384615384,
-0.569230769230769,-0.553846153846154,-0.538461538461538,-0.523076923076923,
-0.507692307692308,-0.492307692307692,-0.476923076923077,-0.461538461538462,
-0.446153846153846,-0.430769230769231,-0.415384615384615,-0.4,-0.384615384615385,
-0.369230769230769,-0.353846153846154,-0.338461538461538,-0.323076923076923,
-0.307692307692308,-0.292307692307692,-0.276923076923077,-0.261538461538462,
-0.246153846153846,-0.230769230769231,-0.215384615384615,-0.2,-0.184615384615385,
-0.169230769230769,-0.153846153846154,-0.138461538461538,-0.123076923076923,
-0.107692307692308,-0.0923076923076923,-0.0769230769230769,-0.0615384615384615,
-0.0461538461538462,-0.0307692307692308,-0.0153846153846154,0.),
 .UNSPECIFIED.)
CURVE()
GEOMETRIC_REPRESENTATION_ITEM()
RATIONAL_B_SPLINE_CURVE((1.,1.,1.,1.,1.,1.,1.,1.,1.,1.,1.,1.,1.,1.,1.,1.,
1.,1.,1.,1.,1.,1.,1.,1.,1.,1.,1.,1.,1.,1.,1.,1.,1.,1.,1.,1.,1.,1.,1.,1.,
1.,1.,1.,1.,1.,1.,1.,1.,1.,1.,1.,1.,1.,1.,1.,1.,1.,1.,1.,1.,1.,1.,1.,1.,
1.,1.,1.,1.,1.,1.))
REPRESENTATION_ITEM('')
);
#327=(
BOUNDED_CURVE()
B_SPLINE_CURVE(5,(#52731,#52732,#52733,#52734,#52735,#52736,#52737,#52738,
#52739,#52740,#52741,#52742,#52743,#52744,#52745,#52746,#52747,#52748,#52749,
#52750,#52751,#52752,#52753,#52754,#52755,#52756,#52757,#52758,#52759,#52760,
#52761,#52762,#52763,#52764,#52765,#52766,#52767,#52768,#52769,#52770,#52771,
#52772,#52773,#52774,#52775,#52776,#52777,#52778,#52779,#52780,#52781,#52782,
#52783,#52784,#52785,#52786,#52787,#52788,#52789,#52790,#52791,#52792,#52793,
#52794,#52795,#52796,#52797,#52798,#52799,#52800),.UNSPECIFIED.,.F.,.F.)
B_SPLINE_CURVE_WITH_KNOTS((6,1,1,1,1,1,1,1,1,1,1,1,1,1,1,1,1,1,1,1,1,1,
1,1,1,1,1,1,1,1,1,1,1,1,1,1,1,1,1,1,1,1,1,1,1,1,1,1,1,1,1,1,1,1,1,1,1,1,
1,1,1,1,1,1,1,6),(-1.,-0.984615384615383,-0.969230769230768,-0.953846153846152,
-0.938461538461537,-0.923076923076922,-0.907692307692306,-0.892307692307691,
-0.876923076923076,-0.86153846153846,-0.846153846153845,-0.83076923076923,
-0.815384615384614,-0.799999999999999,-0.784615384615384,-0.769230769230768,
-0.753846153846153,-0.738461538461538,-0.723076923076922,-0.707692307692307,
-0.692307692307692,-0.676923076923076,-0.661538461538461,-0.646153846153846,
-0.63076923076923,-0.615384615384615,-0.6,-0.584615384615384,-0.569230769230769,
-0.553846153846154,-0.538461538461538,-0.523076923076923,-0.507692307692308,
-0.492307692307692,-0.476923076923077,-0.461538461538462,-0.446153846153846,
-0.430769230769231,-0.415384615384615,-0.4,-0.384615384615385,-0.369230769230769,
-0.353846153846154,-0.338461538461538,-0.323076923076923,-0.307692307692308,
-0.292307692307692,-0.276923076923077,-0.261538461538462,-0.246153846153846,
-0.230769230769231,-0.215384615384615,-0.2,-0.184615384615385,-0.169230769230769,
-0.153846153846154,-0.138461538461538,-0.123076923076923,-0.107692307692308,
-0.0923076923076923,-0.0769230769230769,-0.0615384615384615,-0.0461538461538462,
-0.0307692307692308,-0.0153846153846154,-0.00577184337451698),
 .UNSPECIFIED.)
CURVE()
GEOMETRIC_REPRESENTATION_ITEM()
RATIONAL_B_SPLINE_CURVE((1.,1.,1.,1.,1.,1.,1.,1.,1.,1.,1.,1.,1.,1.,1.,1.,
1.,1.,1.,1.,1.,1.,1.,1.,1.,1.,1.,1.,1.,1.,1.,1.,1.,1.,1.,1.,1.,1.,1.,1.,
1.,1.,1.,1.,1.,1.,1.,1.,1.,1.,1.,1.,1.,1.,1.,1.,1.,1.,1.,1.,1.,1.,1.,1.,
1.,1.,1.,1.,1.,1.))
REPRESENTATION_ITEM('')
);
#328=(
BOUNDED_CURVE()
B_SPLINE_CURVE(5,(#52951,#52952,#52953,#52954,#52955,#52956,#52957,#52958,
#52959,#52960,#52961,#52962,#52963,#52964,#52965,#52966,#52967,#52968,#52969,
#52970,#52971,#52972,#52973,#52974,#52975,#52976,#52977,#52978,#52979,#52980,
#52981,#52982,#52983,#52984,#52985,#52986,#52987,#52988,#52989,#52990,#52991,
#52992,#52993,#52994,#52995,#52996,#52997,#52998,#52999,#53000,#53001,#53002,
#53003,#53004,#53005,#53006,#53007,#53008,#53009,#53010,#53011,#53012,#53013,
#53014,#53015,#53016,#53017,#53018,#53019,#53020),.UNSPECIFIED.,.F.,.F.)
B_SPLINE_CURVE_WITH_KNOTS((6,1,1,1,1,1,1,1,1,1,1,1,1,1,1,1,1,1,1,1,1,1,
1,1,1,1,1,1,1,1,1,1,1,1,1,1,1,1,1,1,1,1,1,1,1,1,1,1,1,1,1,1,1,1,1,1,1,1,
1,1,1,1,1,1,1,6),(-0.994228156739706,-0.984615384615383,-0.969230769230768,
-0.953846153846152,-0.938461538461537,-0.923076923076922,-0.907692307692306,
-0.892307692307691,-0.876923076923076,-0.86153846153846,-0.846153846153845,
-0.83076923076923,-0.815384615384614,-0.799999999999999,-0.784615384615384,
-0.769230769230768,-0.753846153846153,-0.738461538461538,-0.723076923076922,
-0.707692307692307,-0.692307692307692,-0.676923076923076,-0.661538461538461,
-0.646153846153846,-0.63076923076923,-0.615384615384615,-0.6,-0.584615384615384,
-0.569230769230769,-0.553846153846154,-0.538461538461538,-0.523076923076923,
-0.507692307692308,-0.492307692307692,-0.476923076923077,-0.461538461538462,
-0.446153846153846,-0.430769230769231,-0.415384615384615,-0.4,-0.384615384615385,
-0.369230769230769,-0.353846153846154,-0.338461538461538,-0.323076923076923,
-0.307692307692308,-0.292307692307692,-0.276923076923077,-0.261538461538462,
-0.246153846153846,-0.230769230769231,-0.215384615384615,-0.2,-0.184615384615385,
-0.169230769230769,-0.153846153846154,-0.138461538461538,-0.123076923076923,
-0.107692307692308,-0.0923076923076923,-0.0769230769230769,-0.0615384615384615,
-0.0461538461538462,-0.0307692307692308,-0.0153846153846154,0.),
 .UNSPECIFIED.)
CURVE()
GEOMETRIC_REPRESENTATION_ITEM()
RATIONAL_B_SPLINE_CURVE((1.,1.,1.,1.,1.,1.,1.,1.,1.,1.,1.,1.,1.,1.,1.,1.,
1.,1.,1.,1.,1.,1.,1.,1.,1.,1.,1.,1.,1.,1.,1.,1.,1.,1.,1.,1.,1.,1.,1.,1.,
1.,1.,1.,1.,1.,1.,1.,1.,1.,1.,1.,1.,1.,1.,1.,1.,1.,1.,1.,1.,1.,1.,1.,1.,
1.,1.,1.,1.,1.,1.))
REPRESENTATION_ITEM('')
);
#329=(
BOUNDED_CURVE()
B_SPLINE_CURVE(5,(#53173,#53174,#53175,#53176,#53177,#53178,#53179,#53180,
#53181,#53182,#53183,#53184,#53185,#53186,#53187,#53188,#53189,#53190,#53191,
#53192,#53193,#53194,#53195,#53196,#53197,#53198,#53199,#53200,#53201,#53202,
#53203,#53204,#53205,#53206,#53207,#53208,#53209,#53210,#53211,#53212,#53213,
#53214,#53215,#53216,#53217,#53218,#53219,#53220,#53221,#53222,#53223,#53224,
#53225,#53226,#53227,#53228,#53229,#53230,#53231,#53232,#53233,#53234,#53235,
#53236,#53237,#53238,#53239,#53240,#53241,#53242),.UNSPECIFIED.,.F.,.F.)
B_SPLINE_CURVE_WITH_KNOTS((6,1,1,1,1,1,1,1,1,1,1,1,1,1,1,1,1,1,1,1,1,1,
1,1,1,1,1,1,1,1,1,1,1,1,1,1,1,1,1,1,1,1,1,1,1,1,1,1,1,1,1,1,1,1,1,1,1,1,
1,1,1,1,1,1,1,6),(-1.,-0.984615384615383,-0.969230769230768,-0.953846153846152,
-0.938461538461537,-0.923076923076922,-0.907692307692306,-0.892307692307691,
-0.876923076923076,-0.86153846153846,-0.846153846153845,-0.83076923076923,
-0.815384615384614,-0.799999999999999,-0.784615384615384,-0.769230769230768,
-0.753846153846153,-0.738461538461538,-0.723076923076922,-0.707692307692307,
-0.692307692307692,-0.676923076923076,-0.661538461538461,-0.646153846153846,
-0.63076923076923,-0.615384615384615,-0.6,-0.584615384615384,-0.569230769230769,
-0.553846153846154,-0.538461538461538,-0.523076923076923,-0.507692307692308,
-0.492307692307692,-0.476923076923077,-0.461538461538462,-0.446153846153846,
-0.430769230769231,-0.415384615384615,-0.4,-0.384615384615385,-0.369230769230769,
-0.353846153846154,-0.338461538461538,-0.323076923076923,-0.307692307692308,
-0.292307692307692,-0.276923076923077,-0.261538461538462,-0.246153846153846,
-0.230769230769231,-0.215384615384615,-0.2,-0.184615384615385,-0.169230769230769,
-0.153846153846154,-0.138461538461538,-0.123076923076923,-0.107692307692308,
-0.0923076923076923,-0.0769230769230769,-0.0615384615384615,-0.0461538461538462,
-0.0307692307692308,-0.0153846153846154,-0.00577184337452512),
 .UNSPECIFIED.)
CURVE()
GEOMETRIC_REPRESENTATION_ITEM()
RATIONAL_B_SPLINE_CURVE((1.,1.,1.,1.,1.,1.,1.,1.,1.,1.,1.,1.,1.,1.,1.,1.,
1.,1.,1.,1.,1.,1.,1.,1.,1.,1.,1.,1.,1.,1.,1.,1.,1.,1.,1.,1.,1.,1.,1.,1.,
1.,1.,1.,1.,1.,1.,1.,1.,1.,1.,1.,1.,1.,1.,1.,1.,1.,1.,1.,1.,1.,1.,1.,1.,
1.,1.,1.,1.,1.,1.))
REPRESENTATION_ITEM('')
);
#330=(
BOUNDED_CURVE()
B_SPLINE_CURVE(5,(#53393,#53394,#53395,#53396,#53397,#53398,#53399,#53400,
#53401,#53402,#53403,#53404,#53405,#53406,#53407,#53408,#53409,#53410,#53411,
#53412,#53413,#53414,#53415,#53416,#53417,#53418,#53419,#53420,#53421,#53422,
#53423,#53424,#53425,#53426,#53427,#53428,#53429,#53430,#53431,#53432,#53433,
#53434,#53435,#53436,#53437,#53438,#53439,#53440,#53441,#53442,#53443,#53444,
#53445,#53446,#53447,#53448,#53449,#53450,#53451,#53452,#53453,#53454,#53455,
#53456,#53457,#53458,#53459,#53460,#53461,#53462),.UNSPECIFIED.,.F.,.F.)
B_SPLINE_CURVE_WITH_KNOTS((6,1,1,1,1,1,1,1,1,1,1,1,1,1,1,1,1,1,1,1,1,1,
1,1,1,1,1,1,1,1,1,1,1,1,1,1,1,1,1,1,1,1,1,1,1,1,1,1,1,1,1,1,1,1,1,1,1,1,
1,1,1,1,1,1,1,6),(-0.994228156739713,-0.984615384615383,-0.969230769230768,
-0.953846153846152,-0.938461538461537,-0.923076923076922,-0.907692307692306,
-0.892307692307691,-0.876923076923076,-0.86153846153846,-0.846153846153845,
-0.83076923076923,-0.815384615384614,-0.799999999999999,-0.784615384615384,
-0.769230769230768,-0.753846153846153,-0.738461538461538,-0.723076923076922,
-0.707692307692307,-0.692307692307692,-0.676923076923076,-0.661538461538461,
-0.646153846153846,-0.63076923076923,-0.615384615384615,-0.6,-0.584615384615384,
-0.569230769230769,-0.553846153846154,-0.538461538461538,-0.523076923076923,
-0.507692307692308,-0.492307692307692,-0.476923076923077,-0.461538461538462,
-0.446153846153846,-0.430769230769231,-0.415384615384615,-0.4,-0.384615384615385,
-0.369230769230769,-0.353846153846154,-0.338461538461538,-0.323076923076923,
-0.307692307692308,-0.292307692307692,-0.276923076923077,-0.261538461538462,
-0.246153846153846,-0.230769230769231,-0.215384615384615,-0.2,-0.184615384615385,
-0.169230769230769,-0.153846153846154,-0.138461538461538,-0.123076923076923,
-0.107692307692308,-0.0923076923076923,-0.0769230769230769,-0.0615384615384615,
-0.0461538461538462,-0.0307692307692308,-0.0153846153846154,0.),
 .UNSPECIFIED.)
CURVE()
GEOMETRIC_REPRESENTATION_ITEM()
RATIONAL_B_SPLINE_CURVE((1.,1.,1.,1.,1.,1.,1.,1.,1.,1.,1.,1.,1.,1.,1.,1.,
1.,1.,1.,1.,1.,1.,1.,1.,1.,1.,1.,1.,1.,1.,1.,1.,1.,1.,1.,1.,1.,1.,1.,1.,
1.,1.,1.,1.,1.,1.,1.,1.,1.,1.,1.,1.,1.,1.,1.,1.,1.,1.,1.,1.,1.,1.,1.,1.,
1.,1.,1.,1.,1.,1.))
REPRESENTATION_ITEM('')
);
#331=(
BOUNDED_CURVE()
B_SPLINE_CURVE(5,(#53615,#53616,#53617,#53618,#53619,#53620,#53621,#53622,
#53623,#53624,#53625,#53626,#53627,#53628,#53629,#53630,#53631,#53632,#53633,
#53634,#53635,#53636,#53637,#53638,#53639,#53640,#53641,#53642,#53643,#53644,
#53645,#53646,#53647,#53648,#53649,#53650,#53651,#53652,#53653,#53654,#53655,
#53656,#53657,#53658,#53659,#53660,#53661,#53662,#53663,#53664,#53665,#53666,
#53667,#53668,#53669,#53670,#53671,#53672,#53673,#53674,#53675,#53676,#53677,
#53678,#53679,#53680,#53681,#53682,#53683,#53684),.UNSPECIFIED.,.F.,.F.)
B_SPLINE_CURVE_WITH_KNOTS((6,1,1,1,1,1,1,1,1,1,1,1,1,1,1,1,1,1,1,1,1,1,
1,1,1,1,1,1,1,1,1,1,1,1,1,1,1,1,1,1,1,1,1,1,1,1,1,1,1,1,1,1,1,1,1,1,1,1,
1,1,1,1,1,1,1,6),(-1.,-0.984615384615383,-0.969230769230768,-0.953846153846152,
-0.938461538461537,-0.923076923076922,-0.907692307692306,-0.892307692307691,
-0.876923076923076,-0.86153846153846,-0.846153846153845,-0.83076923076923,
-0.815384615384614,-0.799999999999999,-0.784615384615384,-0.769230769230768,
-0.753846153846153,-0.738461538461538,-0.723076923076922,-0.707692307692307,
-0.692307692307692,-0.676923076923076,-0.661538461538461,-0.646153846153846,
-0.63076923076923,-0.615384615384615,-0.6,-0.584615384615384,-0.569230769230769,
-0.553846153846154,-0.538461538461538,-0.523076923076923,-0.507692307692308,
-0.492307692307692,-0.476923076923077,-0.461538461538462,-0.446153846153846,
-0.430769230769231,-0.415384615384615,-0.4,-0.384615384615385,-0.369230769230769,
-0.353846153846154,-0.338461538461538,-0.323076923076923,-0.307692307692308,
-0.292307692307692,-0.276923076923077,-0.261538461538462,-0.246153846153846,
-0.230769230769231,-0.215384615384615,-0.2,-0.184615384615385,-0.169230769230769,
-0.153846153846154,-0.138461538461538,-0.123076923076923,-0.107692307692308,
-0.0923076923076923,-0.0769230769230769,-0.0615384615384615,-0.0461538461538462,
-0.0307692307692308,-0.0153846153846154,-0.00577184337450204),
 .UNSPECIFIED.)
CURVE()
GEOMETRIC_REPRESENTATION_ITEM()
RATIONAL_B_SPLINE_CURVE((1.,1.,1.,1.,1.,1.,1.,1.,1.,1.,1.,1.,1.,1.,1.,1.,
1.,1.,1.,1.,1.,1.,1.,1.,1.,1.,1.,1.,1.,1.,1.,1.,1.,1.,1.,1.,1.,1.,1.,1.,
1.,1.,1.,1.,1.,1.,1.,1.,1.,1.,1.,1.,1.,1.,1.,1.,1.,1.,1.,1.,1.,1.,1.,1.,
1.,1.,1.,1.,1.,1.))
REPRESENTATION_ITEM('')
);
#332=(
BOUNDED_CURVE()
B_SPLINE_CURVE(5,(#53835,#53836,#53837,#53838,#53839,#53840,#53841,#53842,
#53843,#53844,#53845,#53846,#53847,#53848,#53849,#53850,#53851,#53852,#53853,
#53854,#53855,#53856,#53857,#53858,#53859,#53860,#53861,#53862,#53863,#53864,
#53865,#53866,#53867,#53868,#53869,#53870,#53871,#53872,#53873,#53874,#53875,
#53876,#53877,#53878,#53879,#53880,#53881,#53882,#53883,#53884,#53885,#53886,
#53887,#53888,#53889,#53890,#53891,#53892,#53893,#53894,#53895,#53896,#53897,
#53898,#53899,#53900,#53901,#53902,#53903,#53904),.UNSPECIFIED.,.F.,.F.)
B_SPLINE_CURVE_WITH_KNOTS((6,1,1,1,1,1,1,1,1,1,1,1,1,1,1,1,1,1,1,1,1,1,
1,1,1,1,1,1,1,1,1,1,1,1,1,1,1,1,1,1,1,1,1,1,1,1,1,1,1,1,1,1,1,1,1,1,1,1,
1,1,1,1,1,1,1,6),(-0.99422815673972,-0.984615384615383,-0.969230769230768,
-0.953846153846152,-0.938461538461537,-0.923076923076922,-0.907692307692306,
-0.892307692307691,-0.876923076923076,-0.86153846153846,-0.846153846153845,
-0.83076923076923,-0.815384615384614,-0.799999999999999,-0.784615384615384,
-0.769230769230768,-0.753846153846153,-0.738461538461538,-0.723076923076922,
-0.707692307692307,-0.692307692307692,-0.676923076923076,-0.661538461538461,
-0.646153846153846,-0.63076923076923,-0.615384615384615,-0.6,-0.584615384615384,
-0.569230769230769,-0.553846153846154,-0.538461538461538,-0.523076923076923,
-0.507692307692308,-0.492307692307692,-0.476923076923077,-0.461538461538462,
-0.446153846153846,-0.430769230769231,-0.415384615384615,-0.4,-0.384615384615385,
-0.369230769230769,-0.353846153846154,-0.338461538461538,-0.323076923076923,
-0.307692307692308,-0.292307692307692,-0.276923076923077,-0.261538461538462,
-0.246153846153846,-0.230769230769231,-0.215384615384615,-0.2,-0.184615384615385,
-0.169230769230769,-0.153846153846154,-0.138461538461538,-0.123076923076923,
-0.107692307692308,-0.0923076923076923,-0.0769230769230769,-0.0615384615384615,
-0.0461538461538462,-0.0307692307692308,-0.0153846153846154,0.),
 .UNSPECIFIED.)
CURVE()
GEOMETRIC_REPRESENTATION_ITEM()
RATIONAL_B_SPLINE_CURVE((1.,1.,1.,1.,1.,1.,1.,1.,1.,1.,1.,1.,1.,1.,1.,1.,
1.,1.,1.,1.,1.,1.,1.,1.,1.,1.,1.,1.,1.,1.,1.,1.,1.,1.,1.,1.,1.,1.,1.,1.,
1.,1.,1.,1.,1.,1.,1.,1.,1.,1.,1.,1.,1.,1.,1.,1.,1.,1.,1.,1.,1.,1.,1.,1.,
1.,1.,1.,1.,1.,1.))
REPRESENTATION_ITEM('')
);
#333=(
BOUNDED_CURVE()
B_SPLINE_CURVE(5,(#54057,#54058,#54059,#54060,#54061,#54062,#54063,#54064,
#54065,#54066,#54067,#54068,#54069,#54070,#54071,#54072,#54073,#54074,#54075,
#54076,#54077,#54078,#54079,#54080,#54081,#54082,#54083,#54084,#54085,#54086,
#54087,#54088,#54089,#54090,#54091,#54092,#54093,#54094,#54095,#54096,#54097,
#54098,#54099,#54100,#54101,#54102,#54103,#54104,#54105,#54106,#54107,#54108,
#54109,#54110,#54111,#54112,#54113,#54114,#54115,#54116,#54117,#54118,#54119,
#54120,#54121,#54122,#54123,#54124,#54125,#54126),.UNSPECIFIED.,.F.,.F.)
B_SPLINE_CURVE_WITH_KNOTS((6,1,1,1,1,1,1,1,1,1,1,1,1,1,1,1,1,1,1,1,1,1,
1,1,1,1,1,1,1,1,1,1,1,1,1,1,1,1,1,1,1,1,1,1,1,1,1,1,1,1,1,1,1,1,1,1,1,1,
1,1,1,1,1,1,1,6),(-1.,-0.984615384615383,-0.969230769230768,-0.953846153846152,
-0.938461538461537,-0.923076923076922,-0.907692307692306,-0.892307692307691,
-0.876923076923076,-0.86153846153846,-0.846153846153845,-0.83076923076923,
-0.815384615384614,-0.799999999999999,-0.784615384615384,-0.769230769230768,
-0.753846153846153,-0.738461538461538,-0.723076923076922,-0.707692307692307,
-0.692307692307692,-0.676923076923076,-0.661538461538461,-0.646153846153846,
-0.63076923076923,-0.615384615384615,-0.6,-0.584615384615384,-0.569230769230769,
-0.553846153846154,-0.538461538461538,-0.523076923076923,-0.507692307692308,
-0.492307692307692,-0.476923076923077,-0.461538461538462,-0.446153846153846,
-0.430769230769231,-0.415384615384615,-0.4,-0.384615384615385,-0.369230769230769,
-0.353846153846154,-0.338461538461538,-0.323076923076923,-0.307692307692308,
-0.292307692307692,-0.276923076923077,-0.261538461538462,-0.246153846153846,
-0.230769230769231,-0.215384615384615,-0.2,-0.184615384615385,-0.169230769230769,
-0.153846153846154,-0.138461538461538,-0.123076923076923,-0.107692307692308,
-0.0923076923076923,-0.0769230769230769,-0.0615384615384615,-0.0461538461538462,
-0.0307692307692308,-0.0153846153846154,-0.0057718433745107),
 .UNSPECIFIED.)
CURVE()
GEOMETRIC_REPRESENTATION_ITEM()
RATIONAL_B_SPLINE_CURVE((1.,1.,1.,1.,1.,1.,1.,1.,1.,1.,1.,1.,1.,1.,1.,1.,
1.,1.,1.,1.,1.,1.,1.,1.,1.,1.,1.,1.,1.,1.,1.,1.,1.,1.,1.,1.,1.,1.,1.,1.,
1.,1.,1.,1.,1.,1.,1.,1.,1.,1.,1.,1.,1.,1.,1.,1.,1.,1.,1.,1.,1.,1.,1.,1.,
1.,1.,1.,1.,1.,1.))
REPRESENTATION_ITEM('')
);
#334=(
BOUNDED_CURVE()
B_SPLINE_CURVE(5,(#54277,#54278,#54279,#54280,#54281,#54282,#54283,#54284,
#54285,#54286,#54287,#54288,#54289,#54290,#54291,#54292,#54293,#54294,#54295,
#54296,#54297,#54298,#54299,#54300,#54301,#54302,#54303,#54304,#54305,#54306,
#54307,#54308,#54309,#54310,#54311,#54312,#54313,#54314,#54315,#54316,#54317,
#54318,#54319,#54320,#54321,#54322,#54323,#54324,#54325,#54326,#54327,#54328,
#54329,#54330,#54331,#54332,#54333,#54334,#54335,#54336,#54337,#54338,#54339,
#54340,#54341,#54342,#54343,#54344,#54345,#54346),.UNSPECIFIED.,.F.,.F.)
B_SPLINE_CURVE_WITH_KNOTS((6,1,1,1,1,1,1,1,1,1,1,1,1,1,1,1,1,1,1,1,1,1,
1,1,1,1,1,1,1,1,1,1,1,1,1,1,1,1,1,1,1,1,1,1,1,1,1,1,1,1,1,1,1,1,1,1,1,1,
1,1,1,1,1,1,1,6),(-0.994228156739708,-0.984615384615383,-0.969230769230768,
-0.953846153846152,-0.938461538461537,-0.923076923076922,-0.907692307692306,
-0.892307692307691,-0.876923076923076,-0.86153846153846,-0.846153846153845,
-0.83076923076923,-0.815384615384614,-0.799999999999999,-0.784615384615384,
-0.769230769230768,-0.753846153846153,-0.738461538461538,-0.723076923076922,
-0.707692307692307,-0.692307692307692,-0.676923076923076,-0.661538461538461,
-0.646153846153846,-0.63076923076923,-0.615384615384615,-0.6,-0.584615384615384,
-0.569230769230769,-0.553846153846154,-0.538461538461538,-0.523076923076923,
-0.507692307692308,-0.492307692307692,-0.476923076923077,-0.461538461538462,
-0.446153846153846,-0.430769230769231,-0.415384615384615,-0.4,-0.384615384615385,
-0.369230769230769,-0.353846153846154,-0.338461538461538,-0.323076923076923,
-0.307692307692308,-0.292307692307692,-0.276923076923077,-0.261538461538462,
-0.246153846153846,-0.230769230769231,-0.215384615384615,-0.2,-0.184615384615385,
-0.169230769230769,-0.153846153846154,-0.138461538461538,-0.123076923076923,
-0.107692307692308,-0.0923076923076923,-0.0769230769230769,-0.0615384615384615,
-0.0461538461538462,-0.0307692307692308,-0.0153846153846154,0.),
 .UNSPECIFIED.)
CURVE()
GEOMETRIC_REPRESENTATION_ITEM()
RATIONAL_B_SPLINE_CURVE((1.,1.,1.,1.,1.,1.,1.,1.,1.,1.,1.,1.,1.,1.,1.,1.,
1.,1.,1.,1.,1.,1.,1.,1.,1.,1.,1.,1.,1.,1.,1.,1.,1.,1.,1.,1.,1.,1.,1.,1.,
1.,1.,1.,1.,1.,1.,1.,1.,1.,1.,1.,1.,1.,1.,1.,1.,1.,1.,1.,1.,1.,1.,1.,1.,
1.,1.,1.,1.,1.,1.))
REPRESENTATION_ITEM('')
);
#335=(
BOUNDED_CURVE()
B_SPLINE_CURVE(5,(#54499,#54500,#54501,#54502,#54503,#54504,#54505,#54506,
#54507,#54508,#54509,#54510,#54511,#54512,#54513,#54514,#54515,#54516,#54517,
#54518,#54519,#54520,#54521,#54522,#54523,#54524,#54525,#54526,#54527,#54528,
#54529,#54530,#54531,#54532,#54533,#54534,#54535,#54536,#54537,#54538,#54539,
#54540,#54541,#54542,#54543,#54544,#54545,#54546,#54547,#54548,#54549,#54550,
#54551,#54552,#54553,#54554,#54555,#54556,#54557,#54558,#54559,#54560,#54561,
#54562,#54563,#54564,#54565,#54566,#54567,#54568),.UNSPECIFIED.,.F.,.F.)
B_SPLINE_CURVE_WITH_KNOTS((6,1,1,1,1,1,1,1,1,1,1,1,1,1,1,1,1,1,1,1,1,1,
1,1,1,1,1,1,1,1,1,1,1,1,1,1,1,1,1,1,1,1,1,1,1,1,1,1,1,1,1,1,1,1,1,1,1,1,
1,1,1,1,1,1,1,6),(-1.,-0.984615384615383,-0.969230769230768,-0.953846153846152,
-0.938461538461537,-0.923076923076922,-0.907692307692306,-0.892307692307691,
-0.876923076923076,-0.86153846153846,-0.846153846153845,-0.83076923076923,
-0.815384615384614,-0.799999999999999,-0.784615384615384,-0.769230769230768,
-0.753846153846153,-0.738461538461538,-0.723076923076922,-0.707692307692307,
-0.692307692307692,-0.676923076923076,-0.661538461538461,-0.646153846153846,
-0.63076923076923,-0.615384615384615,-0.6,-0.584615384615384,-0.569230769230769,
-0.553846153846154,-0.538461538461538,-0.523076923076923,-0.507692307692308,
-0.492307692307692,-0.476923076923077,-0.461538461538462,-0.446153846153846,
-0.430769230769231,-0.415384615384615,-0.4,-0.384615384615385,-0.369230769230769,
-0.353846153846154,-0.338461538461538,-0.323076923076923,-0.307692307692308,
-0.292307692307692,-0.276923076923077,-0.261538461538462,-0.246153846153846,
-0.230769230769231,-0.215384615384615,-0.2,-0.184615384615385,-0.169230769230769,
-0.153846153846154,-0.138461538461538,-0.123076923076923,-0.107692307692308,
-0.0923076923076923,-0.0769230769230769,-0.0615384615384615,-0.0461538461538462,
-0.0307692307692308,-0.0153846153846154,-0.00577184337451708),
 .UNSPECIFIED.)
CURVE()
GEOMETRIC_REPRESENTATION_ITEM()
RATIONAL_B_SPLINE_CURVE((1.,1.,1.,1.,1.,1.,1.,1.,1.,1.,1.,1.,1.,1.,1.,1.,
1.,1.,1.,1.,1.,1.,1.,1.,1.,1.,1.,1.,1.,1.,1.,1.,1.,1.,1.,1.,1.,1.,1.,1.,
1.,1.,1.,1.,1.,1.,1.,1.,1.,1.,1.,1.,1.,1.,1.,1.,1.,1.,1.,1.,1.,1.,1.,1.,
1.,1.,1.,1.,1.,1.))
REPRESENTATION_ITEM('')
);
#336=(
BOUNDED_CURVE()
B_SPLINE_CURVE(5,(#54719,#54720,#54721,#54722,#54723,#54724,#54725,#54726,
#54727,#54728,#54729,#54730,#54731,#54732,#54733,#54734,#54735,#54736,#54737,
#54738,#54739,#54740,#54741,#54742,#54743,#54744,#54745,#54746,#54747,#54748,
#54749,#54750,#54751,#54752,#54753,#54754,#54755,#54756,#54757,#54758,#54759,
#54760,#54761,#54762,#54763,#54764,#54765,#54766,#54767,#54768,#54769,#54770,
#54771,#54772,#54773,#54774,#54775,#54776,#54777,#54778,#54779,#54780,#54781,
#54782,#54783,#54784,#54785,#54786,#54787,#54788),.UNSPECIFIED.,.F.,.F.)
B_SPLINE_CURVE_WITH_KNOTS((6,1,1,1,1,1,1,1,1,1,1,1,1,1,1,1,1,1,1,1,1,1,
1,1,1,1,1,1,1,1,1,1,1,1,1,1,1,1,1,1,1,1,1,1,1,1,1,1,1,1,1,1,1,1,1,1,1,1,
1,1,1,1,1,1,1,6),(-0.994228156739669,-0.984615384615383,-0.969230769230768,
-0.953846153846152,-0.938461538461537,-0.923076923076922,-0.907692307692306,
-0.892307692307691,-0.876923076923076,-0.86153846153846,-0.846153846153845,
-0.83076923076923,-0.815384615384614,-0.799999999999999,-0.784615384615384,
-0.769230769230768,-0.753846153846153,-0.738461538461538,-0.723076923076922,
-0.707692307692307,-0.692307692307692,-0.676923076923076,-0.661538461538461,
-0.646153846153846,-0.63076923076923,-0.615384615384615,-0.6,-0.584615384615384,
-0.569230769230769,-0.553846153846154,-0.538461538461538,-0.523076923076923,
-0.507692307692308,-0.492307692307692,-0.476923076923077,-0.461538461538462,
-0.446153846153846,-0.430769230769231,-0.415384615384615,-0.4,-0.384615384615385,
-0.369230769230769,-0.353846153846154,-0.338461538461538,-0.323076923076923,
-0.307692307692308,-0.292307692307692,-0.276923076923077,-0.261538461538462,
-0.246153846153846,-0.230769230769231,-0.215384615384615,-0.2,-0.184615384615385,
-0.169230769230769,-0.153846153846154,-0.138461538461538,-0.123076923076923,
-0.107692307692308,-0.0923076923076923,-0.0769230769230769,-0.0615384615384615,
-0.0461538461538462,-0.0307692307692308,-0.0153846153846154,0.),
 .UNSPECIFIED.)
CURVE()
GEOMETRIC_REPRESENTATION_ITEM()
RATIONAL_B_SPLINE_CURVE((1.,1.,1.,1.,1.,1.,1.,1.,1.,1.,1.,1.,1.,1.,1.,1.,
1.,1.,1.,1.,1.,1.,1.,1.,1.,1.,1.,1.,1.,1.,1.,1.,1.,1.,1.,1.,1.,1.,1.,1.,
1.,1.,1.,1.,1.,1.,1.,1.,1.,1.,1.,1.,1.,1.,1.,1.,1.,1.,1.,1.,1.,1.,1.,1.,
1.,1.,1.,1.,1.,1.))
REPRESENTATION_ITEM('')
);
#337=(
BOUNDED_CURVE()
B_SPLINE_CURVE(5,(#54941,#54942,#54943,#54944,#54945,#54946,#54947,#54948,
#54949,#54950,#54951,#54952,#54953,#54954,#54955,#54956,#54957,#54958,#54959,
#54960,#54961,#54962,#54963,#54964,#54965,#54966,#54967,#54968,#54969,#54970,
#54971,#54972,#54973,#54974,#54975,#54976,#54977,#54978,#54979,#54980,#54981,
#54982,#54983,#54984,#54985,#54986,#54987,#54988,#54989,#54990,#54991,#54992,
#54993,#54994,#54995,#54996,#54997,#54998,#54999,#55000,#55001,#55002,#55003,
#55004,#55005,#55006,#55007,#55008,#55009,#55010),.UNSPECIFIED.,.F.,.F.)
B_SPLINE_CURVE_WITH_KNOTS((6,1,1,1,1,1,1,1,1,1,1,1,1,1,1,1,1,1,1,1,1,1,
1,1,1,1,1,1,1,1,1,1,1,1,1,1,1,1,1,1,1,1,1,1,1,1,1,1,1,1,1,1,1,1,1,1,1,1,
1,1,1,1,1,1,1,6),(-1.,-0.984615384615383,-0.969230769230768,-0.953846153846152,
-0.938461538461537,-0.923076923076922,-0.907692307692306,-0.892307692307691,
-0.876923076923076,-0.86153846153846,-0.846153846153845,-0.83076923076923,
-0.815384615384614,-0.799999999999999,-0.784615384615384,-0.769230769230768,
-0.753846153846153,-0.738461538461538,-0.723076923076922,-0.707692307692307,
-0.692307692307692,-0.676923076923076,-0.661538461538461,-0.646153846153846,
-0.63076923076923,-0.615384615384615,-0.6,-0.584615384615384,-0.569230769230769,
-0.553846153846154,-0.538461538461538,-0.523076923076923,-0.507692307692308,
-0.492307692307692,-0.476923076923077,-0.461538461538462,-0.446153846153846,
-0.430769230769231,-0.415384615384615,-0.4,-0.384615384615385,-0.369230769230769,
-0.353846153846154,-0.338461538461538,-0.323076923076923,-0.307692307692308,
-0.292307692307692,-0.276923076923077,-0.261538461538462,-0.246153846153846,
-0.230769230769231,-0.215384615384615,-0.2,-0.184615384615385,-0.169230769230769,
-0.153846153846154,-0.138461538461538,-0.123076923076923,-0.107692307692308,
-0.0923076923076923,-0.0769230769230769,-0.0615384615384615,-0.0461538461538462,
-0.0307692307692308,-0.0153846153846154,-0.0057718433744903),
 .UNSPECIFIED.)
CURVE()
GEOMETRIC_REPRESENTATION_ITEM()
RATIONAL_B_SPLINE_CURVE((1.,1.,1.,1.,1.,1.,1.,1.,1.,1.,1.,1.,1.,1.,1.,1.,
1.,1.,1.,1.,1.,1.,1.,1.,1.,1.,1.,1.,1.,1.,1.,1.,1.,1.,1.,1.,1.,1.,1.,1.,
1.,1.,1.,1.,1.,1.,1.,1.,1.,1.,1.,1.,1.,1.,1.,1.,1.,1.,1.,1.,1.,1.,1.,1.,
1.,1.,1.,1.,1.,1.))
REPRESENTATION_ITEM('')
);
#338=(
BOUNDED_CURVE()
B_SPLINE_CURVE(5,(#55161,#55162,#55163,#55164,#55165,#55166,#55167,#55168,
#55169,#55170,#55171,#55172,#55173,#55174,#55175,#55176,#55177,#55178,#55179,
#55180,#55181,#55182,#55183,#55184,#55185,#55186,#55187,#55188,#55189,#55190,
#55191,#55192,#55193,#55194,#55195,#55196,#55197,#55198,#55199,#55200,#55201,
#55202,#55203,#55204,#55205,#55206,#55207,#55208,#55209,#55210,#55211,#55212,
#55213,#55214,#55215,#55216,#55217,#55218,#55219,#55220,#55221,#55222,#55223,
#55224,#55225,#55226,#55227,#55228,#55229,#55230),.UNSPECIFIED.,.F.,.F.)
B_SPLINE_CURVE_WITH_KNOTS((6,1,1,1,1,1,1,1,1,1,1,1,1,1,1,1,1,1,1,1,1,1,
1,1,1,1,1,1,1,1,1,1,1,1,1,1,1,1,1,1,1,1,1,1,1,1,1,1,1,1,1,1,1,1,1,1,1,1,
1,1,1,1,1,1,1,6),(-0.994228156739712,-0.984615384615383,-0.969230769230768,
-0.953846153846152,-0.938461538461537,-0.923076923076922,-0.907692307692306,
-0.892307692307691,-0.876923076923076,-0.86153846153846,-0.846153846153845,
-0.83076923076923,-0.815384615384614,-0.799999999999999,-0.784615384615384,
-0.769230769230768,-0.753846153846153,-0.738461538461538,-0.723076923076922,
-0.707692307692307,-0.692307692307692,-0.676923076923076,-0.661538461538461,
-0.646153846153846,-0.63076923076923,-0.615384615384615,-0.6,-0.584615384615384,
-0.569230769230769,-0.553846153846154,-0.538461538461538,-0.523076923076923,
-0.507692307692308,-0.492307692307692,-0.476923076923077,-0.461538461538462,
-0.446153846153846,-0.430769230769231,-0.415384615384615,-0.4,-0.384615384615385,
-0.369230769230769,-0.353846153846154,-0.338461538461538,-0.323076923076923,
-0.307692307692308,-0.292307692307692,-0.276923076923077,-0.261538461538462,
-0.246153846153846,-0.230769230769231,-0.215384615384615,-0.2,-0.184615384615385,
-0.169230769230769,-0.153846153846154,-0.138461538461538,-0.123076923076923,
-0.107692307692308,-0.0923076923076923,-0.0769230769230769,-0.0615384615384615,
-0.0461538461538462,-0.0307692307692308,-0.0153846153846154,0.),
 .UNSPECIFIED.)
CURVE()
GEOMETRIC_REPRESENTATION_ITEM()
RATIONAL_B_SPLINE_CURVE((1.,1.,1.,1.,1.,1.,1.,1.,1.,1.,1.,1.,1.,1.,1.,1.,
1.,1.,1.,1.,1.,1.,1.,1.,1.,1.,1.,1.,1.,1.,1.,1.,1.,1.,1.,1.,1.,1.,1.,1.,
1.,1.,1.,1.,1.,1.,1.,1.,1.,1.,1.,1.,1.,1.,1.,1.,1.,1.,1.,1.,1.,1.,1.,1.,
1.,1.,1.,1.,1.,1.))
REPRESENTATION_ITEM('')
);
#339=(
BOUNDED_CURVE()
B_SPLINE_CURVE(5,(#55383,#55384,#55385,#55386,#55387,#55388,#55389,#55390,
#55391,#55392,#55393,#55394,#55395,#55396,#55397,#55398,#55399,#55400,#55401,
#55402,#55403,#55404,#55405,#55406,#55407,#55408,#55409,#55410,#55411,#55412,
#55413,#55414,#55415,#55416,#55417,#55418,#55419,#55420,#55421,#55422,#55423,
#55424,#55425,#55426,#55427,#55428,#55429,#55430,#55431,#55432,#55433,#55434,
#55435,#55436,#55437,#55438,#55439,#55440,#55441,#55442,#55443,#55444,#55445,
#55446,#55447,#55448,#55449,#55450,#55451,#55452),.UNSPECIFIED.,.F.,.F.)
B_SPLINE_CURVE_WITH_KNOTS((6,1,1,1,1,1,1,1,1,1,1,1,1,1,1,1,1,1,1,1,1,1,
1,1,1,1,1,1,1,1,1,1,1,1,1,1,1,1,1,1,1,1,1,1,1,1,1,1,1,1,1,1,1,1,1,1,1,1,
1,1,1,1,1,1,1,6),(-1.,-0.984615384615383,-0.969230769230768,-0.953846153846152,
-0.938461538461537,-0.923076923076922,-0.907692307692306,-0.892307692307691,
-0.876923076923076,-0.86153846153846,-0.846153846153845,-0.83076923076923,
-0.815384615384614,-0.799999999999999,-0.784615384615384,-0.769230769230768,
-0.753846153846153,-0.738461538461538,-0.723076923076922,-0.707692307692307,
-0.692307692307692,-0.676923076923076,-0.661538461538461,-0.646153846153846,
-0.63076923076923,-0.615384615384615,-0.6,-0.584615384615384,-0.569230769230769,
-0.553846153846154,-0.538461538461538,-0.523076923076923,-0.507692307692308,
-0.492307692307692,-0.476923076923077,-0.461538461538462,-0.446153846153846,
-0.430769230769231,-0.415384615384615,-0.4,-0.384615384615385,-0.369230769230769,
-0.353846153846154,-0.338461538461538,-0.323076923076923,-0.307692307692308,
-0.292307692307692,-0.276923076923077,-0.261538461538462,-0.246153846153846,
-0.230769230769231,-0.215384615384615,-0.2,-0.184615384615385,-0.169230769230769,
-0.153846153846154,-0.138461538461538,-0.123076923076923,-0.107692307692308,
-0.0923076923076923,-0.0769230769230769,-0.0615384615384615,-0.0461538461538462,
-0.0307692307692308,-0.0153846153846154,-0.0057718433745291),
 .UNSPECIFIED.)
CURVE()
GEOMETRIC_REPRESENTATION_ITEM()
RATIONAL_B_SPLINE_CURVE((1.,1.,1.,1.,1.,1.,1.,1.,1.,1.,1.,1.,1.,1.,1.,1.,
1.,1.,1.,1.,1.,1.,1.,1.,1.,1.,1.,1.,1.,1.,1.,1.,1.,1.,1.,1.,1.,1.,1.,1.,
1.,1.,1.,1.,1.,1.,1.,1.,1.,1.,1.,1.,1.,1.,1.,1.,1.,1.,1.,1.,1.,1.,1.,1.,
1.,1.,1.,1.,1.,1.))
REPRESENTATION_ITEM('')
);
#340=(
BOUNDED_CURVE()
B_SPLINE_CURVE(5,(#55603,#55604,#55605,#55606,#55607,#55608,#55609,#55610,
#55611,#55612,#55613,#55614,#55615,#55616,#55617,#55618,#55619,#55620,#55621,
#55622,#55623,#55624,#55625,#55626,#55627,#55628,#55629,#55630,#55631,#55632,
#55633,#55634,#55635,#55636,#55637,#55638,#55639,#55640,#55641,#55642,#55643,
#55644,#55645,#55646,#55647,#55648,#55649,#55650,#55651,#55652,#55653,#55654,
#55655,#55656,#55657,#55658,#55659,#55660,#55661,#55662,#55663,#55664,#55665,
#55666,#55667,#55668,#55669,#55670,#55671,#55672),.UNSPECIFIED.,.F.,.F.)
B_SPLINE_CURVE_WITH_KNOTS((6,1,1,1,1,1,1,1,1,1,1,1,1,1,1,1,1,1,1,1,1,1,
1,1,1,1,1,1,1,1,1,1,1,1,1,1,1,1,1,1,1,1,1,1,1,1,1,1,1,1,1,1,1,1,1,1,1,1,
1,1,1,1,1,1,1,6),(-0.994228156739695,-0.984615384615383,-0.969230769230768,
-0.953846153846152,-0.938461538461537,-0.923076923076922,-0.907692307692306,
-0.892307692307691,-0.876923076923076,-0.86153846153846,-0.846153846153845,
-0.83076923076923,-0.815384615384614,-0.799999999999999,-0.784615384615384,
-0.769230769230768,-0.753846153846153,-0.738461538461538,-0.723076923076922,
-0.707692307692307,-0.692307692307692,-0.676923076923076,-0.661538461538461,
-0.646153846153846,-0.63076923076923,-0.615384615384615,-0.6,-0.584615384615384,
-0.569230769230769,-0.553846153846154,-0.538461538461538,-0.523076923076923,
-0.507692307692308,-0.492307692307692,-0.476923076923077,-0.461538461538462,
-0.446153846153846,-0.430769230769231,-0.415384615384615,-0.4,-0.384615384615385,
-0.369230769230769,-0.353846153846154,-0.338461538461538,-0.323076923076923,
-0.307692307692308,-0.292307692307692,-0.276923076923077,-0.261538461538462,
-0.246153846153846,-0.230769230769231,-0.215384615384615,-0.2,-0.184615384615385,
-0.169230769230769,-0.153846153846154,-0.138461538461538,-0.123076923076923,
-0.107692307692308,-0.0923076923076923,-0.0769230769230769,-0.0615384615384615,
-0.0461538461538462,-0.0307692307692308,-0.0153846153846154,0.),
 .UNSPECIFIED.)
CURVE()
GEOMETRIC_REPRESENTATION_ITEM()
RATIONAL_B_SPLINE_CURVE((1.,1.,1.,1.,1.,1.,1.,1.,1.,1.,1.,1.,1.,1.,1.,1.,
1.,1.,1.,1.,1.,1.,1.,1.,1.,1.,1.,1.,1.,1.,1.,1.,1.,1.,1.,1.,1.,1.,1.,1.,
1.,1.,1.,1.,1.,1.,1.,1.,1.,1.,1.,1.,1.,1.,1.,1.,1.,1.,1.,1.,1.,1.,1.,1.,
1.,1.,1.,1.,1.,1.))
REPRESENTATION_ITEM('')
);
#341=(
BOUNDED_CURVE()
B_SPLINE_CURVE(5,(#55825,#55826,#55827,#55828,#55829,#55830,#55831,#55832,
#55833,#55834,#55835,#55836,#55837,#55838,#55839,#55840,#55841,#55842,#55843,
#55844,#55845,#55846,#55847,#55848,#55849,#55850,#55851,#55852,#55853,#55854,
#55855,#55856,#55857,#55858,#55859,#55860,#55861,#55862,#55863,#55864,#55865,
#55866,#55867,#55868,#55869,#55870,#55871,#55872,#55873,#55874,#55875,#55876,
#55877,#55878,#55879,#55880,#55881,#55882,#55883,#55884,#55885,#55886,#55887,
#55888,#55889,#55890,#55891,#55892,#55893,#55894),.UNSPECIFIED.,.F.,.F.)
B_SPLINE_CURVE_WITH_KNOTS((6,1,1,1,1,1,1,1,1,1,1,1,1,1,1,1,1,1,1,1,1,1,
1,1,1,1,1,1,1,1,1,1,1,1,1,1,1,1,1,1,1,1,1,1,1,1,1,1,1,1,1,1,1,1,1,1,1,1,
1,1,1,1,1,1,1,6),(-1.,-0.984615384615383,-0.969230769230768,-0.953846153846152,
-0.938461538461537,-0.923076923076922,-0.907692307692306,-0.892307692307691,
-0.876923076923076,-0.86153846153846,-0.846153846153845,-0.83076923076923,
-0.815384615384614,-0.799999999999999,-0.784615384615384,-0.769230769230768,
-0.753846153846153,-0.738461538461538,-0.723076923076922,-0.707692307692307,
-0.692307692307692,-0.676923076923076,-0.661538461538461,-0.646153846153846,
-0.63076923076923,-0.615384615384615,-0.6,-0.584615384615384,-0.569230769230769,
-0.553846153846154,-0.538461538461538,-0.523076923076923,-0.507692307692308,
-0.492307692307692,-0.476923076923077,-0.461538461538462,-0.446153846153846,
-0.430769230769231,-0.415384615384615,-0.4,-0.384615384615385,-0.369230769230769,
-0.353846153846154,-0.338461538461538,-0.323076923076923,-0.307692307692308,
-0.292307692307692,-0.276923076923077,-0.261538461538462,-0.246153846153846,
-0.230769230769231,-0.215384615384615,-0.2,-0.184615384615385,-0.169230769230769,
-0.153846153846154,-0.138461538461538,-0.123076923076923,-0.107692307692308,
-0.0923076923076923,-0.0769230769230769,-0.0615384615384615,-0.0461538461538462,
-0.0307692307692308,-0.0153846153846154,-0.00577184337450344),
 .UNSPECIFIED.)
CURVE()
GEOMETRIC_REPRESENTATION_ITEM()
RATIONAL_B_SPLINE_CURVE((1.,1.,1.,1.,1.,1.,1.,1.,1.,1.,1.,1.,1.,1.,1.,1.,
1.,1.,1.,1.,1.,1.,1.,1.,1.,1.,1.,1.,1.,1.,1.,1.,1.,1.,1.,1.,1.,1.,1.,1.,
1.,1.,1.,1.,1.,1.,1.,1.,1.,1.,1.,1.,1.,1.,1.,1.,1.,1.,1.,1.,1.,1.,1.,1.,
1.,1.,1.,1.,1.,1.))
REPRESENTATION_ITEM('')
);
#342=(
BOUNDED_CURVE()
B_SPLINE_CURVE(5,(#56045,#56046,#56047,#56048,#56049,#56050,#56051,#56052,
#56053,#56054,#56055,#56056,#56057,#56058,#56059,#56060,#56061,#56062,#56063,
#56064,#56065,#56066,#56067,#56068,#56069,#56070,#56071,#56072,#56073,#56074,
#56075,#56076,#56077,#56078,#56079,#56080,#56081,#56082,#56083,#56084,#56085,
#56086,#56087,#56088,#56089,#56090,#56091,#56092,#56093,#56094,#56095,#56096,
#56097,#56098,#56099,#56100,#56101,#56102,#56103,#56104,#56105,#56106,#56107,
#56108,#56109,#56110,#56111,#56112,#56113,#56114),.UNSPECIFIED.,.F.,.F.)
B_SPLINE_CURVE_WITH_KNOTS((6,1,1,1,1,1,1,1,1,1,1,1,1,1,1,1,1,1,1,1,1,1,
1,1,1,1,1,1,1,1,1,1,1,1,1,1,1,1,1,1,1,1,1,1,1,1,1,1,1,1,1,1,1,1,1,1,1,1,
1,1,1,1,1,1,1,6),(-0.994228156739669,-0.984615384615383,-0.969230769230768,
-0.953846153846152,-0.938461538461537,-0.923076923076922,-0.907692307692306,
-0.892307692307691,-0.876923076923076,-0.86153846153846,-0.846153846153845,
-0.83076923076923,-0.815384615384614,-0.799999999999999,-0.784615384615384,
-0.769230769230768,-0.753846153846153,-0.738461538461538,-0.723076923076922,
-0.707692307692307,-0.692307692307692,-0.676923076923076,-0.661538461538461,
-0.646153846153846,-0.63076923076923,-0.615384615384615,-0.6,-0.584615384615384,
-0.569230769230769,-0.553846153846154,-0.538461538461538,-0.523076923076923,
-0.507692307692308,-0.492307692307692,-0.476923076923077,-0.461538461538462,
-0.446153846153846,-0.430769230769231,-0.415384615384615,-0.4,-0.384615384615385,
-0.369230769230769,-0.353846153846154,-0.338461538461538,-0.323076923076923,
-0.307692307692308,-0.292307692307692,-0.276923076923077,-0.261538461538462,
-0.246153846153846,-0.230769230769231,-0.215384615384615,-0.2,-0.184615384615385,
-0.169230769230769,-0.153846153846154,-0.138461538461538,-0.123076923076923,
-0.107692307692308,-0.0923076923076923,-0.0769230769230769,-0.0615384615384615,
-0.0461538461538462,-0.0307692307692308,-0.0153846153846154,0.),
 .UNSPECIFIED.)
CURVE()
GEOMETRIC_REPRESENTATION_ITEM()
RATIONAL_B_SPLINE_CURVE((1.,1.,1.,1.,1.,1.,1.,1.,1.,1.,1.,1.,1.,1.,1.,1.,
1.,1.,1.,1.,1.,1.,1.,1.,1.,1.,1.,1.,1.,1.,1.,1.,1.,1.,1.,1.,1.,1.,1.,1.,
1.,1.,1.,1.,1.,1.,1.,1.,1.,1.,1.,1.,1.,1.,1.,1.,1.,1.,1.,1.,1.,1.,1.,1.,
1.,1.,1.,1.,1.,1.))
REPRESENTATION_ITEM('')
);
#343=(
BOUNDED_CURVE()
B_SPLINE_CURVE(5,(#56267,#56268,#56269,#56270,#56271,#56272,#56273,#56274,
#56275,#56276,#56277,#56278,#56279,#56280,#56281,#56282,#56283,#56284,#56285,
#56286,#56287,#56288,#56289,#56290,#56291,#56292,#56293,#56294,#56295,#56296,
#56297,#56298,#56299,#56300,#56301,#56302,#56303,#56304,#56305,#56306,#56307,
#56308,#56309,#56310,#56311,#56312,#56313,#56314,#56315,#56316,#56317,#56318,
#56319,#56320,#56321,#56322,#56323,#56324,#56325,#56326,#56327,#56328,#56329,
#56330,#56331,#56332,#56333,#56334,#56335,#56336),.UNSPECIFIED.,.F.,.F.)
B_SPLINE_CURVE_WITH_KNOTS((6,1,1,1,1,1,1,1,1,1,1,1,1,1,1,1,1,1,1,1,1,1,
1,1,1,1,1,1,1,1,1,1,1,1,1,1,1,1,1,1,1,1,1,1,1,1,1,1,1,1,1,1,1,1,1,1,1,1,
1,1,1,1,1,1,1,6),(-1.,-0.984615384615383,-0.969230769230768,-0.953846153846152,
-0.938461538461537,-0.923076923076922,-0.907692307692306,-0.892307692307691,
-0.876923076923076,-0.86153846153846,-0.846153846153845,-0.83076923076923,
-0.815384615384614,-0.799999999999999,-0.784615384615384,-0.769230769230768,
-0.753846153846153,-0.738461538461538,-0.723076923076922,-0.707692307692307,
-0.692307692307692,-0.676923076923076,-0.661538461538461,-0.646153846153846,
-0.63076923076923,-0.615384615384615,-0.6,-0.584615384615384,-0.569230769230769,
-0.553846153846154,-0.538461538461538,-0.523076923076923,-0.507692307692308,
-0.492307692307692,-0.476923076923077,-0.461538461538462,-0.446153846153846,
-0.430769230769231,-0.415384615384615,-0.4,-0.384615384615385,-0.369230769230769,
-0.353846153846154,-0.338461538461538,-0.323076923076923,-0.307692307692308,
-0.292307692307692,-0.276923076923077,-0.261538461538462,-0.246153846153846,
-0.230769230769231,-0.215384615384615,-0.2,-0.184615384615385,-0.169230769230769,
-0.153846153846154,-0.138461538461538,-0.123076923076923,-0.107692307692308,
-0.0923076923076923,-0.0769230769230769,-0.0615384615384615,-0.0461538461538462,
-0.0307692307692308,-0.0153846153846154,-0.00577184337450876),
 .UNSPECIFIED.)
CURVE()
GEOMETRIC_REPRESENTATION_ITEM()
RATIONAL_B_SPLINE_CURVE((1.,1.,1.,1.,1.,1.,1.,1.,1.,1.,1.,1.,1.,1.,1.,1.,
1.,1.,1.,1.,1.,1.,1.,1.,1.,1.,1.,1.,1.,1.,1.,1.,1.,1.,1.,1.,1.,1.,1.,1.,
1.,1.,1.,1.,1.,1.,1.,1.,1.,1.,1.,1.,1.,1.,1.,1.,1.,1.,1.,1.,1.,1.,1.,1.,
1.,1.,1.,1.,1.,1.))
REPRESENTATION_ITEM('')
);
#344=(
BOUNDED_CURVE()
B_SPLINE_CURVE(5,(#56487,#56488,#56489,#56490,#56491,#56492,#56493,#56494,
#56495,#56496,#56497,#56498,#56499,#56500,#56501,#56502,#56503,#56504,#56505,
#56506,#56507,#56508,#56509,#56510,#56511,#56512,#56513,#56514,#56515,#56516,
#56517,#56518,#56519,#56520,#56521,#56522,#56523,#56524,#56525,#56526,#56527,
#56528,#56529,#56530,#56531,#56532,#56533,#56534,#56535,#56536,#56537,#56538,
#56539,#56540,#56541,#56542,#56543,#56544,#56545,#56546,#56547,#56548,#56549,
#56550,#56551,#56552,#56553,#56554,#56555,#56556),.UNSPECIFIED.,.F.,.F.)
B_SPLINE_CURVE_WITH_KNOTS((6,1,1,1,1,1,1,1,1,1,1,1,1,1,1,1,1,1,1,1,1,1,
1,1,1,1,1,1,1,1,1,1,1,1,1,1,1,1,1,1,1,1,1,1,1,1,1,1,1,1,1,1,1,1,1,1,1,1,
1,1,1,1,1,1,1,6),(-0.99422815673966,-0.984615384615383,-0.969230769230768,
-0.953846153846152,-0.938461538461537,-0.923076923076922,-0.907692307692306,
-0.892307692307691,-0.876923076923076,-0.86153846153846,-0.846153846153845,
-0.83076923076923,-0.815384615384614,-0.799999999999999,-0.784615384615384,
-0.769230769230768,-0.753846153846153,-0.738461538461538,-0.723076923076922,
-0.707692307692307,-0.692307692307692,-0.676923076923076,-0.661538461538461,
-0.646153846153846,-0.63076923076923,-0.615384615384615,-0.6,-0.584615384615384,
-0.569230769230769,-0.553846153846154,-0.538461538461538,-0.523076923076923,
-0.507692307692308,-0.492307692307692,-0.476923076923077,-0.461538461538462,
-0.446153846153846,-0.430769230769231,-0.415384615384615,-0.4,-0.384615384615385,
-0.369230769230769,-0.353846153846154,-0.338461538461538,-0.323076923076923,
-0.307692307692308,-0.292307692307692,-0.276923076923077,-0.261538461538462,
-0.246153846153846,-0.230769230769231,-0.215384615384615,-0.2,-0.184615384615385,
-0.169230769230769,-0.153846153846154,-0.138461538461538,-0.123076923076923,
-0.107692307692308,-0.0923076923076923,-0.0769230769230769,-0.0615384615384615,
-0.0461538461538462,-0.0307692307692308,-0.0153846153846154,0.),
 .UNSPECIFIED.)
CURVE()
GEOMETRIC_REPRESENTATION_ITEM()
RATIONAL_B_SPLINE_CURVE((1.,1.,1.,1.,1.,1.,1.,1.,1.,1.,1.,1.,1.,1.,1.,1.,
1.,1.,1.,1.,1.,1.,1.,1.,1.,1.,1.,1.,1.,1.,1.,1.,1.,1.,1.,1.,1.,1.,1.,1.,
1.,1.,1.,1.,1.,1.,1.,1.,1.,1.,1.,1.,1.,1.,1.,1.,1.,1.,1.,1.,1.,1.,1.,1.,
1.,1.,1.,1.,1.,1.))
REPRESENTATION_ITEM('')
);
#345=(
BOUNDED_CURVE()
B_SPLINE_CURVE(5,(#56709,#56710,#56711,#56712,#56713,#56714,#56715,#56716,
#56717,#56718,#56719,#56720,#56721,#56722,#56723,#56724,#56725,#56726,#56727,
#56728,#56729,#56730,#56731,#56732,#56733,#56734,#56735,#56736,#56737,#56738,
#56739,#56740,#56741,#56742,#56743,#56744,#56745,#56746,#56747,#56748,#56749,
#56750,#56751,#56752,#56753,#56754,#56755,#56756,#56757,#56758,#56759,#56760,
#56761,#56762,#56763,#56764,#56765,#56766,#56767,#56768,#56769,#56770,#56771,
#56772,#56773,#56774,#56775,#56776,#56777,#56778),.UNSPECIFIED.,.F.,.F.)
B_SPLINE_CURVE_WITH_KNOTS((6,1,1,1,1,1,1,1,1,1,1,1,1,1,1,1,1,1,1,1,1,1,
1,1,1,1,1,1,1,1,1,1,1,1,1,1,1,1,1,1,1,1,1,1,1,1,1,1,1,1,1,1,1,1,1,1,1,1,
1,1,1,1,1,1,1,6),(-1.,-0.984615384615383,-0.969230769230768,-0.953846153846152,
-0.938461538461537,-0.923076923076922,-0.907692307692306,-0.892307692307691,
-0.876923076923076,-0.86153846153846,-0.846153846153845,-0.83076923076923,
-0.815384615384614,-0.799999999999999,-0.784615384615384,-0.769230769230768,
-0.753846153846153,-0.738461538461538,-0.723076923076922,-0.707692307692307,
-0.692307692307692,-0.676923076923076,-0.661538461538461,-0.646153846153846,
-0.63076923076923,-0.615384615384615,-0.6,-0.584615384615384,-0.569230769230769,
-0.553846153846154,-0.538461538461538,-0.523076923076923,-0.507692307692308,
-0.492307692307692,-0.476923076923077,-0.461538461538462,-0.446153846153846,
-0.430769230769231,-0.415384615384615,-0.4,-0.384615384615385,-0.369230769230769,
-0.353846153846154,-0.338461538461538,-0.323076923076923,-0.307692307692308,
-0.292307692307692,-0.276923076923077,-0.261538461538462,-0.246153846153846,
-0.230769230769231,-0.215384615384615,-0.2,-0.184615384615385,-0.169230769230769,
-0.153846153846154,-0.138461538461538,-0.123076923076923,-0.107692307692308,
-0.0923076923076923,-0.0769230769230769,-0.0615384615384615,-0.0461538461538462,
-0.0307692307692308,-0.0153846153846154,-0.00577184337451051),
 .UNSPECIFIED.)
CURVE()
GEOMETRIC_REPRESENTATION_ITEM()
RATIONAL_B_SPLINE_CURVE((1.,1.,1.,1.,1.,1.,1.,1.,1.,1.,1.,1.,1.,1.,1.,1.,
1.,1.,1.,1.,1.,1.,1.,1.,1.,1.,1.,1.,1.,1.,1.,1.,1.,1.,1.,1.,1.,1.,1.,1.,
1.,1.,1.,1.,1.,1.,1.,1.,1.,1.,1.,1.,1.,1.,1.,1.,1.,1.,1.,1.,1.,1.,1.,1.,
1.,1.,1.,1.,1.,1.))
REPRESENTATION_ITEM('')
);
#346=(
BOUNDED_CURVE()
B_SPLINE_CURVE(5,(#56929,#56930,#56931,#56932,#56933,#56934,#56935,#56936,
#56937,#56938,#56939,#56940,#56941,#56942,#56943,#56944,#56945,#56946,#56947,
#56948,#56949,#56950,#56951,#56952,#56953,#56954,#56955,#56956,#56957,#56958,
#56959,#56960,#56961,#56962,#56963,#56964,#56965,#56966,#56967,#56968,#56969,
#56970,#56971,#56972,#56973,#56974,#56975,#56976,#56977,#56978,#56979,#56980,
#56981,#56982,#56983,#56984,#56985,#56986,#56987,#56988,#56989,#56990,#56991,
#56992,#56993,#56994,#56995,#56996,#56997,#56998),.UNSPECIFIED.,.F.,.F.)
B_SPLINE_CURVE_WITH_KNOTS((6,1,1,1,1,1,1,1,1,1,1,1,1,1,1,1,1,1,1,1,1,1,
1,1,1,1,1,1,1,1,1,1,1,1,1,1,1,1,1,1,1,1,1,1,1,1,1,1,1,1,1,1,1,1,1,1,1,1,
1,1,1,1,1,1,1,6),(-0.994228156739678,-0.984615384615383,-0.969230769230768,
-0.953846153846152,-0.938461538461537,-0.923076923076922,-0.907692307692306,
-0.892307692307691,-0.876923076923076,-0.86153846153846,-0.846153846153845,
-0.83076923076923,-0.815384615384614,-0.799999999999999,-0.784615384615384,
-0.769230769230768,-0.753846153846153,-0.738461538461538,-0.723076923076922,
-0.707692307692307,-0.692307692307692,-0.676923076923076,-0.661538461538461,
-0.646153846153846,-0.63076923076923,-0.615384615384615,-0.6,-0.584615384615384,
-0.569230769230769,-0.553846153846154,-0.538461538461538,-0.523076923076923,
-0.507692307692308,-0.492307692307692,-0.476923076923077,-0.461538461538462,
-0.446153846153846,-0.430769230769231,-0.415384615384615,-0.4,-0.384615384615385,
-0.369230769230769,-0.353846153846154,-0.338461538461538,-0.323076923076923,
-0.307692307692308,-0.292307692307692,-0.276923076923077,-0.261538461538462,
-0.246153846153846,-0.230769230769231,-0.215384615384615,-0.2,-0.184615384615385,
-0.169230769230769,-0.153846153846154,-0.138461538461538,-0.123076923076923,
-0.107692307692308,-0.0923076923076923,-0.0769230769230769,-0.0615384615384615,
-0.0461538461538462,-0.0307692307692308,-0.0153846153846154,0.),
 .UNSPECIFIED.)
CURVE()
GEOMETRIC_REPRESENTATION_ITEM()
RATIONAL_B_SPLINE_CURVE((1.,1.,1.,1.,1.,1.,1.,1.,1.,1.,1.,1.,1.,1.,1.,1.,
1.,1.,1.,1.,1.,1.,1.,1.,1.,1.,1.,1.,1.,1.,1.,1.,1.,1.,1.,1.,1.,1.,1.,1.,
1.,1.,1.,1.,1.,1.,1.,1.,1.,1.,1.,1.,1.,1.,1.,1.,1.,1.,1.,1.,1.,1.,1.,1.,
1.,1.,1.,1.,1.,1.))
REPRESENTATION_ITEM('')
);
#347=(
BOUNDED_CURVE()
B_SPLINE_CURVE(5,(#57151,#57152,#57153,#57154,#57155,#57156,#57157,#57158,
#57159,#57160,#57161,#57162,#57163,#57164,#57165,#57166,#57167,#57168,#57169,
#57170,#57171,#57172,#57173,#57174,#57175,#57176,#57177,#57178,#57179,#57180,
#57181,#57182,#57183,#57184,#57185,#57186,#57187,#57188,#57189,#57190,#57191,
#57192,#57193,#57194,#57195,#57196,#57197,#57198,#57199,#57200,#57201,#57202,
#57203,#57204,#57205,#57206,#57207,#57208,#57209,#57210,#57211,#57212,#57213,
#57214,#57215,#57216,#57217,#57218,#57219,#57220),.UNSPECIFIED.,.F.,.F.)
B_SPLINE_CURVE_WITH_KNOTS((6,1,1,1,1,1,1,1,1,1,1,1,1,1,1,1,1,1,1,1,1,1,
1,1,1,1,1,1,1,1,1,1,1,1,1,1,1,1,1,1,1,1,1,1,1,1,1,1,1,1,1,1,1,1,1,1,1,1,
1,1,1,1,1,1,1,6),(-1.,-0.984615384615383,-0.969230769230768,-0.953846153846152,
-0.938461538461537,-0.923076923076922,-0.907692307692306,-0.892307692307691,
-0.876923076923076,-0.86153846153846,-0.846153846153845,-0.83076923076923,
-0.815384615384614,-0.799999999999999,-0.784615384615384,-0.769230769230768,
-0.753846153846153,-0.738461538461538,-0.723076923076922,-0.707692307692307,
-0.692307692307692,-0.676923076923076,-0.661538461538461,-0.646153846153846,
-0.63076923076923,-0.615384615384615,-0.6,-0.584615384615384,-0.569230769230769,
-0.553846153846154,-0.538461538461538,-0.523076923076923,-0.507692307692308,
-0.492307692307692,-0.476923076923077,-0.461538461538462,-0.446153846153846,
-0.430769230769231,-0.415384615384615,-0.4,-0.384615384615385,-0.369230769230769,
-0.353846153846154,-0.338461538461538,-0.323076923076923,-0.307692307692308,
-0.292307692307692,-0.276923076923077,-0.261538461538462,-0.246153846153846,
-0.230769230769231,-0.215384615384615,-0.2,-0.184615384615385,-0.169230769230769,
-0.153846153846154,-0.138461538461538,-0.123076923076923,-0.107692307692308,
-0.0923076923076923,-0.0769230769230769,-0.0615384615384615,-0.0461538461538462,
-0.0307692307692308,-0.0153846153846154,-0.0057718433745179),
 .UNSPECIFIED.)
CURVE()
GEOMETRIC_REPRESENTATION_ITEM()
RATIONAL_B_SPLINE_CURVE((1.,1.,1.,1.,1.,1.,1.,1.,1.,1.,1.,1.,1.,1.,1.,1.,
1.,1.,1.,1.,1.,1.,1.,1.,1.,1.,1.,1.,1.,1.,1.,1.,1.,1.,1.,1.,1.,1.,1.,1.,
1.,1.,1.,1.,1.,1.,1.,1.,1.,1.,1.,1.,1.,1.,1.,1.,1.,1.,1.,1.,1.,1.,1.,1.,
1.,1.,1.,1.,1.,1.))
REPRESENTATION_ITEM('')
);
#348=(
BOUNDED_CURVE()
B_SPLINE_CURVE(5,(#57371,#57372,#57373,#57374,#57375,#57376,#57377,#57378,
#57379,#57380,#57381,#57382,#57383,#57384,#57385,#57386,#57387,#57388,#57389,
#57390,#57391,#57392,#57393,#57394,#57395,#57396,#57397,#57398,#57399,#57400,
#57401,#57402,#57403,#57404,#57405,#57406,#57407,#57408,#57409,#57410,#57411,
#57412,#57413,#57414,#57415,#57416,#57417,#57418,#57419,#57420,#57421,#57422,
#57423,#57424,#57425,#57426,#57427,#57428,#57429,#57430,#57431,#57432,#57433,
#57434,#57435,#57436,#57437,#57438,#57439,#57440),.UNSPECIFIED.,.F.,.F.)
B_SPLINE_CURVE_WITH_KNOTS((6,1,1,1,1,1,1,1,1,1,1,1,1,1,1,1,1,1,1,1,1,1,
1,1,1,1,1,1,1,1,1,1,1,1,1,1,1,1,1,1,1,1,1,1,1,1,1,1,1,1,1,1,1,1,1,1,1,1,
1,1,1,1,1,1,1,6),(-0.99422815673967,-0.984615384615383,-0.969230769230768,
-0.953846153846152,-0.938461538461537,-0.923076923076922,-0.907692307692306,
-0.892307692307691,-0.876923076923076,-0.86153846153846,-0.846153846153845,
-0.83076923076923,-0.815384615384614,-0.799999999999999,-0.784615384615384,
-0.769230769230768,-0.753846153846153,-0.738461538461538,-0.723076923076922,
-0.707692307692307,-0.692307692307692,-0.676923076923076,-0.661538461538461,
-0.646153846153846,-0.63076923076923,-0.615384615384615,-0.6,-0.584615384615384,
-0.569230769230769,-0.553846153846154,-0.538461538461538,-0.523076923076923,
-0.507692307692308,-0.492307692307692,-0.476923076923077,-0.461538461538462,
-0.446153846153846,-0.430769230769231,-0.415384615384615,-0.4,-0.384615384615385,
-0.369230769230769,-0.353846153846154,-0.338461538461538,-0.323076923076923,
-0.307692307692308,-0.292307692307692,-0.276923076923077,-0.261538461538462,
-0.246153846153846,-0.230769230769231,-0.215384615384615,-0.2,-0.184615384615385,
-0.169230769230769,-0.153846153846154,-0.138461538461538,-0.123076923076923,
-0.107692307692308,-0.0923076923076923,-0.0769230769230769,-0.0615384615384615,
-0.0461538461538462,-0.0307692307692308,-0.0153846153846154,0.),
 .UNSPECIFIED.)
CURVE()
GEOMETRIC_REPRESENTATION_ITEM()
RATIONAL_B_SPLINE_CURVE((1.,1.,1.,1.,1.,1.,1.,1.,1.,1.,1.,1.,1.,1.,1.,1.,
1.,1.,1.,1.,1.,1.,1.,1.,1.,1.,1.,1.,1.,1.,1.,1.,1.,1.,1.,1.,1.,1.,1.,1.,
1.,1.,1.,1.,1.,1.,1.,1.,1.,1.,1.,1.,1.,1.,1.,1.,1.,1.,1.,1.,1.,1.,1.,1.,
1.,1.,1.,1.,1.,1.))
REPRESENTATION_ITEM('')
);
#349=(
BOUNDED_CURVE()
B_SPLINE_CURVE(5,(#57593,#57594,#57595,#57596,#57597,#57598,#57599,#57600,
#57601,#57602,#57603,#57604,#57605,#57606,#57607,#57608,#57609,#57610,#57611,
#57612,#57613,#57614,#57615,#57616,#57617,#57618,#57619,#57620,#57621,#57622,
#57623,#57624,#57625,#57626,#57627,#57628,#57629,#57630,#57631,#57632,#57633,
#57634,#57635,#57636,#57637,#57638,#57639,#57640,#57641,#57642,#57643,#57644,
#57645,#57646,#57647,#57648,#57649,#57650,#57651,#57652,#57653,#57654,#57655,
#57656,#57657,#57658,#57659,#57660,#57661,#57662),.UNSPECIFIED.,.F.,.F.)
B_SPLINE_CURVE_WITH_KNOTS((6,1,1,1,1,1,1,1,1,1,1,1,1,1,1,1,1,1,1,1,1,1,
1,1,1,1,1,1,1,1,1,1,1,1,1,1,1,1,1,1,1,1,1,1,1,1,1,1,1,1,1,1,1,1,1,1,1,1,
1,1,1,1,1,1,1,6),(-1.,-0.984615384615383,-0.969230769230768,-0.953846153846152,
-0.938461538461537,-0.923076923076922,-0.907692307692306,-0.892307692307691,
-0.876923076923076,-0.86153846153846,-0.846153846153845,-0.83076923076923,
-0.815384615384614,-0.799999999999999,-0.784615384615384,-0.769230769230768,
-0.753846153846153,-0.738461538461538,-0.723076923076922,-0.707692307692307,
-0.692307692307692,-0.676923076923076,-0.661538461538461,-0.646153846153846,
-0.63076923076923,-0.615384615384615,-0.6,-0.584615384615384,-0.569230769230769,
-0.553846153846154,-0.538461538461538,-0.523076923076923,-0.507692307692308,
-0.492307692307692,-0.476923076923077,-0.461538461538462,-0.446153846153846,
-0.430769230769231,-0.415384615384615,-0.4,-0.384615384615385,-0.369230769230769,
-0.353846153846154,-0.338461538461538,-0.323076923076923,-0.307692307692308,
-0.292307692307692,-0.276923076923077,-0.261538461538462,-0.246153846153846,
-0.230769230769231,-0.215384615384615,-0.2,-0.184615384615385,-0.169230769230769,
-0.153846153846154,-0.138461538461538,-0.123076923076923,-0.107692307692308,
-0.0923076923076923,-0.0769230769230769,-0.0615384615384615,-0.0461538461538462,
-0.0307692307692308,-0.0153846153846154,-0.00577184337452479),
 .UNSPECIFIED.)
CURVE()
GEOMETRIC_REPRESENTATION_ITEM()
RATIONAL_B_SPLINE_CURVE((1.,1.,1.,1.,1.,1.,1.,1.,1.,1.,1.,1.,1.,1.,1.,1.,
1.,1.,1.,1.,1.,1.,1.,1.,1.,1.,1.,1.,1.,1.,1.,1.,1.,1.,1.,1.,1.,1.,1.,1.,
1.,1.,1.,1.,1.,1.,1.,1.,1.,1.,1.,1.,1.,1.,1.,1.,1.,1.,1.,1.,1.,1.,1.,1.,
1.,1.,1.,1.,1.,1.))
REPRESENTATION_ITEM('')
);
#350=(
BOUNDED_CURVE()
B_SPLINE_CURVE(5,(#57813,#57814,#57815,#57816,#57817,#57818,#57819,#57820,
#57821,#57822,#57823,#57824,#57825,#57826,#57827,#57828,#57829,#57830,#57831,
#57832,#57833,#57834,#57835,#57836,#57837,#57838,#57839,#57840,#57841,#57842,
#57843,#57844,#57845,#57846,#57847,#57848,#57849,#57850,#57851,#57852,#57853,
#57854,#57855,#57856,#57857,#57858,#57859,#57860,#57861,#57862,#57863,#57864,
#57865,#57866,#57867,#57868,#57869,#57870,#57871,#57872,#57873,#57874,#57875,
#57876,#57877,#57878,#57879,#57880,#57881,#57882),.UNSPECIFIED.,.F.,.F.)
B_SPLINE_CURVE_WITH_KNOTS((6,1,1,1,1,1,1,1,1,1,1,1,1,1,1,1,1,1,1,1,1,1,
1,1,1,1,1,1,1,1,1,1,1,1,1,1,1,1,1,1,1,1,1,1,1,1,1,1,1,1,1,1,1,1,1,1,1,1,
1,1,1,1,1,1,1,6),(-0.99422815673967,-0.984615384615383,-0.969230769230768,
-0.953846153846152,-0.938461538461537,-0.923076923076922,-0.907692307692306,
-0.892307692307691,-0.876923076923076,-0.86153846153846,-0.846153846153845,
-0.83076923076923,-0.815384615384614,-0.799999999999999,-0.784615384615384,
-0.769230769230768,-0.753846153846153,-0.738461538461538,-0.723076923076922,
-0.707692307692307,-0.692307692307692,-0.676923076923076,-0.661538461538461,
-0.646153846153846,-0.63076923076923,-0.615384615384615,-0.6,-0.584615384615384,
-0.569230769230769,-0.553846153846154,-0.538461538461538,-0.523076923076923,
-0.507692307692308,-0.492307692307692,-0.476923076923077,-0.461538461538462,
-0.446153846153846,-0.430769230769231,-0.415384615384615,-0.4,-0.384615384615385,
-0.369230769230769,-0.353846153846154,-0.338461538461538,-0.323076923076923,
-0.307692307692308,-0.292307692307692,-0.276923076923077,-0.261538461538462,
-0.246153846153846,-0.230769230769231,-0.215384615384615,-0.2,-0.184615384615385,
-0.169230769230769,-0.153846153846154,-0.138461538461538,-0.123076923076923,
-0.107692307692308,-0.0923076923076923,-0.0769230769230769,-0.0615384615384615,
-0.0461538461538462,-0.0307692307692308,-0.0153846153846154,0.),
 .UNSPECIFIED.)
CURVE()
GEOMETRIC_REPRESENTATION_ITEM()
RATIONAL_B_SPLINE_CURVE((1.,1.,1.,1.,1.,1.,1.,1.,1.,1.,1.,1.,1.,1.,1.,1.,
1.,1.,1.,1.,1.,1.,1.,1.,1.,1.,1.,1.,1.,1.,1.,1.,1.,1.,1.,1.,1.,1.,1.,1.,
1.,1.,1.,1.,1.,1.,1.,1.,1.,1.,1.,1.,1.,1.,1.,1.,1.,1.,1.,1.,1.,1.,1.,1.,
1.,1.,1.,1.,1.,1.))
REPRESENTATION_ITEM('')
);
#351=(
BOUNDED_CURVE()
B_SPLINE_CURVE(5,(#58035,#58036,#58037,#58038,#58039,#58040,#58041,#58042,
#58043,#58044,#58045,#58046,#58047,#58048,#58049,#58050,#58051,#58052,#58053,
#58054,#58055,#58056,#58057,#58058,#58059,#58060,#58061,#58062,#58063,#58064,
#58065,#58066,#58067,#58068,#58069,#58070,#58071,#58072,#58073,#58074,#58075,
#58076,#58077,#58078,#58079,#58080,#58081,#58082,#58083,#58084,#58085,#58086,
#58087,#58088,#58089,#58090,#58091,#58092,#58093,#58094,#58095,#58096,#58097,
#58098,#58099,#58100,#58101,#58102,#58103,#58104),.UNSPECIFIED.,.F.,.F.)
B_SPLINE_CURVE_WITH_KNOTS((6,1,1,1,1,1,1,1,1,1,1,1,1,1,1,1,1,1,1,1,1,1,
1,1,1,1,1,1,1,1,1,1,1,1,1,1,1,1,1,1,1,1,1,1,1,1,1,1,1,1,1,1,1,1,1,1,1,1,
1,1,1,1,1,1,1,6),(-1.,-0.984615384615383,-0.969230769230768,-0.953846153846152,
-0.938461538461537,-0.923076923076922,-0.907692307692306,-0.892307692307691,
-0.876923076923076,-0.86153846153846,-0.846153846153845,-0.83076923076923,
-0.815384615384614,-0.799999999999999,-0.784615384615384,-0.769230769230768,
-0.753846153846153,-0.738461538461538,-0.723076923076922,-0.707692307692307,
-0.692307692307692,-0.676923076923076,-0.661538461538461,-0.646153846153846,
-0.63076923076923,-0.615384615384615,-0.6,-0.584615384615384,-0.569230769230769,
-0.553846153846154,-0.538461538461538,-0.523076923076923,-0.507692307692308,
-0.492307692307692,-0.476923076923077,-0.461538461538462,-0.446153846153846,
-0.430769230769231,-0.415384615384615,-0.4,-0.384615384615385,-0.369230769230769,
-0.353846153846154,-0.338461538461538,-0.323076923076923,-0.307692307692308,
-0.292307692307692,-0.276923076923077,-0.261538461538462,-0.246153846153846,
-0.230769230769231,-0.215384615384615,-0.2,-0.184615384615385,-0.169230769230769,
-0.153846153846154,-0.138461538461538,-0.123076923076923,-0.107692307692308,
-0.0923076923076923,-0.0769230769230769,-0.0615384615384615,-0.0461538461538462,
-0.0307692307692308,-0.0153846153846154,-0.0057718433745009),
 .UNSPECIFIED.)
CURVE()
GEOMETRIC_REPRESENTATION_ITEM()
RATIONAL_B_SPLINE_CURVE((1.,1.,1.,1.,1.,1.,1.,1.,1.,1.,1.,1.,1.,1.,1.,1.,
1.,1.,1.,1.,1.,1.,1.,1.,1.,1.,1.,1.,1.,1.,1.,1.,1.,1.,1.,1.,1.,1.,1.,1.,
1.,1.,1.,1.,1.,1.,1.,1.,1.,1.,1.,1.,1.,1.,1.,1.,1.,1.,1.,1.,1.,1.,1.,1.,
1.,1.,1.,1.,1.,1.))
REPRESENTATION_ITEM('')
);
#352=(
BOUNDED_CURVE()
B_SPLINE_CURVE(5,(#58255,#58256,#58257,#58258,#58259,#58260,#58261,#58262,
#58263,#58264,#58265,#58266,#58267,#58268,#58269,#58270,#58271,#58272,#58273,
#58274,#58275,#58276,#58277,#58278,#58279,#58280,#58281,#58282,#58283,#58284,
#58285,#58286,#58287,#58288,#58289,#58290,#58291,#58292,#58293,#58294,#58295,
#58296,#58297,#58298,#58299,#58300,#58301,#58302,#58303,#58304,#58305,#58306,
#58307,#58308,#58309,#58310,#58311,#58312,#58313,#58314,#58315,#58316,#58317,
#58318,#58319,#58320,#58321,#58322,#58323,#58324),.UNSPECIFIED.,.F.,.F.)
B_SPLINE_CURVE_WITH_KNOTS((6,1,1,1,1,1,1,1,1,1,1,1,1,1,1,1,1,1,1,1,1,1,
1,1,1,1,1,1,1,1,1,1,1,1,1,1,1,1,1,1,1,1,1,1,1,1,1,1,1,1,1,1,1,1,1,1,1,1,
1,1,1,1,1,1,1,6),(-0.99422815673967,-0.984615384615383,-0.969230769230768,
-0.953846153846152,-0.938461538461537,-0.923076923076922,-0.907692307692306,
-0.892307692307691,-0.876923076923076,-0.86153846153846,-0.846153846153845,
-0.83076923076923,-0.815384615384614,-0.799999999999999,-0.784615384615384,
-0.769230769230768,-0.753846153846153,-0.738461538461538,-0.723076923076922,
-0.707692307692307,-0.692307692307692,-0.676923076923076,-0.661538461538461,
-0.646153846153846,-0.63076923076923,-0.615384615384615,-0.6,-0.584615384615384,
-0.569230769230769,-0.553846153846154,-0.538461538461538,-0.523076923076923,
-0.507692307692308,-0.492307692307692,-0.476923076923077,-0.461538461538462,
-0.446153846153846,-0.430769230769231,-0.415384615384615,-0.4,-0.384615384615385,
-0.369230769230769,-0.353846153846154,-0.338461538461538,-0.323076923076923,
-0.307692307692308,-0.292307692307692,-0.276923076923077,-0.261538461538462,
-0.246153846153846,-0.230769230769231,-0.215384615384615,-0.2,-0.184615384615385,
-0.169230769230769,-0.153846153846154,-0.138461538461538,-0.123076923076923,
-0.107692307692308,-0.0923076923076923,-0.0769230769230769,-0.0615384615384615,
-0.0461538461538462,-0.0307692307692308,-0.0153846153846154,0.),
 .UNSPECIFIED.)
CURVE()
GEOMETRIC_REPRESENTATION_ITEM()
RATIONAL_B_SPLINE_CURVE((1.,1.,1.,1.,1.,1.,1.,1.,1.,1.,1.,1.,1.,1.,1.,1.,
1.,1.,1.,1.,1.,1.,1.,1.,1.,1.,1.,1.,1.,1.,1.,1.,1.,1.,1.,1.,1.,1.,1.,1.,
1.,1.,1.,1.,1.,1.,1.,1.,1.,1.,1.,1.,1.,1.,1.,1.,1.,1.,1.,1.,1.,1.,1.,1.,
1.,1.,1.,1.,1.,1.))
REPRESENTATION_ITEM('')
);
#353=(
BOUNDED_CURVE()
B_SPLINE_CURVE(5,(#58477,#58478,#58479,#58480,#58481,#58482,#58483,#58484,
#58485,#58486,#58487,#58488,#58489,#58490,#58491,#58492,#58493,#58494,#58495,
#58496,#58497,#58498,#58499,#58500,#58501,#58502,#58503,#58504,#58505,#58506,
#58507,#58508,#58509,#58510,#58511,#58512,#58513,#58514,#58515,#58516,#58517,
#58518,#58519,#58520,#58521,#58522,#58523,#58524,#58525,#58526,#58527,#58528,
#58529,#58530,#58531,#58532,#58533,#58534,#58535,#58536,#58537,#58538,#58539,
#58540,#58541,#58542,#58543,#58544,#58545,#58546),.UNSPECIFIED.,.F.,.F.)
B_SPLINE_CURVE_WITH_KNOTS((6,1,1,1,1,1,1,1,1,1,1,1,1,1,1,1,1,1,1,1,1,1,
1,1,1,1,1,1,1,1,1,1,1,1,1,1,1,1,1,1,1,1,1,1,1,1,1,1,1,1,1,1,1,1,1,1,1,1,
1,1,1,1,1,1,1,6),(-1.,-0.984615384615383,-0.969230769230768,-0.953846153846152,
-0.938461538461537,-0.923076923076922,-0.907692307692306,-0.892307692307691,
-0.876923076923076,-0.86153846153846,-0.846153846153845,-0.83076923076923,
-0.815384615384614,-0.799999999999999,-0.784615384615384,-0.769230769230768,
-0.753846153846153,-0.738461538461538,-0.723076923076922,-0.707692307692307,
-0.692307692307692,-0.676923076923076,-0.661538461538461,-0.646153846153846,
-0.63076923076923,-0.615384615384615,-0.6,-0.584615384615384,-0.569230769230769,
-0.553846153846154,-0.538461538461538,-0.523076923076923,-0.507692307692308,
-0.492307692307692,-0.476923076923077,-0.461538461538462,-0.446153846153846,
-0.430769230769231,-0.415384615384615,-0.4,-0.384615384615385,-0.369230769230769,
-0.353846153846154,-0.338461538461538,-0.323076923076923,-0.307692307692308,
-0.292307692307692,-0.276923076923077,-0.261538461538462,-0.246153846153846,
-0.230769230769231,-0.215384615384615,-0.2,-0.184615384615385,-0.169230769230769,
-0.153846153846154,-0.138461538461538,-0.123076923076923,-0.107692307692308,
-0.0923076923076923,-0.0769230769230769,-0.0615384615384615,-0.0461538461538462,
-0.0307692307692308,-0.0153846153846154,-0.00577184337450701),
 .UNSPECIFIED.)
CURVE()
GEOMETRIC_REPRESENTATION_ITEM()
RATIONAL_B_SPLINE_CURVE((1.,1.,1.,1.,1.,1.,1.,1.,1.,1.,1.,1.,1.,1.,1.,1.,
1.,1.,1.,1.,1.,1.,1.,1.,1.,1.,1.,1.,1.,1.,1.,1.,1.,1.,1.,1.,1.,1.,1.,1.,
1.,1.,1.,1.,1.,1.,1.,1.,1.,1.,1.,1.,1.,1.,1.,1.,1.,1.,1.,1.,1.,1.,1.,1.,
1.,1.,1.,1.,1.,1.))
REPRESENTATION_ITEM('')
);
#354=(
BOUNDED_CURVE()
B_SPLINE_CURVE(5,(#58697,#58698,#58699,#58700,#58701,#58702,#58703,#58704,
#58705,#58706,#58707,#58708,#58709,#58710,#58711,#58712,#58713,#58714,#58715,
#58716,#58717,#58718,#58719,#58720,#58721,#58722,#58723,#58724,#58725,#58726,
#58727,#58728,#58729,#58730,#58731,#58732,#58733,#58734,#58735,#58736,#58737,
#58738,#58739,#58740,#58741,#58742,#58743,#58744,#58745,#58746,#58747,#58748,
#58749,#58750,#58751,#58752,#58753,#58754,#58755,#58756,#58757,#58758,#58759,
#58760,#58761,#58762,#58763,#58764,#58765,#58766),.UNSPECIFIED.,.F.,.F.)
B_SPLINE_CURVE_WITH_KNOTS((6,1,1,1,1,1,1,1,1,1,1,1,1,1,1,1,1,1,1,1,1,1,
1,1,1,1,1,1,1,1,1,1,1,1,1,1,1,1,1,1,1,1,1,1,1,1,1,1,1,1,1,1,1,1,1,1,1,1,
1,1,1,1,1,1,1,6),(-0.994228156739689,-0.984615384615383,-0.969230769230768,
-0.953846153846152,-0.938461538461537,-0.923076923076922,-0.907692307692306,
-0.892307692307691,-0.876923076923076,-0.86153846153846,-0.846153846153845,
-0.83076923076923,-0.815384615384614,-0.799999999999999,-0.784615384615384,
-0.769230769230768,-0.753846153846153,-0.738461538461538,-0.723076923076922,
-0.707692307692307,-0.692307692307692,-0.676923076923076,-0.661538461538461,
-0.646153846153846,-0.63076923076923,-0.615384615384615,-0.6,-0.584615384615384,
-0.569230769230769,-0.553846153846154,-0.538461538461538,-0.523076923076923,
-0.507692307692308,-0.492307692307692,-0.476923076923077,-0.461538461538462,
-0.446153846153846,-0.430769230769231,-0.415384615384615,-0.4,-0.384615384615385,
-0.369230769230769,-0.353846153846154,-0.338461538461538,-0.323076923076923,
-0.307692307692308,-0.292307692307692,-0.276923076923077,-0.261538461538462,
-0.246153846153846,-0.230769230769231,-0.215384615384615,-0.2,-0.184615384615385,
-0.169230769230769,-0.153846153846154,-0.138461538461538,-0.123076923076923,
-0.107692307692308,-0.0923076923076923,-0.0769230769230769,-0.0615384615384615,
-0.0461538461538462,-0.0307692307692308,-0.0153846153846154,0.),
 .UNSPECIFIED.)
CURVE()
GEOMETRIC_REPRESENTATION_ITEM()
RATIONAL_B_SPLINE_CURVE((1.,1.,1.,1.,1.,1.,1.,1.,1.,1.,1.,1.,1.,1.,1.,1.,
1.,1.,1.,1.,1.,1.,1.,1.,1.,1.,1.,1.,1.,1.,1.,1.,1.,1.,1.,1.,1.,1.,1.,1.,
1.,1.,1.,1.,1.,1.,1.,1.,1.,1.,1.,1.,1.,1.,1.,1.,1.,1.,1.,1.,1.,1.,1.,1.,
1.,1.,1.,1.,1.,1.))
REPRESENTATION_ITEM('')
);
#355=(
BOUNDED_CURVE()
B_SPLINE_CURVE(5,(#58919,#58920,#58921,#58922,#58923,#58924,#58925,#58926,
#58927,#58928,#58929,#58930,#58931,#58932,#58933,#58934,#58935,#58936,#58937,
#58938,#58939,#58940,#58941,#58942,#58943,#58944,#58945,#58946,#58947,#58948,
#58949,#58950,#58951,#58952,#58953,#58954,#58955,#58956,#58957,#58958,#58959,
#58960,#58961,#58962,#58963,#58964,#58965,#58966,#58967,#58968,#58969,#58970,
#58971,#58972,#58973,#58974,#58975,#58976,#58977,#58978,#58979,#58980,#58981,
#58982,#58983,#58984,#58985,#58986,#58987,#58988),.UNSPECIFIED.,.F.,.F.)
B_SPLINE_CURVE_WITH_KNOTS((6,1,1,1,1,1,1,1,1,1,1,1,1,1,1,1,1,1,1,1,1,1,
1,1,1,1,1,1,1,1,1,1,1,1,1,1,1,1,1,1,1,1,1,1,1,1,1,1,1,1,1,1,1,1,1,1,1,1,
1,1,1,1,1,1,1,6),(-1.,-0.984615384615383,-0.969230769230768,-0.953846153846152,
-0.938461538461537,-0.923076923076922,-0.907692307692306,-0.892307692307691,
-0.876923076923076,-0.86153846153846,-0.846153846153845,-0.83076923076923,
-0.815384615384614,-0.799999999999999,-0.784615384615384,-0.769230769230768,
-0.753846153846153,-0.738461538461538,-0.723076923076922,-0.707692307692307,
-0.692307692307692,-0.676923076923076,-0.661538461538461,-0.646153846153846,
-0.63076923076923,-0.615384615384615,-0.6,-0.584615384615384,-0.569230769230769,
-0.553846153846154,-0.538461538461538,-0.523076923076923,-0.507692307692308,
-0.492307692307692,-0.476923076923077,-0.461538461538462,-0.446153846153846,
-0.430769230769231,-0.415384615384615,-0.4,-0.384615384615385,-0.369230769230769,
-0.353846153846154,-0.338461538461538,-0.323076923076923,-0.307692307692308,
-0.292307692307692,-0.276923076923077,-0.261538461538462,-0.246153846153846,
-0.230769230769231,-0.215384615384615,-0.2,-0.184615384615385,-0.169230769230769,
-0.153846153846154,-0.138461538461538,-0.123076923076923,-0.107692307692308,
-0.0923076923076923,-0.0769230769230769,-0.0615384615384615,-0.0461538461538462,
-0.0307692307692308,-0.0153846153846154,-0.00577184337452382),
 .UNSPECIFIED.)
CURVE()
GEOMETRIC_REPRESENTATION_ITEM()
RATIONAL_B_SPLINE_CURVE((1.,1.,1.,1.,1.,1.,1.,1.,1.,1.,1.,1.,1.,1.,1.,1.,
1.,1.,1.,1.,1.,1.,1.,1.,1.,1.,1.,1.,1.,1.,1.,1.,1.,1.,1.,1.,1.,1.,1.,1.,
1.,1.,1.,1.,1.,1.,1.,1.,1.,1.,1.,1.,1.,1.,1.,1.,1.,1.,1.,1.,1.,1.,1.,1.,
1.,1.,1.,1.,1.,1.))
REPRESENTATION_ITEM('')
);
#356=(
BOUNDED_CURVE()
B_SPLINE_CURVE(5,(#59139,#59140,#59141,#59142,#59143,#59144,#59145,#59146,
#59147,#59148,#59149,#59150,#59151,#59152,#59153,#59154,#59155,#59156,#59157,
#59158,#59159,#59160,#59161,#59162,#59163,#59164,#59165,#59166,#59167,#59168,
#59169,#59170,#59171,#59172,#59173,#59174,#59175,#59176,#59177,#59178,#59179,
#59180,#59181,#59182,#59183,#59184,#59185,#59186,#59187,#59188,#59189,#59190,
#59191,#59192,#59193,#59194,#59195,#59196,#59197,#59198,#59199,#59200,#59201,
#59202,#59203,#59204,#59205,#59206,#59207,#59208),.UNSPECIFIED.,.F.,.F.)
B_SPLINE_CURVE_WITH_KNOTS((6,1,1,1,1,1,1,1,1,1,1,1,1,1,1,1,1,1,1,1,1,1,
1,1,1,1,1,1,1,1,1,1,1,1,1,1,1,1,1,1,1,1,1,1,1,1,1,1,1,1,1,1,1,1,1,1,1,1,
1,1,1,1,1,1,1,6),(-0.994228156739677,-0.984615384615383,-0.969230769230768,
-0.953846153846152,-0.938461538461537,-0.923076923076922,-0.907692307692306,
-0.892307692307691,-0.876923076923076,-0.86153846153846,-0.846153846153845,
-0.83076923076923,-0.815384615384614,-0.799999999999999,-0.784615384615384,
-0.769230769230768,-0.753846153846153,-0.738461538461538,-0.723076923076922,
-0.707692307692307,-0.692307692307692,-0.676923076923076,-0.661538461538461,
-0.646153846153846,-0.63076923076923,-0.615384615384615,-0.6,-0.584615384615384,
-0.569230769230769,-0.553846153846154,-0.538461538461538,-0.523076923076923,
-0.507692307692308,-0.492307692307692,-0.476923076923077,-0.461538461538462,
-0.446153846153846,-0.430769230769231,-0.415384615384615,-0.4,-0.384615384615385,
-0.369230769230769,-0.353846153846154,-0.338461538461538,-0.323076923076923,
-0.307692307692308,-0.292307692307692,-0.276923076923077,-0.261538461538462,
-0.246153846153846,-0.230769230769231,-0.215384615384615,-0.2,-0.184615384615385,
-0.169230769230769,-0.153846153846154,-0.138461538461538,-0.123076923076923,
-0.107692307692308,-0.0923076923076923,-0.0769230769230769,-0.0615384615384615,
-0.0461538461538462,-0.0307692307692308,-0.0153846153846154,0.),
 .UNSPECIFIED.)
CURVE()
GEOMETRIC_REPRESENTATION_ITEM()
RATIONAL_B_SPLINE_CURVE((1.,1.,1.,1.,1.,1.,1.,1.,1.,1.,1.,1.,1.,1.,1.,1.,
1.,1.,1.,1.,1.,1.,1.,1.,1.,1.,1.,1.,1.,1.,1.,1.,1.,1.,1.,1.,1.,1.,1.,1.,
1.,1.,1.,1.,1.,1.,1.,1.,1.,1.,1.,1.,1.,1.,1.,1.,1.,1.,1.,1.,1.,1.,1.,1.,
1.,1.,1.,1.,1.,1.))
REPRESENTATION_ITEM('')
);
#357=(
BOUNDED_CURVE()
B_SPLINE_CURVE(5,(#59361,#59362,#59363,#59364,#59365,#59366,#59367,#59368,
#59369,#59370,#59371,#59372,#59373,#59374,#59375,#59376,#59377,#59378,#59379,
#59380,#59381,#59382,#59383,#59384,#59385,#59386,#59387,#59388,#59389,#59390,
#59391,#59392,#59393,#59394,#59395,#59396,#59397,#59398,#59399,#59400,#59401,
#59402,#59403,#59404,#59405,#59406,#59407,#59408,#59409,#59410,#59411,#59412,
#59413,#59414,#59415,#59416,#59417,#59418,#59419,#59420,#59421,#59422,#59423,
#59424,#59425,#59426,#59427,#59428,#59429,#59430),.UNSPECIFIED.,.F.,.F.)
B_SPLINE_CURVE_WITH_KNOTS((6,1,1,1,1,1,1,1,1,1,1,1,1,1,1,1,1,1,1,1,1,1,
1,1,1,1,1,1,1,1,1,1,1,1,1,1,1,1,1,1,1,1,1,1,1,1,1,1,1,1,1,1,1,1,1,1,1,1,
1,1,1,1,1,1,1,6),(-1.,-0.984615384615383,-0.969230769230768,-0.953846153846152,
-0.938461538461537,-0.923076923076922,-0.907692307692306,-0.892307692307691,
-0.876923076923076,-0.86153846153846,-0.846153846153845,-0.83076923076923,
-0.815384615384614,-0.799999999999999,-0.784615384615384,-0.769230769230768,
-0.753846153846153,-0.738461538461538,-0.723076923076922,-0.707692307692307,
-0.692307692307692,-0.676923076923076,-0.661538461538461,-0.646153846153846,
-0.63076923076923,-0.615384615384615,-0.6,-0.584615384615384,-0.569230769230769,
-0.553846153846154,-0.538461538461538,-0.523076923076923,-0.507692307692308,
-0.492307692307692,-0.476923076923077,-0.461538461538462,-0.446153846153846,
-0.430769230769231,-0.415384615384615,-0.4,-0.384615384615385,-0.369230769230769,
-0.353846153846154,-0.338461538461538,-0.323076923076923,-0.307692307692308,
-0.292307692307692,-0.276923076923077,-0.261538461538462,-0.246153846153846,
-0.230769230769231,-0.215384615384615,-0.2,-0.184615384615385,-0.169230769230769,
-0.153846153846154,-0.138461538461538,-0.123076923076923,-0.107692307692308,
-0.0923076923076923,-0.0769230769230769,-0.0615384615384615,-0.0461538461538462,
-0.0307692307692308,-0.0153846153846154,-0.0057718433744938),
 .UNSPECIFIED.)
CURVE()
GEOMETRIC_REPRESENTATION_ITEM()
RATIONAL_B_SPLINE_CURVE((1.,1.,1.,1.,1.,1.,1.,1.,1.,1.,1.,1.,1.,1.,1.,1.,
1.,1.,1.,1.,1.,1.,1.,1.,1.,1.,1.,1.,1.,1.,1.,1.,1.,1.,1.,1.,1.,1.,1.,1.,
1.,1.,1.,1.,1.,1.,1.,1.,1.,1.,1.,1.,1.,1.,1.,1.,1.,1.,1.,1.,1.,1.,1.,1.,
1.,1.,1.,1.,1.,1.))
REPRESENTATION_ITEM('')
);
#358=(
BOUNDED_CURVE()
B_SPLINE_CURVE(5,(#59581,#59582,#59583,#59584,#59585,#59586,#59587,#59588,
#59589,#59590,#59591,#59592,#59593,#59594,#59595,#59596,#59597,#59598,#59599,
#59600,#59601,#59602,#59603,#59604,#59605,#59606,#59607,#59608,#59609,#59610,
#59611,#59612,#59613,#59614,#59615,#59616,#59617,#59618,#59619,#59620,#59621,
#59622,#59623,#59624,#59625,#59626,#59627,#59628,#59629,#59630,#59631,#59632,
#59633,#59634,#59635,#59636,#59637,#59638,#59639,#59640,#59641,#59642,#59643,
#59644,#59645,#59646,#59647,#59648,#59649,#59650),.UNSPECIFIED.,.F.,.F.)
B_SPLINE_CURVE_WITH_KNOTS((6,1,1,1,1,1,1,1,1,1,1,1,1,1,1,1,1,1,1,1,1,1,
1,1,1,1,1,1,1,1,1,1,1,1,1,1,1,1,1,1,1,1,1,1,1,1,1,1,1,1,1,1,1,1,1,1,1,1,
1,1,1,1,1,1,1,6),(-0.994228156739743,-0.984615384615383,-0.969230769230768,
-0.953846153846152,-0.938461538461537,-0.923076923076922,-0.907692307692306,
-0.892307692307691,-0.876923076923076,-0.86153846153846,-0.846153846153845,
-0.83076923076923,-0.815384615384614,-0.799999999999999,-0.784615384615384,
-0.769230769230768,-0.753846153846153,-0.738461538461538,-0.723076923076922,
-0.707692307692307,-0.692307692307692,-0.676923076923076,-0.661538461538461,
-0.646153846153846,-0.63076923076923,-0.615384615384615,-0.6,-0.584615384615384,
-0.569230769230769,-0.553846153846154,-0.538461538461538,-0.523076923076923,
-0.507692307692308,-0.492307692307692,-0.476923076923077,-0.461538461538462,
-0.446153846153846,-0.430769230769231,-0.415384615384615,-0.4,-0.384615384615385,
-0.369230769230769,-0.353846153846154,-0.338461538461538,-0.323076923076923,
-0.307692307692308,-0.292307692307692,-0.276923076923077,-0.261538461538462,
-0.246153846153846,-0.230769230769231,-0.215384615384615,-0.2,-0.184615384615385,
-0.169230769230769,-0.153846153846154,-0.138461538461538,-0.123076923076923,
-0.107692307692308,-0.0923076923076923,-0.0769230769230769,-0.0615384615384615,
-0.0461538461538462,-0.0307692307692308,-0.0153846153846154,0.),
 .UNSPECIFIED.)
CURVE()
GEOMETRIC_REPRESENTATION_ITEM()
RATIONAL_B_SPLINE_CURVE((1.,1.,1.,1.,1.,1.,1.,1.,1.,1.,1.,1.,1.,1.,1.,1.,
1.,1.,1.,1.,1.,1.,1.,1.,1.,1.,1.,1.,1.,1.,1.,1.,1.,1.,1.,1.,1.,1.,1.,1.,
1.,1.,1.,1.,1.,1.,1.,1.,1.,1.,1.,1.,1.,1.,1.,1.,1.,1.,1.,1.,1.,1.,1.,1.,
1.,1.,1.,1.,1.,1.))
REPRESENTATION_ITEM('')
);
#359=(
BOUNDED_CURVE()
B_SPLINE_CURVE(5,(#59803,#59804,#59805,#59806,#59807,#59808,#59809,#59810,
#59811,#59812,#59813,#59814,#59815,#59816,#59817,#59818,#59819,#59820,#59821,
#59822,#59823,#59824,#59825,#59826,#59827,#59828,#59829,#59830,#59831,#59832,
#59833,#59834,#59835,#59836,#59837,#59838,#59839,#59840,#59841,#59842,#59843,
#59844,#59845,#59846,#59847,#59848,#59849,#59850,#59851,#59852,#59853,#59854,
#59855,#59856,#59857,#59858,#59859,#59860,#59861,#59862,#59863,#59864,#59865,
#59866,#59867,#59868,#59869,#59870,#59871,#59872),.UNSPECIFIED.,.F.,.F.)
B_SPLINE_CURVE_WITH_KNOTS((6,1,1,1,1,1,1,1,1,1,1,1,1,1,1,1,1,1,1,1,1,1,
1,1,1,1,1,1,1,1,1,1,1,1,1,1,1,1,1,1,1,1,1,1,1,1,1,1,1,1,1,1,1,1,1,1,1,1,
1,1,1,1,1,1,1,6),(-1.,-0.984615384615383,-0.969230769230768,-0.953846153846152,
-0.938461538461537,-0.923076923076922,-0.907692307692306,-0.892307692307691,
-0.876923076923076,-0.86153846153846,-0.846153846153845,-0.83076923076923,
-0.815384615384614,-0.799999999999999,-0.784615384615384,-0.769230769230768,
-0.753846153846153,-0.738461538461538,-0.723076923076922,-0.707692307692307,
-0.692307692307692,-0.676923076923076,-0.661538461538461,-0.646153846153846,
-0.63076923076923,-0.615384615384615,-0.6,-0.584615384615384,-0.569230769230769,
-0.553846153846154,-0.538461538461538,-0.523076923076923,-0.507692307692308,
-0.492307692307692,-0.476923076923077,-0.461538461538462,-0.446153846153846,
-0.430769230769231,-0.415384615384615,-0.4,-0.384615384615385,-0.369230769230769,
-0.353846153846154,-0.338461538461538,-0.323076923076923,-0.307692307692308,
-0.292307692307692,-0.276923076923077,-0.261538461538462,-0.246153846153846,
-0.230769230769231,-0.215384615384615,-0.2,-0.184615384615385,-0.169230769230769,
-0.153846153846154,-0.138461538461538,-0.123076923076923,-0.107692307692308,
-0.0923076923076923,-0.0769230769230769,-0.0615384615384615,-0.0461538461538462,
-0.0307692307692308,-0.0153846153846154,-0.0057718433745291),
 .UNSPECIFIED.)
CURVE()
GEOMETRIC_REPRESENTATION_ITEM()
RATIONAL_B_SPLINE_CURVE((1.,1.,1.,1.,1.,1.,1.,1.,1.,1.,1.,1.,1.,1.,1.,1.,
1.,1.,1.,1.,1.,1.,1.,1.,1.,1.,1.,1.,1.,1.,1.,1.,1.,1.,1.,1.,1.,1.,1.,1.,
1.,1.,1.,1.,1.,1.,1.,1.,1.,1.,1.,1.,1.,1.,1.,1.,1.,1.,1.,1.,1.,1.,1.,1.,
1.,1.,1.,1.,1.,1.))
REPRESENTATION_ITEM('')
);
#360=(
BOUNDED_CURVE()
B_SPLINE_CURVE(5,(#60023,#60024,#60025,#60026,#60027,#60028,#60029,#60030,
#60031,#60032,#60033,#60034,#60035,#60036,#60037,#60038,#60039,#60040,#60041,
#60042,#60043,#60044,#60045,#60046,#60047,#60048,#60049,#60050,#60051,#60052,
#60053,#60054,#60055,#60056,#60057,#60058,#60059,#60060,#60061,#60062,#60063,
#60064,#60065,#60066,#60067,#60068,#60069,#60070,#60071,#60072,#60073,#60074,
#60075,#60076,#60077,#60078,#60079,#60080,#60081,#60082,#60083,#60084,#60085,
#60086,#60087,#60088,#60089,#60090,#60091,#60092),.UNSPECIFIED.,.F.,.F.)
B_SPLINE_CURVE_WITH_KNOTS((6,1,1,1,1,1,1,1,1,1,1,1,1,1,1,1,1,1,1,1,1,1,
1,1,1,1,1,1,1,1,1,1,1,1,1,1,1,1,1,1,1,1,1,1,1,1,1,1,1,1,1,1,1,1,1,1,1,1,
1,1,1,1,1,1,1,6),(-0.994228156739665,-0.984615384615383,-0.969230769230768,
-0.953846153846152,-0.938461538461537,-0.923076923076922,-0.907692307692306,
-0.892307692307691,-0.876923076923076,-0.86153846153846,-0.846153846153845,
-0.83076923076923,-0.815384615384614,-0.799999999999999,-0.784615384615384,
-0.769230769230768,-0.753846153846153,-0.738461538461538,-0.723076923076922,
-0.707692307692307,-0.692307692307692,-0.676923076923076,-0.661538461538461,
-0.646153846153846,-0.63076923076923,-0.615384615384615,-0.6,-0.584615384615384,
-0.569230769230769,-0.553846153846154,-0.538461538461538,-0.523076923076923,
-0.507692307692308,-0.492307692307692,-0.476923076923077,-0.461538461538462,
-0.446153846153846,-0.430769230769231,-0.415384615384615,-0.4,-0.384615384615385,
-0.369230769230769,-0.353846153846154,-0.338461538461538,-0.323076923076923,
-0.307692307692308,-0.292307692307692,-0.276923076923077,-0.261538461538462,
-0.246153846153846,-0.230769230769231,-0.215384615384615,-0.2,-0.184615384615385,
-0.169230769230769,-0.153846153846154,-0.138461538461538,-0.123076923076923,
-0.107692307692308,-0.0923076923076923,-0.0769230769230769,-0.0615384615384615,
-0.0461538461538462,-0.0307692307692308,-0.0153846153846154,0.),
 .UNSPECIFIED.)
CURVE()
GEOMETRIC_REPRESENTATION_ITEM()
RATIONAL_B_SPLINE_CURVE((1.,1.,1.,1.,1.,1.,1.,1.,1.,1.,1.,1.,1.,1.,1.,1.,
1.,1.,1.,1.,1.,1.,1.,1.,1.,1.,1.,1.,1.,1.,1.,1.,1.,1.,1.,1.,1.,1.,1.,1.,
1.,1.,1.,1.,1.,1.,1.,1.,1.,1.,1.,1.,1.,1.,1.,1.,1.,1.,1.,1.,1.,1.,1.,1.,
1.,1.,1.,1.,1.,1.))
REPRESENTATION_ITEM('')
);
#361=(
BOUNDED_CURVE()
B_SPLINE_CURVE(5,(#60245,#60246,#60247,#60248,#60249,#60250,#60251,#60252,
#60253,#60254,#60255,#60256,#60257,#60258,#60259,#60260,#60261,#60262,#60263,
#60264,#60265,#60266,#60267,#60268,#60269,#60270,#60271,#60272,#60273,#60274,
#60275,#60276,#60277,#60278,#60279,#60280,#60281,#60282,#60283,#60284,#60285,
#60286,#60287,#60288,#60289,#60290,#60291,#60292,#60293,#60294,#60295,#60296,
#60297,#60298,#60299,#60300,#60301,#60302,#60303,#60304,#60305,#60306,#60307,
#60308,#60309,#60310,#60311,#60312,#60313,#60314),.UNSPECIFIED.,.F.,.F.)
B_SPLINE_CURVE_WITH_KNOTS((6,1,1,1,1,1,1,1,1,1,1,1,1,1,1,1,1,1,1,1,1,1,
1,1,1,1,1,1,1,1,1,1,1,1,1,1,1,1,1,1,1,1,1,1,1,1,1,1,1,1,1,1,1,1,1,1,1,1,
1,1,1,1,1,1,1,6),(-1.,-0.984615384615383,-0.969230769230768,-0.953846153846152,
-0.938461538461537,-0.923076923076922,-0.907692307692306,-0.892307692307691,
-0.876923076923076,-0.86153846153846,-0.846153846153845,-0.83076923076923,
-0.815384615384614,-0.799999999999999,-0.784615384615384,-0.769230769230768,
-0.753846153846153,-0.738461538461538,-0.723076923076922,-0.707692307692307,
-0.692307692307692,-0.676923076923076,-0.661538461538461,-0.646153846153846,
-0.63076923076923,-0.615384615384615,-0.6,-0.584615384615384,-0.569230769230769,
-0.553846153846154,-0.538461538461538,-0.523076923076923,-0.507692307692308,
-0.492307692307692,-0.476923076923077,-0.461538461538462,-0.446153846153846,
-0.430769230769231,-0.415384615384615,-0.4,-0.384615384615385,-0.369230769230769,
-0.353846153846154,-0.338461538461538,-0.323076923076923,-0.307692307692308,
-0.292307692307692,-0.276923076923077,-0.261538461538462,-0.246153846153846,
-0.230769230769231,-0.215384615384615,-0.2,-0.184615384615385,-0.169230769230769,
-0.153846153846154,-0.138461538461538,-0.123076923076923,-0.107692307692308,
-0.0923076923076923,-0.0769230769230769,-0.0615384615384615,-0.0461538461538462,
-0.0307692307692308,-0.0153846153846154,-0.00577184337450666),
 .UNSPECIFIED.)
CURVE()
GEOMETRIC_REPRESENTATION_ITEM()
RATIONAL_B_SPLINE_CURVE((1.,1.,1.,1.,1.,1.,1.,1.,1.,1.,1.,1.,1.,1.,1.,1.,
1.,1.,1.,1.,1.,1.,1.,1.,1.,1.,1.,1.,1.,1.,1.,1.,1.,1.,1.,1.,1.,1.,1.,1.,
1.,1.,1.,1.,1.,1.,1.,1.,1.,1.,1.,1.,1.,1.,1.,1.,1.,1.,1.,1.,1.,1.,1.,1.,
1.,1.,1.,1.,1.,1.))
REPRESENTATION_ITEM('')
);
#362=(
BOUNDED_CURVE()
B_SPLINE_CURVE(5,(#60465,#60466,#60467,#60468,#60469,#60470,#60471,#60472,
#60473,#60474,#60475,#60476,#60477,#60478,#60479,#60480,#60481,#60482,#60483,
#60484,#60485,#60486,#60487,#60488,#60489,#60490,#60491,#60492,#60493,#60494,
#60495,#60496,#60497,#60498,#60499,#60500,#60501,#60502,#60503,#60504,#60505,
#60506,#60507,#60508,#60509,#60510,#60511,#60512,#60513,#60514,#60515,#60516,
#60517,#60518,#60519,#60520,#60521,#60522,#60523,#60524,#60525,#60526,#60527,
#60528,#60529,#60530,#60531,#60532,#60533,#60534),.UNSPECIFIED.,.F.,.F.)
B_SPLINE_CURVE_WITH_KNOTS((6,1,1,1,1,1,1,1,1,1,1,1,1,1,1,1,1,1,1,1,1,1,
1,1,1,1,1,1,1,1,1,1,1,1,1,1,1,1,1,1,1,1,1,1,1,1,1,1,1,1,1,1,1,1,1,1,1,1,
1,1,1,1,1,1,1,6),(-0.994228156739758,-0.984615384615383,-0.969230769230768,
-0.953846153846152,-0.938461538461537,-0.923076923076922,-0.907692307692306,
-0.892307692307691,-0.876923076923076,-0.86153846153846,-0.846153846153845,
-0.83076923076923,-0.815384615384614,-0.799999999999999,-0.784615384615384,
-0.769230769230768,-0.753846153846153,-0.738461538461538,-0.723076923076922,
-0.707692307692307,-0.692307692307692,-0.676923076923076,-0.661538461538461,
-0.646153846153846,-0.63076923076923,-0.615384615384615,-0.6,-0.584615384615384,
-0.569230769230769,-0.553846153846154,-0.538461538461538,-0.523076923076923,
-0.507692307692308,-0.492307692307692,-0.476923076923077,-0.461538461538462,
-0.446153846153846,-0.430769230769231,-0.415384615384615,-0.4,-0.384615384615385,
-0.369230769230769,-0.353846153846154,-0.338461538461538,-0.323076923076923,
-0.307692307692308,-0.292307692307692,-0.276923076923077,-0.261538461538462,
-0.246153846153846,-0.230769230769231,-0.215384615384615,-0.2,-0.184615384615385,
-0.169230769230769,-0.153846153846154,-0.138461538461538,-0.123076923076923,
-0.107692307692308,-0.0923076923076923,-0.0769230769230769,-0.0615384615384615,
-0.0461538461538462,-0.0307692307692308,-0.0153846153846154,0.),
 .UNSPECIFIED.)
CURVE()
GEOMETRIC_REPRESENTATION_ITEM()
RATIONAL_B_SPLINE_CURVE((1.,1.,1.,1.,1.,1.,1.,1.,1.,1.,1.,1.,1.,1.,1.,1.,
1.,1.,1.,1.,1.,1.,1.,1.,1.,1.,1.,1.,1.,1.,1.,1.,1.,1.,1.,1.,1.,1.,1.,1.,
1.,1.,1.,1.,1.,1.,1.,1.,1.,1.,1.,1.,1.,1.,1.,1.,1.,1.,1.,1.,1.,1.,1.,1.,
1.,1.,1.,1.,1.,1.))
REPRESENTATION_ITEM('')
);
#363=(
BOUNDED_CURVE()
B_SPLINE_CURVE(5,(#60687,#60688,#60689,#60690,#60691,#60692,#60693,#60694,
#60695,#60696,#60697,#60698,#60699,#60700,#60701,#60702,#60703,#60704,#60705,
#60706,#60707,#60708,#60709,#60710,#60711,#60712,#60713,#60714,#60715,#60716,
#60717,#60718,#60719,#60720,#60721,#60722,#60723,#60724,#60725,#60726,#60727,
#60728,#60729,#60730,#60731,#60732,#60733,#60734,#60735,#60736,#60737,#60738,
#60739,#60740,#60741,#60742,#60743,#60744,#60745,#60746,#60747,#60748,#60749,
#60750,#60751,#60752,#60753,#60754,#60755,#60756),.UNSPECIFIED.,.F.,.F.)
B_SPLINE_CURVE_WITH_KNOTS((6,1,1,1,1,1,1,1,1,1,1,1,1,1,1,1,1,1,1,1,1,1,
1,1,1,1,1,1,1,1,1,1,1,1,1,1,1,1,1,1,1,1,1,1,1,1,1,1,1,1,1,1,1,1,1,1,1,1,
1,1,1,1,1,1,1,6),(-1.,-0.984615384615383,-0.969230769230768,-0.953846153846152,
-0.938461538461537,-0.923076923076922,-0.907692307692306,-0.892307692307691,
-0.876923076923076,-0.86153846153846,-0.846153846153845,-0.83076923076923,
-0.815384615384614,-0.799999999999999,-0.784615384615384,-0.769230769230768,
-0.753846153846153,-0.738461538461538,-0.723076923076922,-0.707692307692307,
-0.692307692307692,-0.676923076923076,-0.661538461538461,-0.646153846153846,
-0.63076923076923,-0.615384615384615,-0.6,-0.584615384615384,-0.569230769230769,
-0.553846153846154,-0.538461538461538,-0.523076923076923,-0.507692307692308,
-0.492307692307692,-0.476923076923077,-0.461538461538462,-0.446153846153846,
-0.430769230769231,-0.415384615384615,-0.4,-0.384615384615385,-0.369230769230769,
-0.353846153846154,-0.338461538461538,-0.323076923076923,-0.307692307692308,
-0.292307692307692,-0.276923076923077,-0.261538461538462,-0.246153846153846,
-0.230769230769231,-0.215384615384615,-0.2,-0.184615384615385,-0.169230769230769,
-0.153846153846154,-0.138461538461538,-0.123076923076923,-0.107692307692308,
-0.0923076923076923,-0.0769230769230769,-0.0615384615384615,-0.0461538461538462,
-0.0307692307692308,-0.0153846153846154,-0.00577184337451981),
 .UNSPECIFIED.)
CURVE()
GEOMETRIC_REPRESENTATION_ITEM()
RATIONAL_B_SPLINE_CURVE((1.,1.,1.,1.,1.,1.,1.,1.,1.,1.,1.,1.,1.,1.,1.,1.,
1.,1.,1.,1.,1.,1.,1.,1.,1.,1.,1.,1.,1.,1.,1.,1.,1.,1.,1.,1.,1.,1.,1.,1.,
1.,1.,1.,1.,1.,1.,1.,1.,1.,1.,1.,1.,1.,1.,1.,1.,1.,1.,1.,1.,1.,1.,1.,1.,
1.,1.,1.,1.,1.,1.))
REPRESENTATION_ITEM('')
);
#364=(
BOUNDED_CURVE()
B_SPLINE_CURVE(5,(#60907,#60908,#60909,#60910,#60911,#60912,#60913,#60914,
#60915,#60916,#60917,#60918,#60919,#60920,#60921,#60922,#60923,#60924,#60925,
#60926,#60927,#60928,#60929,#60930,#60931,#60932,#60933,#60934,#60935,#60936,
#60937,#60938,#60939,#60940,#60941,#60942,#60943,#60944,#60945,#60946,#60947,
#60948,#60949,#60950,#60951,#60952,#60953,#60954,#60955,#60956,#60957,#60958,
#60959,#60960,#60961,#60962,#60963,#60964,#60965,#60966,#60967,#60968,#60969,
#60970,#60971,#60972,#60973,#60974,#60975,#60976),.UNSPECIFIED.,.F.,.F.)
B_SPLINE_CURVE_WITH_KNOTS((6,1,1,1,1,1,1,1,1,1,1,1,1,1,1,1,1,1,1,1,1,1,
1,1,1,1,1,1,1,1,1,1,1,1,1,1,1,1,1,1,1,1,1,1,1,1,1,1,1,1,1,1,1,1,1,1,1,1,
1,1,1,1,1,1,1,6),(-0.994228156739659,-0.984615384615383,-0.969230769230768,
-0.953846153846152,-0.938461538461537,-0.923076923076922,-0.907692307692306,
-0.892307692307691,-0.876923076923076,-0.86153846153846,-0.846153846153845,
-0.83076923076923,-0.815384615384614,-0.799999999999999,-0.784615384615384,
-0.769230769230768,-0.753846153846153,-0.738461538461538,-0.723076923076922,
-0.707692307692307,-0.692307692307692,-0.676923076923076,-0.661538461538461,
-0.646153846153846,-0.63076923076923,-0.615384615384615,-0.6,-0.584615384615384,
-0.569230769230769,-0.553846153846154,-0.538461538461538,-0.523076923076923,
-0.507692307692308,-0.492307692307692,-0.476923076923077,-0.461538461538462,
-0.446153846153846,-0.430769230769231,-0.415384615384615,-0.4,-0.384615384615385,
-0.369230769230769,-0.353846153846154,-0.338461538461538,-0.323076923076923,
-0.307692307692308,-0.292307692307692,-0.276923076923077,-0.261538461538462,
-0.246153846153846,-0.230769230769231,-0.215384615384615,-0.2,-0.184615384615385,
-0.169230769230769,-0.153846153846154,-0.138461538461538,-0.123076923076923,
-0.107692307692308,-0.0923076923076923,-0.0769230769230769,-0.0615384615384615,
-0.0461538461538462,-0.0307692307692308,-0.0153846153846154,0.),
 .UNSPECIFIED.)
CURVE()
GEOMETRIC_REPRESENTATION_ITEM()
RATIONAL_B_SPLINE_CURVE((1.,1.,1.,1.,1.,1.,1.,1.,1.,1.,1.,1.,1.,1.,1.,1.,
1.,1.,1.,1.,1.,1.,1.,1.,1.,1.,1.,1.,1.,1.,1.,1.,1.,1.,1.,1.,1.,1.,1.,1.,
1.,1.,1.,1.,1.,1.,1.,1.,1.,1.,1.,1.,1.,1.,1.,1.,1.,1.,1.,1.,1.,1.,1.,1.,
1.,1.,1.,1.,1.,1.))
REPRESENTATION_ITEM('')
);
#365=(
BOUNDED_CURVE()
B_SPLINE_CURVE(5,(#61129,#61130,#61131,#61132,#61133,#61134,#61135,#61136,
#61137,#61138,#61139,#61140,#61141,#61142,#61143,#61144,#61145,#61146,#61147,
#61148,#61149,#61150,#61151,#61152,#61153,#61154,#61155,#61156,#61157,#61158,
#61159,#61160,#61161,#61162,#61163,#61164,#61165,#61166,#61167,#61168,#61169,
#61170,#61171,#61172,#61173,#61174,#61175,#61176,#61177,#61178,#61179,#61180,
#61181,#61182,#61183,#61184,#61185,#61186,#61187,#61188,#61189,#61190,#61191,
#61192,#61193,#61194,#61195,#61196,#61197,#61198),.UNSPECIFIED.,.F.,.F.)
B_SPLINE_CURVE_WITH_KNOTS((6,1,1,1,1,1,1,1,1,1,1,1,1,1,1,1,1,1,1,1,1,1,
1,1,1,1,1,1,1,1,1,1,1,1,1,1,1,1,1,1,1,1,1,1,1,1,1,1,1,1,1,1,1,1,1,1,1,1,
1,1,1,1,1,1,1,6),(-1.,-0.984615384615383,-0.969230769230768,-0.953846153846152,
-0.938461538461537,-0.923076923076922,-0.907692307692306,-0.892307692307691,
-0.876923076923076,-0.86153846153846,-0.846153846153845,-0.83076923076923,
-0.815384615384614,-0.799999999999999,-0.784615384615384,-0.769230769230768,
-0.753846153846153,-0.738461538461538,-0.723076923076922,-0.707692307692307,
-0.692307692307692,-0.676923076923076,-0.661538461538461,-0.646153846153846,
-0.63076923076923,-0.615384615384615,-0.6,-0.584615384615384,-0.569230769230769,
-0.553846153846154,-0.538461538461538,-0.523076923076923,-0.507692307692308,
-0.492307692307692,-0.476923076923077,-0.461538461538462,-0.446153846153846,
-0.430769230769231,-0.415384615384615,-0.4,-0.384615384615385,-0.369230769230769,
-0.353846153846154,-0.338461538461538,-0.323076923076923,-0.307692307692308,
-0.292307692307692,-0.276923076923077,-0.261538461538462,-0.246153846153846,
-0.230769230769231,-0.215384615384615,-0.2,-0.184615384615385,-0.169230769230769,
-0.153846153846154,-0.138461538461538,-0.123076923076923,-0.107692307692308,
-0.0923076923076923,-0.0769230769230769,-0.0615384615384615,-0.0461538461538462,
-0.0307692307692308,-0.0153846153846154,-0.00577184337450306),
 .UNSPECIFIED.)
CURVE()
GEOMETRIC_REPRESENTATION_ITEM()
RATIONAL_B_SPLINE_CURVE((1.,1.,1.,1.,1.,1.,1.,1.,1.,1.,1.,1.,1.,1.,1.,1.,
1.,1.,1.,1.,1.,1.,1.,1.,1.,1.,1.,1.,1.,1.,1.,1.,1.,1.,1.,1.,1.,1.,1.,1.,
1.,1.,1.,1.,1.,1.,1.,1.,1.,1.,1.,1.,1.,1.,1.,1.,1.,1.,1.,1.,1.,1.,1.,1.,
1.,1.,1.,1.,1.,1.))
REPRESENTATION_ITEM('')
);
#366=(
BOUNDED_CURVE()
B_SPLINE_CURVE(5,(#61349,#61350,#61351,#61352,#61353,#61354,#61355,#61356,
#61357,#61358,#61359,#61360,#61361,#61362,#61363,#61364,#61365,#61366,#61367,
#61368,#61369,#61370,#61371,#61372,#61373,#61374,#61375,#61376,#61377,#61378,
#61379,#61380,#61381,#61382,#61383,#61384,#61385,#61386,#61387,#61388,#61389,
#61390,#61391,#61392,#61393,#61394,#61395,#61396,#61397,#61398,#61399,#61400,
#61401,#61402,#61403,#61404,#61405,#61406,#61407,#61408,#61409,#61410,#61411,
#61412,#61413,#61414,#61415,#61416,#61417,#61418),.UNSPECIFIED.,.F.,.F.)
B_SPLINE_CURVE_WITH_KNOTS((6,1,1,1,1,1,1,1,1,1,1,1,1,1,1,1,1,1,1,1,1,1,
1,1,1,1,1,1,1,1,1,1,1,1,1,1,1,1,1,1,1,1,1,1,1,1,1,1,1,1,1,1,1,1,1,1,1,1,
1,1,1,1,1,1,1,6),(-0.994228156739675,-0.984615384615383,-0.969230769230768,
-0.953846153846152,-0.938461538461537,-0.923076923076922,-0.907692307692306,
-0.892307692307691,-0.876923076923076,-0.86153846153846,-0.846153846153845,
-0.83076923076923,-0.815384615384614,-0.799999999999999,-0.784615384615384,
-0.769230769230768,-0.753846153846153,-0.738461538461538,-0.723076923076922,
-0.707692307692307,-0.692307692307692,-0.676923076923076,-0.661538461538461,
-0.646153846153846,-0.63076923076923,-0.615384615384615,-0.6,-0.584615384615384,
-0.569230769230769,-0.553846153846154,-0.538461538461538,-0.523076923076923,
-0.507692307692308,-0.492307692307692,-0.476923076923077,-0.461538461538462,
-0.446153846153846,-0.430769230769231,-0.415384615384615,-0.4,-0.384615384615385,
-0.369230769230769,-0.353846153846154,-0.338461538461538,-0.323076923076923,
-0.307692307692308,-0.292307692307692,-0.276923076923077,-0.261538461538462,
-0.246153846153846,-0.230769230769231,-0.215384615384615,-0.2,-0.184615384615385,
-0.169230769230769,-0.153846153846154,-0.138461538461538,-0.123076923076923,
-0.107692307692308,-0.0923076923076923,-0.0769230769230769,-0.0615384615384615,
-0.0461538461538462,-0.0307692307692308,-0.0153846153846154,0.),
 .UNSPECIFIED.)
CURVE()
GEOMETRIC_REPRESENTATION_ITEM()
RATIONAL_B_SPLINE_CURVE((1.,1.,1.,1.,1.,1.,1.,1.,1.,1.,1.,1.,1.,1.,1.,1.,
1.,1.,1.,1.,1.,1.,1.,1.,1.,1.,1.,1.,1.,1.,1.,1.,1.,1.,1.,1.,1.,1.,1.,1.,
1.,1.,1.,1.,1.,1.,1.,1.,1.,1.,1.,1.,1.,1.,1.,1.,1.,1.,1.,1.,1.,1.,1.,1.,
1.,1.,1.,1.,1.,1.))
REPRESENTATION_ITEM('')
);
#367=(
BOUNDED_CURVE()
B_SPLINE_CURVE(5,(#61571,#61572,#61573,#61574,#61575,#61576,#61577,#61578,
#61579,#61580,#61581,#61582,#61583,#61584,#61585,#61586,#61587,#61588,#61589,
#61590,#61591,#61592,#61593,#61594,#61595,#61596,#61597,#61598,#61599,#61600,
#61601,#61602,#61603,#61604,#61605,#61606,#61607,#61608,#61609,#61610,#61611,
#61612,#61613,#61614,#61615,#61616,#61617,#61618,#61619,#61620,#61621,#61622,
#61623,#61624,#61625,#61626,#61627,#61628,#61629,#61630,#61631,#61632,#61633,
#61634,#61635,#61636,#61637,#61638,#61639,#61640),.UNSPECIFIED.,.F.,.F.)
B_SPLINE_CURVE_WITH_KNOTS((6,1,1,1,1,1,1,1,1,1,1,1,1,1,1,1,1,1,1,1,1,1,
1,1,1,1,1,1,1,1,1,1,1,1,1,1,1,1,1,1,1,1,1,1,1,1,1,1,1,1,1,1,1,1,1,1,1,1,
1,1,1,1,1,1,1,6),(-1.,-0.984615384615383,-0.969230769230768,-0.953846153846152,
-0.938461538461537,-0.923076923076922,-0.907692307692306,-0.892307692307691,
-0.876923076923076,-0.86153846153846,-0.846153846153845,-0.83076923076923,
-0.815384615384614,-0.799999999999999,-0.784615384615384,-0.769230769230768,
-0.753846153846153,-0.738461538461538,-0.723076923076922,-0.707692307692307,
-0.692307692307692,-0.676923076923076,-0.661538461538461,-0.646153846153846,
-0.63076923076923,-0.615384615384615,-0.6,-0.584615384615384,-0.569230769230769,
-0.553846153846154,-0.538461538461538,-0.523076923076923,-0.507692307692308,
-0.492307692307692,-0.476923076923077,-0.461538461538462,-0.446153846153846,
-0.430769230769231,-0.415384615384615,-0.4,-0.384615384615385,-0.369230769230769,
-0.353846153846154,-0.338461538461538,-0.323076923076923,-0.307692307692308,
-0.292307692307692,-0.276923076923077,-0.261538461538462,-0.246153846153846,
-0.230769230769231,-0.215384615384615,-0.2,-0.184615384615385,-0.169230769230769,
-0.153846153846154,-0.138461538461538,-0.123076923076923,-0.107692307692308,
-0.0923076923076923,-0.0769230769230769,-0.0615384615384615,-0.0461538461538462,
-0.0307692307692308,-0.0153846153846154,-0.00577184337450328),
 .UNSPECIFIED.)
CURVE()
GEOMETRIC_REPRESENTATION_ITEM()
RATIONAL_B_SPLINE_CURVE((1.,1.,1.,1.,1.,1.,1.,1.,1.,1.,1.,1.,1.,1.,1.,1.,
1.,1.,1.,1.,1.,1.,1.,1.,1.,1.,1.,1.,1.,1.,1.,1.,1.,1.,1.,1.,1.,1.,1.,1.,
1.,1.,1.,1.,1.,1.,1.,1.,1.,1.,1.,1.,1.,1.,1.,1.,1.,1.,1.,1.,1.,1.,1.,1.,
1.,1.,1.,1.,1.,1.))
REPRESENTATION_ITEM('')
);
#368=(
BOUNDED_CURVE()
B_SPLINE_CURVE(5,(#61793,#61794,#61795,#61796,#61797,#61798,#61799,#61800,
#61801,#61802,#61803,#61804,#61805,#61806,#61807,#61808,#61809,#61810,#61811,
#61812,#61813,#61814,#61815,#61816,#61817,#61818,#61819,#61820,#61821,#61822,
#61823,#61824,#61825,#61826,#61827,#61828,#61829,#61830,#61831,#61832,#61833,
#61834,#61835,#61836,#61837,#61838,#61839,#61840,#61841,#61842,#61843,#61844,
#61845,#61846,#61847,#61848,#61849,#61850,#61851,#61852,#61853,#61854,#61855,
#61856,#61857,#61858,#61859,#61860,#61861,#61862),.UNSPECIFIED.,.F.,.F.)
B_SPLINE_CURVE_WITH_KNOTS((6,1,1,1,1,1,1,1,1,1,1,1,1,1,1,1,1,1,1,1,1,1,
1,1,1,1,1,1,1,1,1,1,1,1,1,1,1,1,1,1,1,1,1,1,1,1,1,1,1,1,1,1,1,1,1,1,1,1,
1,1,1,1,1,1,1,6),(-0.994228156739672,-0.984615384615383,-0.969230769230768,
-0.953846153846152,-0.938461538461537,-0.923076923076922,-0.907692307692306,
-0.892307692307691,-0.876923076923076,-0.86153846153846,-0.846153846153845,
-0.83076923076923,-0.815384615384614,-0.799999999999999,-0.784615384615384,
-0.769230769230768,-0.753846153846153,-0.738461538461538,-0.723076923076922,
-0.707692307692307,-0.692307692307692,-0.676923076923076,-0.661538461538461,
-0.646153846153846,-0.63076923076923,-0.615384615384615,-0.6,-0.584615384615384,
-0.569230769230769,-0.553846153846154,-0.538461538461538,-0.523076923076923,
-0.507692307692308,-0.492307692307692,-0.476923076923077,-0.461538461538462,
-0.446153846153846,-0.430769230769231,-0.415384615384615,-0.4,-0.384615384615385,
-0.369230769230769,-0.353846153846154,-0.338461538461538,-0.323076923076923,
-0.307692307692308,-0.292307692307692,-0.276923076923077,-0.261538461538462,
-0.246153846153846,-0.230769230769231,-0.215384615384615,-0.2,-0.184615384615385,
-0.169230769230769,-0.153846153846154,-0.138461538461538,-0.123076923076923,
-0.107692307692308,-0.0923076923076923,-0.0769230769230769,-0.0615384615384615,
-0.0461538461538462,-0.0307692307692308,-0.0153846153846154,0.),
 .UNSPECIFIED.)
CURVE()
GEOMETRIC_REPRESENTATION_ITEM()
RATIONAL_B_SPLINE_CURVE((1.,1.,1.,1.,1.,1.,1.,1.,1.,1.,1.,1.,1.,1.,1.,1.,
1.,1.,1.,1.,1.,1.,1.,1.,1.,1.,1.,1.,1.,1.,1.,1.,1.,1.,1.,1.,1.,1.,1.,1.,
1.,1.,1.,1.,1.,1.,1.,1.,1.,1.,1.,1.,1.,1.,1.,1.,1.,1.,1.,1.,1.,1.,1.,1.,
1.,1.,1.,1.,1.,1.))
REPRESENTATION_ITEM('')
);
#369=(
BOUNDED_CURVE()
B_SPLINE_CURVE(5,(#62021,#62022,#62023,#62024,#62025,#62026,#62027,#62028,
#62029,#62030,#62031,#62032,#62033,#62034,#62035,#62036,#62037,#62038,#62039,
#62040,#62041,#62042,#62043,#62044,#62045,#62046,#62047,#62048,#62049,#62050,
#62051,#62052,#62053,#62054,#62055,#62056,#62057,#62058,#62059,#62060,#62061,
#62062,#62063,#62064,#62065,#62066,#62067,#62068,#62069,#62070,#62071,#62072,
#62073,#62074,#62075,#62076,#62077,#62078,#62079,#62080,#62081,#62082,#62083,
#62084,#62085,#62086,#62087,#62088,#62089,#62090),.UNSPECIFIED.,.F.,.F.)
B_SPLINE_CURVE_WITH_KNOTS((6,1,1,1,1,1,1,1,1,1,1,1,1,1,1,1,1,1,1,1,1,1,
1,1,1,1,1,1,1,1,1,1,1,1,1,1,1,1,1,1,1,1,1,1,1,1,1,1,1,1,1,1,1,1,1,1,1,1,
1,1,1,1,1,1,1,6),(-0.994228156739704,-0.984615384615383,-0.969230769230768,
-0.953846153846152,-0.938461538461537,-0.923076923076922,-0.907692307692306,
-0.892307692307691,-0.876923076923076,-0.86153846153846,-0.846153846153845,
-0.83076923076923,-0.815384615384614,-0.799999999999999,-0.784615384615384,
-0.769230769230768,-0.753846153846153,-0.738461538461538,-0.723076923076922,
-0.707692307692307,-0.692307692307692,-0.676923076923076,-0.661538461538461,
-0.646153846153846,-0.63076923076923,-0.615384615384615,-0.6,-0.584615384615384,
-0.569230769230769,-0.553846153846154,-0.538461538461538,-0.523076923076923,
-0.507692307692308,-0.492307692307692,-0.476923076923077,-0.461538461538462,
-0.446153846153846,-0.430769230769231,-0.415384615384615,-0.4,-0.384615384615385,
-0.369230769230769,-0.353846153846154,-0.338461538461538,-0.323076923076923,
-0.307692307692308,-0.292307692307692,-0.276923076923077,-0.261538461538462,
-0.246153846153846,-0.230769230769231,-0.215384615384615,-0.2,-0.184615384615385,
-0.169230769230769,-0.153846153846154,-0.138461538461538,-0.123076923076923,
-0.107692307692308,-0.0923076923076923,-0.0769230769230769,-0.0615384615384615,
-0.0461538461538462,-0.0307692307692308,-0.0153846153846154,0.),
 .UNSPECIFIED.)
CURVE()
GEOMETRIC_REPRESENTATION_ITEM()
RATIONAL_B_SPLINE_CURVE((1.,1.,1.,1.,1.,1.,1.,1.,1.,1.,1.,1.,1.,1.,1.,1.,
1.,1.,1.,1.,1.,1.,1.,1.,1.,1.,1.,1.,1.,1.,1.,1.,1.,1.,1.,1.,1.,1.,1.,1.,
1.,1.,1.,1.,1.,1.,1.,1.,1.,1.,1.,1.,1.,1.,1.,1.,1.,1.,1.,1.,1.,1.,1.,1.,
1.,1.,1.,1.,1.,1.))
REPRESENTATION_ITEM('')
);
#370=(
BOUNDED_CURVE()
B_SPLINE_CURVE(5,(#62232,#62233,#62234,#62235,#62236,#62237,#62238,#62239,
#62240,#62241,#62242,#62243,#62244,#62245,#62246,#62247,#62248,#62249,#62250,
#62251,#62252,#62253,#62254,#62255,#62256,#62257,#62258,#62259,#62260,#62261,
#62262,#62263,#62264,#62265,#62266,#62267,#62268,#62269,#62270,#62271,#62272,
#62273,#62274,#62275,#62276,#62277,#62278,#62279,#62280,#62281,#62282,#62283,
#62284,#62285,#62286,#62287,#62288,#62289,#62290,#62291,#62292,#62293,#62294,
#62295,#62296,#62297,#62298,#62299,#62300,#62301),.UNSPECIFIED.,.F.,.F.)
B_SPLINE_CURVE_WITH_KNOTS((6,1,1,1,1,1,1,1,1,1,1,1,1,1,1,1,1,1,1,1,1,1,
1,1,1,1,1,1,1,1,1,1,1,1,1,1,1,1,1,1,1,1,1,1,1,1,1,1,1,1,1,1,1,1,1,1,1,1,
1,1,1,1,1,1,1,6),(-1.,-0.984615384615383,-0.969230769230768,-0.953846153846152,
-0.938461538461537,-0.923076923076922,-0.907692307692306,-0.892307692307691,
-0.876923076923076,-0.86153846153846,-0.846153846153845,-0.83076923076923,
-0.815384615384614,-0.799999999999999,-0.784615384615384,-0.769230769230768,
-0.753846153846153,-0.738461538461538,-0.723076923076922,-0.707692307692307,
-0.692307692307692,-0.676923076923076,-0.661538461538461,-0.646153846153846,
-0.63076923076923,-0.615384615384615,-0.6,-0.584615384615384,-0.569230769230769,
-0.553846153846154,-0.538461538461538,-0.523076923076923,-0.507692307692308,
-0.492307692307692,-0.476923076923077,-0.461538461538462,-0.446153846153846,
-0.430769230769231,-0.415384615384615,-0.4,-0.384615384615385,-0.369230769230769,
-0.353846153846154,-0.338461538461538,-0.323076923076923,-0.307692307692308,
-0.292307692307692,-0.276923076923077,-0.261538461538462,-0.246153846153846,
-0.230769230769231,-0.215384615384615,-0.2,-0.184615384615385,-0.169230769230769,
-0.153846153846154,-0.138461538461538,-0.123076923076923,-0.107692307692308,
-0.0923076923076923,-0.0769230769230769,-0.0615384615384615,-0.0461538461538462,
-0.0307692307692308,-0.0153846153846154,-0.00577184337451611),
 .UNSPECIFIED.)
CURVE()
GEOMETRIC_REPRESENTATION_ITEM()
RATIONAL_B_SPLINE_CURVE((1.,1.,1.,1.,1.,1.,1.,1.,1.,1.,1.,1.,1.,1.,1.,1.,
1.,1.,1.,1.,1.,1.,1.,1.,1.,1.,1.,1.,1.,1.,1.,1.,1.,1.,1.,1.,1.,1.,1.,1.,
1.,1.,1.,1.,1.,1.,1.,1.,1.,1.,1.,1.,1.,1.,1.,1.,1.,1.,1.,1.,1.,1.,1.,1.,
1.,1.,1.,1.,1.,1.))
REPRESENTATION_ITEM('')
);
#371=ITEM_DEFINED_TRANSFORMATION($,$,#17485,#17607);
#372=ITEM_DEFINED_TRANSFORMATION($,$,#17505,#17608);
#373=ITEM_DEFINED_TRANSFORMATION($,$,#17525,#17609);
#374=ITEM_DEFINED_TRANSFORMATION($,$,#17540,#17610);
#375=ITEM_DEFINED_TRANSFORMATION($,$,#17590,#17611);
#376=ITEM_DEFINED_TRANSFORMATION($,$,#17613,#17741);
#377=ITEM_DEFINED_TRANSFORMATION($,$,#17633,#17742);
#378=ITEM_DEFINED_TRANSFORMATION($,$,#17653,#17743);
#379=ITEM_DEFINED_TRANSFORMATION($,$,#17670,#17744);
#380=ITEM_DEFINED_TRANSFORMATION($,$,#17724,#17745);
#381=ITEM_DEFINED_TRANSFORMATION($,$,#17160,#18709);
#382=ITEM_DEFINED_TRANSFORMATION($,$,#17176,#18710);
#383=ITEM_DEFINED_TRANSFORMATION($,$,#17260,#18711);
#384=ITEM_DEFINED_TRANSFORMATION($,$,#17285,#18712);
#385=ITEM_DEFINED_TRANSFORMATION($,$,#17310,#18713);
#386=ITEM_DEFINED_TRANSFORMATION($,$,#17335,#18714);
#387=ITEM_DEFINED_TRANSFORMATION($,$,#17360,#18715);
#388=ITEM_DEFINED_TRANSFORMATION($,$,#17360,#18716);
#389=ITEM_DEFINED_TRANSFORMATION($,$,#17360,#18717);
#390=ITEM_DEFINED_TRANSFORMATION($,$,#17484,#18718);
#391=ITEM_DEFINED_TRANSFORMATION($,$,#17746,#18719);
#392=ITEM_DEFINED_TRANSFORMATION($,$,#17746,#18720);
#393=ITEM_DEFINED_TRANSFORMATION($,$,#17746,#18721);
#394=ITEM_DEFINED_TRANSFORMATION($,$,#17746,#18722);
#395=ITEM_DEFINED_TRANSFORMATION($,$,#17746,#18723);
#396=ITEM_DEFINED_TRANSFORMATION($,$,#17746,#18724);
#397=ITEM_DEFINED_TRANSFORMATION($,$,#17746,#18725);
#398=ITEM_DEFINED_TRANSFORMATION($,$,#17746,#18726);
#399=ITEM_DEFINED_TRANSFORMATION($,$,#17612,#18727);
#400=ITEM_DEFINED_TRANSFORMATION($,$,#17746,#18728);
#401=ITEM_DEFINED_TRANSFORMATION($,$,#17746,#18729);
#402=ITEM_DEFINED_TRANSFORMATION($,$,#17746,#18730);
#403=ITEM_DEFINED_TRANSFORMATION($,$,#17746,#18731);
#404=ITEM_DEFINED_TRANSFORMATION($,$,#17746,#18732);
#405=ITEM_DEFINED_TRANSFORMATION($,$,#17746,#18733);
#406=ITEM_DEFINED_TRANSFORMATION($,$,#17746,#18734);
#407=ITEM_DEFINED_TRANSFORMATION($,$,#17746,#18735);
#408=ITEM_DEFINED_TRANSFORMATION($,$,#17384,#18736);
#409=ITEM_DEFINED_TRANSFORMATION($,$,#17409,#18737);
#410=ITEM_DEFINED_TRANSFORMATION($,$,#17434,#18738);
#411=ITEM_DEFINED_TRANSFORMATION($,$,#17459,#18739);
#412=ITEM_DEFINED_TRANSFORMATION($,$,#17484,#18740);
#413=ITEM_DEFINED_TRANSFORMATION($,$,#17746,#18741);
#414=ITEM_DEFINED_TRANSFORMATION($,$,#17746,#18742);
#415=ITEM_DEFINED_TRANSFORMATION($,$,#17746,#18743);
#416=ITEM_DEFINED_TRANSFORMATION($,$,#17746,#18744);
#417=ITEM_DEFINED_TRANSFORMATION($,$,#17746,#18745);
#418=ITEM_DEFINED_TRANSFORMATION($,$,#17746,#18746);
#419=ITEM_DEFINED_TRANSFORMATION($,$,#17746,#18747);
#420=ITEM_DEFINED_TRANSFORMATION($,$,#17746,#18748);
#421=ITEM_DEFINED_TRANSFORMATION($,$,#17612,#18749);
#422=ITEM_DEFINED_TRANSFORMATION($,$,#17746,#18750);
#423=ITEM_DEFINED_TRANSFORMATION($,$,#17746,#18751);
#424=ITEM_DEFINED_TRANSFORMATION($,$,#17746,#18752);
#425=ITEM_DEFINED_TRANSFORMATION($,$,#17746,#18753);
#426=ITEM_DEFINED_TRANSFORMATION($,$,#17746,#18754);
#427=ITEM_DEFINED_TRANSFORMATION($,$,#17746,#18755);
#428=ITEM_DEFINED_TRANSFORMATION($,$,#17746,#18756);
#429=ITEM_DEFINED_TRANSFORMATION($,$,#17746,#18757);
#430=ITEM_DEFINED_TRANSFORMATION($,$,#17770,#18758);
#431=ITEM_DEFINED_TRANSFORMATION($,$,#17912,#18759);
#432=ITEM_DEFINED_TRANSFORMATION($,$,#17921,#18760);
#433=ITEM_DEFINED_TRANSFORMATION($,$,#17930,#18761);
#434=ITEM_DEFINED_TRANSFORMATION($,$,#17937,#18762);
#435=ITEM_DEFINED_TRANSFORMATION($,$,#18683,#18763);
#436=ITEM_DEFINED_TRANSFORMATION($,$,#17944,#18764);
#437=ITEM_DEFINED_TRANSFORMATION($,$,#18683,#18765);
#438=ITEM_DEFINED_TRANSFORMATION($,$,#17944,#18766);
#439=ITEM_DEFINED_TRANSFORMATION($,$,#17973,#18767);
#440=ITEM_DEFINED_TRANSFORMATION($,$,#18005,#18768);
#441=ITEM_DEFINED_TRANSFORMATION($,$,#18014,#18769);
#442=ITEM_DEFINED_TRANSFORMATION($,$,#18023,#18770);
#443=ITEM_DEFINED_TRANSFORMATION($,$,#18038,#18771);
#444=ITEM_DEFINED_TRANSFORMATION($,$,#18062,#18772);
#445=ITEM_DEFINED_TRANSFORMATION($,$,#18071,#18773);
#446=ITEM_DEFINED_TRANSFORMATION($,$,#18080,#18774);
#447=ITEM_DEFINED_TRANSFORMATION($,$,#18089,#18775);
#448=ITEM_DEFINED_TRANSFORMATION($,$,#18666,#18776);
#449=ITEM_DEFINED_TRANSFORMATION($,$,#18271,#18777);
#450=ITEM_DEFINED_TRANSFORMATION($,$,#18364,#18778);
#451=ITEM_DEFINED_TRANSFORMATION($,$,#18364,#18779);
#452=ITEM_DEFINED_TRANSFORMATION($,$,#18683,#18780);
#453=ITEM_DEFINED_TRANSFORMATION($,$,#18098,#18781);
#454=ITEM_DEFINED_TRANSFORMATION($,$,#18107,#18782);
#455=ITEM_DEFINED_TRANSFORMATION($,$,#18136,#18783);
#456=ITEM_DEFINED_TRANSFORMATION($,$,#18161,#18784);
#457=ITEM_DEFINED_TRANSFORMATION($,$,#18170,#18785);
#458=ITEM_DEFINED_TRANSFORMATION($,$,#18179,#18786);
#459=ITEM_DEFINED_TRANSFORMATION($,$,#18194,#18787);
#460=ITEM_DEFINED_TRANSFORMATION($,$,#18666,#18788);
#461=ITEM_DEFINED_TRANSFORMATION($,$,#18482,#18789);
#462=ITEM_DEFINED_TRANSFORMATION($,$,#18655,#18790);
#463=ITEM_DEFINED_TRANSFORMATION($,$,#18683,#18791);
#464=ITEM_DEFINED_TRANSFORMATION($,$,#18204,#18792);
#465=ITEM_DEFINED_TRANSFORMATION($,$,#18229,#18793);
#466=ITEM_DEFINED_TRANSFORMATION($,$,#18238,#18794);
#467=ITEM_DEFINED_TRANSFORMATION($,$,#18247,#18795);
#468=ITEM_DEFINED_TRANSFORMATION($,$,#18262,#18796);
#469=ITEM_DEFINED_TRANSFORMATION($,$,#18666,#18797);
#470=ITEM_DEFINED_TRANSFORMATION($,$,#18271,#18798);
#471=ITEM_DEFINED_TRANSFORMATION($,$,#18364,#18799);
#472=ITEM_DEFINED_TRANSFORMATION($,$,#18683,#18800);
#473=ITEM_DEFINED_TRANSFORMATION($,$,#18376,#18801);
#474=ITEM_DEFINED_TRANSFORMATION($,$,#18401,#18802);
#475=ITEM_DEFINED_TRANSFORMATION($,$,#18410,#18803);
#476=ITEM_DEFINED_TRANSFORMATION($,$,#18419,#18804);
#477=ITEM_DEFINED_TRANSFORMATION($,$,#18434,#18805);
#478=ITEM_DEFINED_TRANSFORMATION($,$,#18443,#18806);
#479=ITEM_DEFINED_TRANSFORMATION($,$,#18452,#18807);
#480=ITEM_DEFINED_TRANSFORMATION($,$,#18473,#18808);
#481=ITEM_DEFINED_TRANSFORMATION($,$,#18666,#18809);
#482=ITEM_DEFINED_TRANSFORMATION($,$,#18482,#18810);
#483=ITEM_DEFINED_TRANSFORMATION($,$,#18655,#18811);
#484=ITEM_DEFINED_TRANSFORMATION($,$,#18666,#18812);
#485=ITEM_DEFINED_TRANSFORMATION($,$,#18683,#18813);
#486=ITEM_DEFINED_TRANSFORMATION($,$,#18815,#18824);
#487=ITEM_DEFINED_TRANSFORMATION($,$,#17159,#18825);
#488=ITEM_DEFINED_TRANSFORMATION($,$,#17972,#18826);
#489=ITEM_DEFINED_TRANSFORMATION($,$,#18135,#18827);
#490=ITEM_DEFINED_TRANSFORMATION($,$,#18203,#18828);
#491=ITEM_DEFINED_TRANSFORMATION($,$,#18375,#18829);
#492=ITEM_DEFINED_TRANSFORMATION($,$,#18814,#18830);
#493=(
REPRESENTATION_RELATIONSHIP($,$,#63045,#63044)
REPRESENTATION_RELATIONSHIP_WITH_TRANSFORMATION(#371)
SHAPE_REPRESENTATION_RELATIONSHIP()
);
#494=(
REPRESENTATION_RELATIONSHIP($,$,#63046,#63044)
REPRESENTATION_RELATIONSHIP_WITH_TRANSFORMATION(#372)
SHAPE_REPRESENTATION_RELATIONSHIP()
);
#495=(
REPRESENTATION_RELATIONSHIP($,$,#63047,#63044)
REPRESENTATION_RELATIONSHIP_WITH_TRANSFORMATION(#373)
SHAPE_REPRESENTATION_RELATIONSHIP()
);
#496=(
REPRESENTATION_RELATIONSHIP($,$,#63048,#63044)
REPRESENTATION_RELATIONSHIP_WITH_TRANSFORMATION(#374)
SHAPE_REPRESENTATION_RELATIONSHIP()
);
#497=(
REPRESENTATION_RELATIONSHIP($,$,#63049,#63044)
REPRESENTATION_RELATIONSHIP_WITH_TRANSFORMATION(#375)
SHAPE_REPRESENTATION_RELATIONSHIP()
);
#498=(
REPRESENTATION_RELATIONSHIP($,$,#63051,#63050)
REPRESENTATION_RELATIONSHIP_WITH_TRANSFORMATION(#376)
SHAPE_REPRESENTATION_RELATIONSHIP()
);
#499=(
REPRESENTATION_RELATIONSHIP($,$,#63052,#63050)
REPRESENTATION_RELATIONSHIP_WITH_TRANSFORMATION(#377)
SHAPE_REPRESENTATION_RELATIONSHIP()
);
#500=(
REPRESENTATION_RELATIONSHIP($,$,#63053,#63050)
REPRESENTATION_RELATIONSHIP_WITH_TRANSFORMATION(#378)
SHAPE_REPRESENTATION_RELATIONSHIP()
);
#501=(
REPRESENTATION_RELATIONSHIP($,$,#63054,#63050)
REPRESENTATION_RELATIONSHIP_WITH_TRANSFORMATION(#379)
SHAPE_REPRESENTATION_RELATIONSHIP()
);
#502=(
REPRESENTATION_RELATIONSHIP($,$,#63055,#63050)
REPRESENTATION_RELATIONSHIP_WITH_TRANSFORMATION(#380)
SHAPE_REPRESENTATION_RELATIONSHIP()
);
#503=(
REPRESENTATION_RELATIONSHIP($,$,#63033,#63032)
REPRESENTATION_RELATIONSHIP_WITH_TRANSFORMATION(#381)
SHAPE_REPRESENTATION_RELATIONSHIP()
);
#504=(
REPRESENTATION_RELATIONSHIP($,$,#63034,#63032)
REPRESENTATION_RELATIONSHIP_WITH_TRANSFORMATION(#382)
SHAPE_REPRESENTATION_RELATIONSHIP()
);
#505=(
REPRESENTATION_RELATIONSHIP($,$,#63035,#63032)
REPRESENTATION_RELATIONSHIP_WITH_TRANSFORMATION(#383)
SHAPE_REPRESENTATION_RELATIONSHIP()
);
#506=(
REPRESENTATION_RELATIONSHIP($,$,#63036,#63032)
REPRESENTATION_RELATIONSHIP_WITH_TRANSFORMATION(#384)
SHAPE_REPRESENTATION_RELATIONSHIP()
);
#507=(
REPRESENTATION_RELATIONSHIP($,$,#63037,#63032)
REPRESENTATION_RELATIONSHIP_WITH_TRANSFORMATION(#385)
SHAPE_REPRESENTATION_RELATIONSHIP()
);
#508=(
REPRESENTATION_RELATIONSHIP($,$,#63038,#63032)
REPRESENTATION_RELATIONSHIP_WITH_TRANSFORMATION(#386)
SHAPE_REPRESENTATION_RELATIONSHIP()
);
#509=(
REPRESENTATION_RELATIONSHIP($,$,#63039,#63032)
REPRESENTATION_RELATIONSHIP_WITH_TRANSFORMATION(#387)
SHAPE_REPRESENTATION_RELATIONSHIP()
);
#510=(
REPRESENTATION_RELATIONSHIP($,$,#63039,#63032)
REPRESENTATION_RELATIONSHIP_WITH_TRANSFORMATION(#388)
SHAPE_REPRESENTATION_RELATIONSHIP()
);
#511=(
REPRESENTATION_RELATIONSHIP($,$,#63039,#63032)
REPRESENTATION_RELATIONSHIP_WITH_TRANSFORMATION(#389)
SHAPE_REPRESENTATION_RELATIONSHIP()
);
#512=(
REPRESENTATION_RELATIONSHIP($,$,#63044,#63032)
REPRESENTATION_RELATIONSHIP_WITH_TRANSFORMATION(#390)
SHAPE_REPRESENTATION_RELATIONSHIP()
);
#513=(
REPRESENTATION_RELATIONSHIP($,$,#63056,#63032)
REPRESENTATION_RELATIONSHIP_WITH_TRANSFORMATION(#391)
SHAPE_REPRESENTATION_RELATIONSHIP()
);
#514=(
REPRESENTATION_RELATIONSHIP($,$,#63056,#63032)
REPRESENTATION_RELATIONSHIP_WITH_TRANSFORMATION(#392)
SHAPE_REPRESENTATION_RELATIONSHIP()
);
#515=(
REPRESENTATION_RELATIONSHIP($,$,#63056,#63032)
REPRESENTATION_RELATIONSHIP_WITH_TRANSFORMATION(#393)
SHAPE_REPRESENTATION_RELATIONSHIP()
);
#516=(
REPRESENTATION_RELATIONSHIP($,$,#63056,#63032)
REPRESENTATION_RELATIONSHIP_WITH_TRANSFORMATION(#394)
SHAPE_REPRESENTATION_RELATIONSHIP()
);
#517=(
REPRESENTATION_RELATIONSHIP($,$,#63056,#63032)
REPRESENTATION_RELATIONSHIP_WITH_TRANSFORMATION(#395)
SHAPE_REPRESENTATION_RELATIONSHIP()
);
#518=(
REPRESENTATION_RELATIONSHIP($,$,#63056,#63032)
REPRESENTATION_RELATIONSHIP_WITH_TRANSFORMATION(#396)
SHAPE_REPRESENTATION_RELATIONSHIP()
);
#519=(
REPRESENTATION_RELATIONSHIP($,$,#63056,#63032)
REPRESENTATION_RELATIONSHIP_WITH_TRANSFORMATION(#397)
SHAPE_REPRESENTATION_RELATIONSHIP()
);
#520=(
REPRESENTATION_RELATIONSHIP($,$,#63056,#63032)
REPRESENTATION_RELATIONSHIP_WITH_TRANSFORMATION(#398)
SHAPE_REPRESENTATION_RELATIONSHIP()
);
#521=(
REPRESENTATION_RELATIONSHIP($,$,#63050,#63032)
REPRESENTATION_RELATIONSHIP_WITH_TRANSFORMATION(#399)
SHAPE_REPRESENTATION_RELATIONSHIP()
);
#522=(
REPRESENTATION_RELATIONSHIP($,$,#63056,#63032)
REPRESENTATION_RELATIONSHIP_WITH_TRANSFORMATION(#400)
SHAPE_REPRESENTATION_RELATIONSHIP()
);
#523=(
REPRESENTATION_RELATIONSHIP($,$,#63056,#63032)
REPRESENTATION_RELATIONSHIP_WITH_TRANSFORMATION(#401)
SHAPE_REPRESENTATION_RELATIONSHIP()
);
#524=(
REPRESENTATION_RELATIONSHIP($,$,#63056,#63032)
REPRESENTATION_RELATIONSHIP_WITH_TRANSFORMATION(#402)
SHAPE_REPRESENTATION_RELATIONSHIP()
);
#525=(
REPRESENTATION_RELATIONSHIP($,$,#63056,#63032)
REPRESENTATION_RELATIONSHIP_WITH_TRANSFORMATION(#403)
SHAPE_REPRESENTATION_RELATIONSHIP()
);
#526=(
REPRESENTATION_RELATIONSHIP($,$,#63056,#63032)
REPRESENTATION_RELATIONSHIP_WITH_TRANSFORMATION(#404)
SHAPE_REPRESENTATION_RELATIONSHIP()
);
#527=(
REPRESENTATION_RELATIONSHIP($,$,#63056,#63032)
REPRESENTATION_RELATIONSHIP_WITH_TRANSFORMATION(#405)
SHAPE_REPRESENTATION_RELATIONSHIP()
);
#528=(
REPRESENTATION_RELATIONSHIP($,$,#63056,#63032)
REPRESENTATION_RELATIONSHIP_WITH_TRANSFORMATION(#406)
SHAPE_REPRESENTATION_RELATIONSHIP()
);
#529=(
REPRESENTATION_RELATIONSHIP($,$,#63056,#63032)
REPRESENTATION_RELATIONSHIP_WITH_TRANSFORMATION(#407)
SHAPE_REPRESENTATION_RELATIONSHIP()
);
#530=(
REPRESENTATION_RELATIONSHIP($,$,#63040,#63032)
REPRESENTATION_RELATIONSHIP_WITH_TRANSFORMATION(#408)
SHAPE_REPRESENTATION_RELATIONSHIP()
);
#531=(
REPRESENTATION_RELATIONSHIP($,$,#63041,#63032)
REPRESENTATION_RELATIONSHIP_WITH_TRANSFORMATION(#409)
SHAPE_REPRESENTATION_RELATIONSHIP()
);
#532=(
REPRESENTATION_RELATIONSHIP($,$,#63042,#63032)
REPRESENTATION_RELATIONSHIP_WITH_TRANSFORMATION(#410)
SHAPE_REPRESENTATION_RELATIONSHIP()
);
#533=(
REPRESENTATION_RELATIONSHIP($,$,#63043,#63032)
REPRESENTATION_RELATIONSHIP_WITH_TRANSFORMATION(#411)
SHAPE_REPRESENTATION_RELATIONSHIP()
);
#534=(
REPRESENTATION_RELATIONSHIP($,$,#63044,#63032)
REPRESENTATION_RELATIONSHIP_WITH_TRANSFORMATION(#412)
SHAPE_REPRESENTATION_RELATIONSHIP()
);
#535=(
REPRESENTATION_RELATIONSHIP($,$,#63056,#63032)
REPRESENTATION_RELATIONSHIP_WITH_TRANSFORMATION(#413)
SHAPE_REPRESENTATION_RELATIONSHIP()
);
#536=(
REPRESENTATION_RELATIONSHIP($,$,#63056,#63032)
REPRESENTATION_RELATIONSHIP_WITH_TRANSFORMATION(#414)
SHAPE_REPRESENTATION_RELATIONSHIP()
);
#537=(
REPRESENTATION_RELATIONSHIP($,$,#63056,#63032)
REPRESENTATION_RELATIONSHIP_WITH_TRANSFORMATION(#415)
SHAPE_REPRESENTATION_RELATIONSHIP()
);
#538=(
REPRESENTATION_RELATIONSHIP($,$,#63056,#63032)
REPRESENTATION_RELATIONSHIP_WITH_TRANSFORMATION(#416)
SHAPE_REPRESENTATION_RELATIONSHIP()
);
#539=(
REPRESENTATION_RELATIONSHIP($,$,#63056,#63032)
REPRESENTATION_RELATIONSHIP_WITH_TRANSFORMATION(#417)
SHAPE_REPRESENTATION_RELATIONSHIP()
);
#540=(
REPRESENTATION_RELATIONSHIP($,$,#63056,#63032)
REPRESENTATION_RELATIONSHIP_WITH_TRANSFORMATION(#418)
SHAPE_REPRESENTATION_RELATIONSHIP()
);
#541=(
REPRESENTATION_RELATIONSHIP($,$,#63056,#63032)
REPRESENTATION_RELATIONSHIP_WITH_TRANSFORMATION(#419)
SHAPE_REPRESENTATION_RELATIONSHIP()
);
#542=(
REPRESENTATION_RELATIONSHIP($,$,#63056,#63032)
REPRESENTATION_RELATIONSHIP_WITH_TRANSFORMATION(#420)
SHAPE_REPRESENTATION_RELATIONSHIP()
);
#543=(
REPRESENTATION_RELATIONSHIP($,$,#63050,#63032)
REPRESENTATION_RELATIONSHIP_WITH_TRANSFORMATION(#421)
SHAPE_REPRESENTATION_RELATIONSHIP()
);
#544=(
REPRESENTATION_RELATIONSHIP($,$,#63056,#63032)
REPRESENTATION_RELATIONSHIP_WITH_TRANSFORMATION(#422)
SHAPE_REPRESENTATION_RELATIONSHIP()
);
#545=(
REPRESENTATION_RELATIONSHIP($,$,#63056,#63032)
REPRESENTATION_RELATIONSHIP_WITH_TRANSFORMATION(#423)
SHAPE_REPRESENTATION_RELATIONSHIP()
);
#546=(
REPRESENTATION_RELATIONSHIP($,$,#63056,#63032)
REPRESENTATION_RELATIONSHIP_WITH_TRANSFORMATION(#424)
SHAPE_REPRESENTATION_RELATIONSHIP()
);
#547=(
REPRESENTATION_RELATIONSHIP($,$,#63056,#63032)
REPRESENTATION_RELATIONSHIP_WITH_TRANSFORMATION(#425)
SHAPE_REPRESENTATION_RELATIONSHIP()
);
#548=(
REPRESENTATION_RELATIONSHIP($,$,#63056,#63032)
REPRESENTATION_RELATIONSHIP_WITH_TRANSFORMATION(#426)
SHAPE_REPRESENTATION_RELATIONSHIP()
);
#549=(
REPRESENTATION_RELATIONSHIP($,$,#63056,#63032)
REPRESENTATION_RELATIONSHIP_WITH_TRANSFORMATION(#427)
SHAPE_REPRESENTATION_RELATIONSHIP()
);
#550=(
REPRESENTATION_RELATIONSHIP($,$,#63056,#63032)
REPRESENTATION_RELATIONSHIP_WITH_TRANSFORMATION(#428)
SHAPE_REPRESENTATION_RELATIONSHIP()
);
#551=(
REPRESENTATION_RELATIONSHIP($,$,#63056,#63032)
REPRESENTATION_RELATIONSHIP_WITH_TRANSFORMATION(#429)
SHAPE_REPRESENTATION_RELATIONSHIP()
);
#552=(
REPRESENTATION_RELATIONSHIP($,$,#63057,#63032)
REPRESENTATION_RELATIONSHIP_WITH_TRANSFORMATION(#430)
SHAPE_REPRESENTATION_RELATIONSHIP()
);
#553=(
REPRESENTATION_RELATIONSHIP($,$,#63058,#63032)
REPRESENTATION_RELATIONSHIP_WITH_TRANSFORMATION(#431)
SHAPE_REPRESENTATION_RELATIONSHIP()
);
#554=(
REPRESENTATION_RELATIONSHIP($,$,#63059,#63032)
REPRESENTATION_RELATIONSHIP_WITH_TRANSFORMATION(#432)
SHAPE_REPRESENTATION_RELATIONSHIP()
);
#555=(
REPRESENTATION_RELATIONSHIP($,$,#63060,#63032)
REPRESENTATION_RELATIONSHIP_WITH_TRANSFORMATION(#433)
SHAPE_REPRESENTATION_RELATIONSHIP()
);
#556=(
REPRESENTATION_RELATIONSHIP($,$,#63061,#63032)
REPRESENTATION_RELATIONSHIP_WITH_TRANSFORMATION(#434)
SHAPE_REPRESENTATION_RELATIONSHIP()
);
#557=(
REPRESENTATION_RELATIONSHIP($,$,#63101,#63032)
REPRESENTATION_RELATIONSHIP_WITH_TRANSFORMATION(#435)
SHAPE_REPRESENTATION_RELATIONSHIP()
);
#558=(
REPRESENTATION_RELATIONSHIP($,$,#63062,#63032)
REPRESENTATION_RELATIONSHIP_WITH_TRANSFORMATION(#436)
SHAPE_REPRESENTATION_RELATIONSHIP()
);
#559=(
REPRESENTATION_RELATIONSHIP($,$,#63101,#63032)
REPRESENTATION_RELATIONSHIP_WITH_TRANSFORMATION(#437)
SHAPE_REPRESENTATION_RELATIONSHIP()
);
#560=(
REPRESENTATION_RELATIONSHIP($,$,#63062,#63032)
REPRESENTATION_RELATIONSHIP_WITH_TRANSFORMATION(#438)
SHAPE_REPRESENTATION_RELATIONSHIP()
);
#561=(
REPRESENTATION_RELATIONSHIP($,$,#63064,#63063)
REPRESENTATION_RELATIONSHIP_WITH_TRANSFORMATION(#439)
SHAPE_REPRESENTATION_RELATIONSHIP()
);
#562=(
REPRESENTATION_RELATIONSHIP($,$,#63065,#63063)
REPRESENTATION_RELATIONSHIP_WITH_TRANSFORMATION(#440)
SHAPE_REPRESENTATION_RELATIONSHIP()
);
#563=(
REPRESENTATION_RELATIONSHIP($,$,#63066,#63063)
REPRESENTATION_RELATIONSHIP_WITH_TRANSFORMATION(#441)
SHAPE_REPRESENTATION_RELATIONSHIP()
);
#564=(
REPRESENTATION_RELATIONSHIP($,$,#63067,#63063)
REPRESENTATION_RELATIONSHIP_WITH_TRANSFORMATION(#442)
SHAPE_REPRESENTATION_RELATIONSHIP()
);
#565=(
REPRESENTATION_RELATIONSHIP($,$,#63068,#63063)
REPRESENTATION_RELATIONSHIP_WITH_TRANSFORMATION(#443)
SHAPE_REPRESENTATION_RELATIONSHIP()
);
#566=(
REPRESENTATION_RELATIONSHIP($,$,#63069,#63063)
REPRESENTATION_RELATIONSHIP_WITH_TRANSFORMATION(#444)
SHAPE_REPRESENTATION_RELATIONSHIP()
);
#567=(
REPRESENTATION_RELATIONSHIP($,$,#63070,#63063)
REPRESENTATION_RELATIONSHIP_WITH_TRANSFORMATION(#445)
SHAPE_REPRESENTATION_RELATIONSHIP()
);
#568=(
REPRESENTATION_RELATIONSHIP($,$,#63071,#63063)
REPRESENTATION_RELATIONSHIP_WITH_TRANSFORMATION(#446)
SHAPE_REPRESENTATION_RELATIONSHIP()
);
#569=(
REPRESENTATION_RELATIONSHIP($,$,#63072,#63063)
REPRESENTATION_RELATIONSHIP_WITH_TRANSFORMATION(#447)
SHAPE_REPRESENTATION_RELATIONSHIP()
);
#570=(
REPRESENTATION_RELATIONSHIP($,$,#63100,#63063)
REPRESENTATION_RELATIONSHIP_WITH_TRANSFORMATION(#448)
SHAPE_REPRESENTATION_RELATIONSHIP()
);
#571=(
REPRESENTATION_RELATIONSHIP($,$,#63087,#63063)
REPRESENTATION_RELATIONSHIP_WITH_TRANSFORMATION(#449)
SHAPE_REPRESENTATION_RELATIONSHIP()
);
#572=(
REPRESENTATION_RELATIONSHIP($,$,#63088,#63063)
REPRESENTATION_RELATIONSHIP_WITH_TRANSFORMATION(#450)
SHAPE_REPRESENTATION_RELATIONSHIP()
);
#573=(
REPRESENTATION_RELATIONSHIP($,$,#63088,#63063)
REPRESENTATION_RELATIONSHIP_WITH_TRANSFORMATION(#451)
SHAPE_REPRESENTATION_RELATIONSHIP()
);
#574=(
REPRESENTATION_RELATIONSHIP($,$,#63101,#63063)
REPRESENTATION_RELATIONSHIP_WITH_TRANSFORMATION(#452)
SHAPE_REPRESENTATION_RELATIONSHIP()
);
#575=(
REPRESENTATION_RELATIONSHIP($,$,#63073,#63063)
REPRESENTATION_RELATIONSHIP_WITH_TRANSFORMATION(#453)
SHAPE_REPRESENTATION_RELATIONSHIP()
);
#576=(
REPRESENTATION_RELATIONSHIP($,$,#63074,#63063)
REPRESENTATION_RELATIONSHIP_WITH_TRANSFORMATION(#454)
SHAPE_REPRESENTATION_RELATIONSHIP()
);
#577=(
REPRESENTATION_RELATIONSHIP($,$,#63076,#63075)
REPRESENTATION_RELATIONSHIP_WITH_TRANSFORMATION(#455)
SHAPE_REPRESENTATION_RELATIONSHIP()
);
#578=(
REPRESENTATION_RELATIONSHIP($,$,#63077,#63075)
REPRESENTATION_RELATIONSHIP_WITH_TRANSFORMATION(#456)
SHAPE_REPRESENTATION_RELATIONSHIP()
);
#579=(
REPRESENTATION_RELATIONSHIP($,$,#63078,#63075)
REPRESENTATION_RELATIONSHIP_WITH_TRANSFORMATION(#457)
SHAPE_REPRESENTATION_RELATIONSHIP()
);
#580=(
REPRESENTATION_RELATIONSHIP($,$,#63079,#63075)
REPRESENTATION_RELATIONSHIP_WITH_TRANSFORMATION(#458)
SHAPE_REPRESENTATION_RELATIONSHIP()
);
#581=(
REPRESENTATION_RELATIONSHIP($,$,#63080,#63075)
REPRESENTATION_RELATIONSHIP_WITH_TRANSFORMATION(#459)
SHAPE_REPRESENTATION_RELATIONSHIP()
);
#582=(
REPRESENTATION_RELATIONSHIP($,$,#63100,#63075)
REPRESENTATION_RELATIONSHIP_WITH_TRANSFORMATION(#460)
SHAPE_REPRESENTATION_RELATIONSHIP()
);
#583=(
REPRESENTATION_RELATIONSHIP($,$,#63098,#63075)
REPRESENTATION_RELATIONSHIP_WITH_TRANSFORMATION(#461)
SHAPE_REPRESENTATION_RELATIONSHIP()
);
#584=(
REPRESENTATION_RELATIONSHIP($,$,#63099,#63075)
REPRESENTATION_RELATIONSHIP_WITH_TRANSFORMATION(#462)
SHAPE_REPRESENTATION_RELATIONSHIP()
);
#585=(
REPRESENTATION_RELATIONSHIP($,$,#63101,#63075)
REPRESENTATION_RELATIONSHIP_WITH_TRANSFORMATION(#463)
SHAPE_REPRESENTATION_RELATIONSHIP()
);
#586=(
REPRESENTATION_RELATIONSHIP($,$,#63082,#63081)
REPRESENTATION_RELATIONSHIP_WITH_TRANSFORMATION(#464)
SHAPE_REPRESENTATION_RELATIONSHIP()
);
#587=(
REPRESENTATION_RELATIONSHIP($,$,#63083,#63081)
REPRESENTATION_RELATIONSHIP_WITH_TRANSFORMATION(#465)
SHAPE_REPRESENTATION_RELATIONSHIP()
);
#588=(
REPRESENTATION_RELATIONSHIP($,$,#63084,#63081)
REPRESENTATION_RELATIONSHIP_WITH_TRANSFORMATION(#466)
SHAPE_REPRESENTATION_RELATIONSHIP()
);
#589=(
REPRESENTATION_RELATIONSHIP($,$,#63085,#63081)
REPRESENTATION_RELATIONSHIP_WITH_TRANSFORMATION(#467)
SHAPE_REPRESENTATION_RELATIONSHIP()
);
#590=(
REPRESENTATION_RELATIONSHIP($,$,#63086,#63081)
REPRESENTATION_RELATIONSHIP_WITH_TRANSFORMATION(#468)
SHAPE_REPRESENTATION_RELATIONSHIP()
);
#591=(
REPRESENTATION_RELATIONSHIP($,$,#63100,#63081)
REPRESENTATION_RELATIONSHIP_WITH_TRANSFORMATION(#469)
SHAPE_REPRESENTATION_RELATIONSHIP()
);
#592=(
REPRESENTATION_RELATIONSHIP($,$,#63087,#63081)
REPRESENTATION_RELATIONSHIP_WITH_TRANSFORMATION(#470)
SHAPE_REPRESENTATION_RELATIONSHIP()
);
#593=(
REPRESENTATION_RELATIONSHIP($,$,#63088,#63081)
REPRESENTATION_RELATIONSHIP_WITH_TRANSFORMATION(#471)
SHAPE_REPRESENTATION_RELATIONSHIP()
);
#594=(
REPRESENTATION_RELATIONSHIP($,$,#63101,#63081)
REPRESENTATION_RELATIONSHIP_WITH_TRANSFORMATION(#472)
SHAPE_REPRESENTATION_RELATIONSHIP()
);
#595=(
REPRESENTATION_RELATIONSHIP($,$,#63090,#63089)
REPRESENTATION_RELATIONSHIP_WITH_TRANSFORMATION(#473)
SHAPE_REPRESENTATION_RELATIONSHIP()
);
#596=(
REPRESENTATION_RELATIONSHIP($,$,#63091,#63089)
REPRESENTATION_RELATIONSHIP_WITH_TRANSFORMATION(#474)
SHAPE_REPRESENTATION_RELATIONSHIP()
);
#597=(
REPRESENTATION_RELATIONSHIP($,$,#63092,#63089)
REPRESENTATION_RELATIONSHIP_WITH_TRANSFORMATION(#475)
SHAPE_REPRESENTATION_RELATIONSHIP()
);
#598=(
REPRESENTATION_RELATIONSHIP($,$,#63093,#63089)
REPRESENTATION_RELATIONSHIP_WITH_TRANSFORMATION(#476)
SHAPE_REPRESENTATION_RELATIONSHIP()
);
#599=(
REPRESENTATION_RELATIONSHIP($,$,#63094,#63089)
REPRESENTATION_RELATIONSHIP_WITH_TRANSFORMATION(#477)
SHAPE_REPRESENTATION_RELATIONSHIP()
);
#600=(
REPRESENTATION_RELATIONSHIP($,$,#63095,#63089)
REPRESENTATION_RELATIONSHIP_WITH_TRANSFORMATION(#478)
SHAPE_REPRESENTATION_RELATIONSHIP()
);
#601=(
REPRESENTATION_RELATIONSHIP($,$,#63096,#63089)
REPRESENTATION_RELATIONSHIP_WITH_TRANSFORMATION(#479)
SHAPE_REPRESENTATION_RELATIONSHIP()
);
#602=(
REPRESENTATION_RELATIONSHIP($,$,#63097,#63089)
REPRESENTATION_RELATIONSHIP_WITH_TRANSFORMATION(#480)
SHAPE_REPRESENTATION_RELATIONSHIP()
);
#603=(
REPRESENTATION_RELATIONSHIP($,$,#63100,#63089)
REPRESENTATION_RELATIONSHIP_WITH_TRANSFORMATION(#481)
SHAPE_REPRESENTATION_RELATIONSHIP()
);
#604=(
REPRESENTATION_RELATIONSHIP($,$,#63098,#63089)
REPRESENTATION_RELATIONSHIP_WITH_TRANSFORMATION(#482)
SHAPE_REPRESENTATION_RELATIONSHIP()
);
#605=(
REPRESENTATION_RELATIONSHIP($,$,#63099,#63089)
REPRESENTATION_RELATIONSHIP_WITH_TRANSFORMATION(#483)
SHAPE_REPRESENTATION_RELATIONSHIP()
);
#606=(
REPRESENTATION_RELATIONSHIP($,$,#63100,#63089)
REPRESENTATION_RELATIONSHIP_WITH_TRANSFORMATION(#484)
SHAPE_REPRESENTATION_RELATIONSHIP()
);
#607=(
REPRESENTATION_RELATIONSHIP($,$,#63101,#63089)
REPRESENTATION_RELATIONSHIP_WITH_TRANSFORMATION(#485)
SHAPE_REPRESENTATION_RELATIONSHIP()
);
#608=(
REPRESENTATION_RELATIONSHIP($,$,#63103,#63102)
REPRESENTATION_RELATIONSHIP_WITH_TRANSFORMATION(#486)
SHAPE_REPRESENTATION_RELATIONSHIP()
);
#609=(
REPRESENTATION_RELATIONSHIP($,$,#63032,#63031)
REPRESENTATION_RELATIONSHIP_WITH_TRANSFORMATION(#487)
SHAPE_REPRESENTATION_RELATIONSHIP()
);
#610=(
REPRESENTATION_RELATIONSHIP($,$,#63063,#63031)
REPRESENTATION_RELATIONSHIP_WITH_TRANSFORMATION(#488)
SHAPE_REPRESENTATION_RELATIONSHIP()
);
#611=(
REPRESENTATION_RELATIONSHIP($,$,#63075,#63031)
REPRESENTATION_RELATIONSHIP_WITH_TRANSFORMATION(#489)
SHAPE_REPRESENTATION_RELATIONSHIP()
);
#612=(
REPRESENTATION_RELATIONSHIP($,$,#63081,#63031)
REPRESENTATION_RELATIONSHIP_WITH_TRANSFORMATION(#490)
SHAPE_REPRESENTATION_RELATIONSHIP()
);
#613=(
REPRESENTATION_RELATIONSHIP($,$,#63089,#63031)
REPRESENTATION_RELATIONSHIP_WITH_TRANSFORMATION(#491)
SHAPE_REPRESENTATION_RELATIONSHIP()
);
#614=(
REPRESENTATION_RELATIONSHIP($,$,#63102,#63031)
REPRESENTATION_RELATIONSHIP_WITH_TRANSFORMATION(#492)
SHAPE_REPRESENTATION_RELATIONSHIP()
);
#615=CONTEXT_DEPENDENT_SHAPE_REPRESENTATION(#493,#62855);
#616=CONTEXT_DEPENDENT_SHAPE_REPRESENTATION(#494,#62856);
#617=CONTEXT_DEPENDENT_SHAPE_REPRESENTATION(#495,#62857);
#618=CONTEXT_DEPENDENT_SHAPE_REPRESENTATION(#496,#62858);
#619=CONTEXT_DEPENDENT_SHAPE_REPRESENTATION(#497,#62859);
#620=CONTEXT_DEPENDENT_SHAPE_REPRESENTATION(#498,#62866);
#621=CONTEXT_DEPENDENT_SHAPE_REPRESENTATION(#499,#62867);
#622=CONTEXT_DEPENDENT_SHAPE_REPRESENTATION(#500,#62868);
#623=CONTEXT_DEPENDENT_SHAPE_REPRESENTATION(#501,#62869);
#624=CONTEXT_DEPENDENT_SHAPE_REPRESENTATION(#502,#62870);
#625=CONTEXT_DEPENDENT_SHAPE_REPRESENTATION(#503,#62917);
#626=CONTEXT_DEPENDENT_SHAPE_REPRESENTATION(#504,#62918);
#627=CONTEXT_DEPENDENT_SHAPE_REPRESENTATION(#505,#62919);
#628=CONTEXT_DEPENDENT_SHAPE_REPRESENTATION(#506,#62920);
#629=CONTEXT_DEPENDENT_SHAPE_REPRESENTATION(#507,#62921);
#630=CONTEXT_DEPENDENT_SHAPE_REPRESENTATION(#508,#62922);
#631=CONTEXT_DEPENDENT_SHAPE_REPRESENTATION(#509,#62923);
#632=CONTEXT_DEPENDENT_SHAPE_REPRESENTATION(#510,#62924);
#633=CONTEXT_DEPENDENT_SHAPE_REPRESENTATION(#511,#62925);
#634=CONTEXT_DEPENDENT_SHAPE_REPRESENTATION(#512,#62926);
#635=CONTEXT_DEPENDENT_SHAPE_REPRESENTATION(#513,#62927);
#636=CONTEXT_DEPENDENT_SHAPE_REPRESENTATION(#514,#62928);
#637=CONTEXT_DEPENDENT_SHAPE_REPRESENTATION(#515,#62929);
#638=CONTEXT_DEPENDENT_SHAPE_REPRESENTATION(#516,#62930);
#639=CONTEXT_DEPENDENT_SHAPE_REPRESENTATION(#517,#62931);
#640=CONTEXT_DEPENDENT_SHAPE_REPRESENTATION(#518,#62932);
#641=CONTEXT_DEPENDENT_SHAPE_REPRESENTATION(#519,#62933);
#642=CONTEXT_DEPENDENT_SHAPE_REPRESENTATION(#520,#62934);
#643=CONTEXT_DEPENDENT_SHAPE_REPRESENTATION(#521,#62935);
#644=CONTEXT_DEPENDENT_SHAPE_REPRESENTATION(#522,#62936);
#645=CONTEXT_DEPENDENT_SHAPE_REPRESENTATION(#523,#62937);
#646=CONTEXT_DEPENDENT_SHAPE_REPRESENTATION(#524,#62938);
#647=CONTEXT_DEPENDENT_SHAPE_REPRESENTATION(#525,#62939);
#648=CONTEXT_DEPENDENT_SHAPE_REPRESENTATION(#526,#62940);
#649=CONTEXT_DEPENDENT_SHAPE_REPRESENTATION(#527,#62941);
#650=CONTEXT_DEPENDENT_SHAPE_REPRESENTATION(#528,#62942);
#651=CONTEXT_DEPENDENT_SHAPE_REPRESENTATION(#529,#62943);
#652=CONTEXT_DEPENDENT_SHAPE_REPRESENTATION(#530,#62944);
#653=CONTEXT_DEPENDENT_SHAPE_REPRESENTATION(#531,#62945);
#654=CONTEXT_DEPENDENT_SHAPE_REPRESENTATION(#532,#62946);
#655=CONTEXT_DEPENDENT_SHAPE_REPRESENTATION(#533,#62947);
#656=CONTEXT_DEPENDENT_SHAPE_REPRESENTATION(#534,#62948);
#657=CONTEXT_DEPENDENT_SHAPE_REPRESENTATION(#535,#62949);
#658=CONTEXT_DEPENDENT_SHAPE_REPRESENTATION(#536,#62950);
#659=CONTEXT_DEPENDENT_SHAPE_REPRESENTATION(#537,#62951);
#660=CONTEXT_DEPENDENT_SHAPE_REPRESENTATION(#538,#62952);
#661=CONTEXT_DEPENDENT_SHAPE_REPRESENTATION(#539,#62953);
#662=CONTEXT_DEPENDENT_SHAPE_REPRESENTATION(#540,#62954);
#663=CONTEXT_DEPENDENT_SHAPE_REPRESENTATION(#541,#62955);
#664=CONTEXT_DEPENDENT_SHAPE_REPRESENTATION(#542,#62956);
#665=CONTEXT_DEPENDENT_SHAPE_REPRESENTATION(#543,#62957);
#666=CONTEXT_DEPENDENT_SHAPE_REPRESENTATION(#544,#62958);
#667=CONTEXT_DEPENDENT_SHAPE_REPRESENTATION(#545,#62959);
#668=CONTEXT_DEPENDENT_SHAPE_REPRESENTATION(#546,#62960);
#669=CONTEXT_DEPENDENT_SHAPE_REPRESENTATION(#547,#62961);
#670=CONTEXT_DEPENDENT_SHAPE_REPRESENTATION(#548,#62962);
#671=CONTEXT_DEPENDENT_SHAPE_REPRESENTATION(#549,#62963);
#672=CONTEXT_DEPENDENT_SHAPE_REPRESENTATION(#550,#62964);
#673=CONTEXT_DEPENDENT_SHAPE_REPRESENTATION(#551,#62965);
#674=CONTEXT_DEPENDENT_SHAPE_REPRESENTATION(#552,#62966);
#675=CONTEXT_DEPENDENT_SHAPE_REPRESENTATION(#553,#62967);
#676=CONTEXT_DEPENDENT_SHAPE_REPRESENTATION(#554,#62968);
#677=CONTEXT_DEPENDENT_SHAPE_REPRESENTATION(#555,#62969);
#678=CONTEXT_DEPENDENT_SHAPE_REPRESENTATION(#556,#62970);
#679=CONTEXT_DEPENDENT_SHAPE_REPRESENTATION(#557,#62971);
#680=CONTEXT_DEPENDENT_SHAPE_REPRESENTATION(#558,#62972);
#681=CONTEXT_DEPENDENT_SHAPE_REPRESENTATION(#559,#62973);
#682=CONTEXT_DEPENDENT_SHAPE_REPRESENTATION(#560,#62974);
#683=CONTEXT_DEPENDENT_SHAPE_REPRESENTATION(#561,#62975);
#684=CONTEXT_DEPENDENT_SHAPE_REPRESENTATION(#562,#62976);
#685=CONTEXT_DEPENDENT_SHAPE_REPRESENTATION(#563,#62977);
#686=CONTEXT_DEPENDENT_SHAPE_REPRESENTATION(#564,#62978);
#687=CONTEXT_DEPENDENT_SHAPE_REPRESENTATION(#565,#62979);
#688=CONTEXT_DEPENDENT_SHAPE_REPRESENTATION(#566,#62980);
#689=CONTEXT_DEPENDENT_SHAPE_REPRESENTATION(#567,#62981);
#690=CONTEXT_DEPENDENT_SHAPE_REPRESENTATION(#568,#62982);
#691=CONTEXT_DEPENDENT_SHAPE_REPRESENTATION(#569,#62983);
#692=CONTEXT_DEPENDENT_SHAPE_REPRESENTATION(#570,#62984);
#693=CONTEXT_DEPENDENT_SHAPE_REPRESENTATION(#571,#62985);
#694=CONTEXT_DEPENDENT_SHAPE_REPRESENTATION(#572,#62986);
#695=CONTEXT_DEPENDENT_SHAPE_REPRESENTATION(#573,#62987);
#696=CONTEXT_DEPENDENT_SHAPE_REPRESENTATION(#574,#62988);
#697=CONTEXT_DEPENDENT_SHAPE_REPRESENTATION(#575,#62989);
#698=CONTEXT_DEPENDENT_SHAPE_REPRESENTATION(#576,#62990);
#699=CONTEXT_DEPENDENT_SHAPE_REPRESENTATION(#577,#62991);
#700=CONTEXT_DEPENDENT_SHAPE_REPRESENTATION(#578,#62992);
#701=CONTEXT_DEPENDENT_SHAPE_REPRESENTATION(#579,#62993);
#702=CONTEXT_DEPENDENT_SHAPE_REPRESENTATION(#580,#62994);
#703=CONTEXT_DEPENDENT_SHAPE_REPRESENTATION(#581,#62995);
#704=CONTEXT_DEPENDENT_SHAPE_REPRESENTATION(#582,#62996);
#705=CONTEXT_DEPENDENT_SHAPE_REPRESENTATION(#583,#62997);
#706=CONTEXT_DEPENDENT_SHAPE_REPRESENTATION(#584,#62998);
#707=CONTEXT_DEPENDENT_SHAPE_REPRESENTATION(#585,#62999);
#708=CONTEXT_DEPENDENT_SHAPE_REPRESENTATION(#586,#63000);
#709=CONTEXT_DEPENDENT_SHAPE_REPRESENTATION(#587,#63001);
#710=CONTEXT_DEPENDENT_SHAPE_REPRESENTATION(#588,#63002);
#711=CONTEXT_DEPENDENT_SHAPE_REPRESENTATION(#589,#63003);
#712=CONTEXT_DEPENDENT_SHAPE_REPRESENTATION(#590,#63004);
#713=CONTEXT_DEPENDENT_SHAPE_REPRESENTATION(#591,#63005);
#714=CONTEXT_DEPENDENT_SHAPE_REPRESENTATION(#592,#63006);
#715=CONTEXT_DEPENDENT_SHAPE_REPRESENTATION(#593,#63007);
#716=CONTEXT_DEPENDENT_SHAPE_REPRESENTATION(#594,#63008);
#717=CONTEXT_DEPENDENT_SHAPE_REPRESENTATION(#595,#63009);
#718=CONTEXT_DEPENDENT_SHAPE_REPRESENTATION(#596,#63010);
#719=CONTEXT_DEPENDENT_SHAPE_REPRESENTATION(#597,#63011);
#720=CONTEXT_DEPENDENT_SHAPE_REPRESENTATION(#598,#63012);
#721=CONTEXT_DEPENDENT_SHAPE_REPRESENTATION(#599,#63013);
#722=CONTEXT_DEPENDENT_SHAPE_REPRESENTATION(#600,#63014);
#723=CONTEXT_DEPENDENT_SHAPE_REPRESENTATION(#601,#63015);
#724=CONTEXT_DEPENDENT_SHAPE_REPRESENTATION(#602,#63016);
#725=CONTEXT_DEPENDENT_SHAPE_REPRESENTATION(#603,#63017);
#726=CONTEXT_DEPENDENT_SHAPE_REPRESENTATION(#604,#63018);
#727=CONTEXT_DEPENDENT_SHAPE_REPRESENTATION(#605,#63019);
#728=CONTEXT_DEPENDENT_SHAPE_REPRESENTATION(#606,#63020);
#729=CONTEXT_DEPENDENT_SHAPE_REPRESENTATION(#607,#63021);
#730=CONTEXT_DEPENDENT_SHAPE_REPRESENTATION(#608,#63024);
#731=CONTEXT_DEPENDENT_SHAPE_REPRESENTATION(#609,#63025);
#732=CONTEXT_DEPENDENT_SHAPE_REPRESENTATION(#610,#63026);
#733=CONTEXT_DEPENDENT_SHAPE_REPRESENTATION(#611,#63027);
#734=CONTEXT_DEPENDENT_SHAPE_REPRESENTATION(#612,#63028);
#735=CONTEXT_DEPENDENT_SHAPE_REPRESENTATION(#613,#63029);
#736=CONTEXT_DEPENDENT_SHAPE_REPRESENTATION(#614,#63030);
#737=NEXT_ASSEMBLY_USAGE_OCCURRENCE('Inner ring:1','Inner ring:1',
'Inner ring:1',#63118,#63119,'Inner ring:1');
#738=NEXT_ASSEMBLY_USAGE_OCCURRENCE('Outer ring:1','Outer ring:1',
'Outer ring:1',#63118,#63120,'Outer ring:1');
#739=NEXT_ASSEMBLY_USAGE_OCCURRENCE('Balls:1','Balls:1','Balls:1',#63118,
#63121,'Balls:1');
#740=NEXT_ASSEMBLY_USAGE_OCCURRENCE('Cage:1','Cage:1','Cage:1',#63118,#63122,
'Cage:1');
#741=NEXT_ASSEMBLY_USAGE_OCCURRENCE('Seals 2RS:1','Seals 2RS:1',
'Seals 2RS:1',#63118,#63123,'Seals 2RS:1');
#742=NEXT_ASSEMBLY_USAGE_OCCURRENCE('Inner ring (1):1',
'Inner ring (1):1','Inner ring (1):1',#63124,#63125,'Inner ring (1):1');
#743=NEXT_ASSEMBLY_USAGE_OCCURRENCE('Outer ring (1):1',
'Outer ring (1):1','Outer ring (1):1',#63124,#63126,'Outer ring (1):1');
#744=NEXT_ASSEMBLY_USAGE_OCCURRENCE('Balls (1):1','Balls (1):1',
'Balls (1):1',#63124,#63127,'Balls (1):1');
#745=NEXT_ASSEMBLY_USAGE_OCCURRENCE('Cage (1):1','Cage (1):1',
'Cage (1):1',#63124,#63128,'Cage (1):1');
#746=NEXT_ASSEMBLY_USAGE_OCCURRENCE('Seals 2RS (1):1','Seals 2RS (1):1',
'Seals 2RS (1):1',#63124,#63129,'Seals 2RS (1):1');
#747=NEXT_ASSEMBLY_USAGE_OCCURRENCE('Base:1','Base:1','Base:1',#63106,#63107,
'Base:1');
#748=NEXT_ASSEMBLY_USAGE_OCCURRENCE('Bearing plate:1','Bearing plate:1',
'Bearing plate:1',#63106,#63108,'Bearing plate:1');
#749=NEXT_ASSEMBLY_USAGE_OCCURRENCE('mm bearing cap:1',
'mm bearing cap:1','mm bearing cap:1',#63106,#63109,'mm bearing cap:1');
#750=NEXT_ASSEMBLY_USAGE_OCCURRENCE('mm bearing cap (1):1',
'mm bearing cap (1):1','mm bearing cap (1):1',#63106,#63110,
'mm bearing cap (1):1');
#751=NEXT_ASSEMBLY_USAGE_OCCURRENCE('mm bearing cap (2):1',
'mm bearing cap (2):1','mm bearing cap (2):1',#63106,#63111,
'mm bearing cap (2):1');
#752=NEXT_ASSEMBLY_USAGE_OCCURRENCE('mm bearing cap (3):1',
'mm bearing cap (3):1','mm bearing cap (3):1',#63106,#63112,
'mm bearing cap (3):1');
#753=NEXT_ASSEMBLY_USAGE_OCCURRENCE('M6x18 mounting screw:2',
'M6x18 mounting screw:2','M6x18 mounting screw:2',#63106,#63113,
'M6x18 mounting screw:2');
#754=NEXT_ASSEMBLY_USAGE_OCCURRENCE('M6x18 mounting screw:3',
'M6x18 mounting screw:3','M6x18 mounting screw:3',#63106,#63113,
'M6x18 mounting screw:3');
#755=NEXT_ASSEMBLY_USAGE_OCCURRENCE('M6x18 mounting screw:4',
'M6x18 mounting screw:4','M6x18 mounting screw:4',#63106,#63113,
'M6x18 mounting screw:4');
#756=NEXT_ASSEMBLY_USAGE_OCCURRENCE(
'Sealed Ball Bearing - 12 x 32 x 10 mm:2',
'Sealed Ball Bearing - 12 x 32 x 10 mm:2',
'Sealed Ball Bearing - 12 x 32 x 10 mm:2',#63106,#63118,
'Sealed Ball Bearing - 12 x 32 x 10 mm:2');
#757=NEXT_ASSEMBLY_USAGE_OCCURRENCE('M4x10 Cap Screw:2',
'M4x10 Cap Screw:2','M4x10 Cap Screw:2',#63106,#63130,
'M4x10 Cap Screw:2');
#758=NEXT_ASSEMBLY_USAGE_OCCURRENCE('M4x10 Cap Screw:3',
'M4x10 Cap Screw:3','M4x10 Cap Screw:3',#63106,#63130,
'M4x10 Cap Screw:3');
#759=NEXT_ASSEMBLY_USAGE_OCCURRENCE('M4x10 Cap Screw:4',
'M4x10 Cap Screw:4','M4x10 Cap Screw:4',#63106,#63130,
'M4x10 Cap Screw:4');
#760=NEXT_ASSEMBLY_USAGE_OCCURRENCE('M4x10 Cap Screw:5',
'M4x10 Cap Screw:5','M4x10 Cap Screw:5',#63106,#63130,
'M4x10 Cap Screw:5');
#761=NEXT_ASSEMBLY_USAGE_OCCURRENCE('M4x10 Cap Screw:6',
'M4x10 Cap Screw:6','M4x10 Cap Screw:6',#63106,#63130,
'M4x10 Cap Screw:6');
#762=NEXT_ASSEMBLY_USAGE_OCCURRENCE('M4x10 Cap Screw:7',
'M4x10 Cap Screw:7','M4x10 Cap Screw:7',#63106,#63130,
'M4x10 Cap Screw:7');
#763=NEXT_ASSEMBLY_USAGE_OCCURRENCE('M4x10 Cap Screw:8',
'M4x10 Cap Screw:8','M4x10 Cap Screw:8',#63106,#63130,
'M4x10 Cap Screw:8');
#764=NEXT_ASSEMBLY_USAGE_OCCURRENCE('M4x10 Cap Screw:9',
'M4x10 Cap Screw:9','M4x10 Cap Screw:9',#63106,#63130,
'M4x10 Cap Screw:9');
#765=NEXT_ASSEMBLY_USAGE_OCCURRENCE(
'Sealed Ball Bearing - 20 x 47 x 14 mm:2',
'Sealed Ball Bearing - 20 x 47 x 14 mm:2',
'Sealed Ball Bearing - 20 x 47 x 14 mm:2',#63106,#63124,
'Sealed Ball Bearing - 20 x 47 x 14 mm:2');
#766=NEXT_ASSEMBLY_USAGE_OCCURRENCE('M4x10 Cap Screw:10',
'M4x10 Cap Screw:10','M4x10 Cap Screw:10',#63106,#63130,
'M4x10 Cap Screw:10');
#767=NEXT_ASSEMBLY_USAGE_OCCURRENCE('M4x10 Cap Screw:11',
'M4x10 Cap Screw:11','M4x10 Cap Screw:11',#63106,#63130,
'M4x10 Cap Screw:11');
#768=NEXT_ASSEMBLY_USAGE_OCCURRENCE('M4x10 Cap Screw:12',
'M4x10 Cap Screw:12','M4x10 Cap Screw:12',#63106,#63130,
'M4x10 Cap Screw:12');
#769=NEXT_ASSEMBLY_USAGE_OCCURRENCE('M4x10 Cap Screw:13',
'M4x10 Cap Screw:13','M4x10 Cap Screw:13',#63106,#63130,
'M4x10 Cap Screw:13');
#770=NEXT_ASSEMBLY_USAGE_OCCURRENCE('M4x10 Cap Screw:14',
'M4x10 Cap Screw:14','M4x10 Cap Screw:14',#63106,#63130,
'M4x10 Cap Screw:14');
#771=NEXT_ASSEMBLY_USAGE_OCCURRENCE('M4x10 Cap Screw:15',
'M4x10 Cap Screw:15','M4x10 Cap Screw:15',#63106,#63130,
'M4x10 Cap Screw:15');
#772=NEXT_ASSEMBLY_USAGE_OCCURRENCE('M4x10 Cap Screw:16',
'M4x10 Cap Screw:16','M4x10 Cap Screw:16',#63106,#63130,
'M4x10 Cap Screw:16');
#773=NEXT_ASSEMBLY_USAGE_OCCURRENCE('M4x10 Cap Screw:17',
'M4x10 Cap Screw:17','M4x10 Cap Screw:17',#63106,#63130,
'M4x10 Cap Screw:17');
#774=NEXT_ASSEMBLY_USAGE_OCCURRENCE('mm bearing cap (4):1',
'mm bearing cap (4):1','mm bearing cap (4):1',#63106,#63114,
'mm bearing cap (4):1');
#775=NEXT_ASSEMBLY_USAGE_OCCURRENCE('mm bearing cap (5):1',
'mm bearing cap (5):1','mm bearing cap (5):1',#63106,#63115,
'mm bearing cap (5):1');
#776=NEXT_ASSEMBLY_USAGE_OCCURRENCE('mm bearing cap (6):1',
'mm bearing cap (6):1','mm bearing cap (6):1',#63106,#63116,
'mm bearing cap (6):1');
#777=NEXT_ASSEMBLY_USAGE_OCCURRENCE('mm bearing cap (7):1',
'mm bearing cap (7):1','mm bearing cap (7):1',#63106,#63117,
'mm bearing cap (7):1');
#778=NEXT_ASSEMBLY_USAGE_OCCURRENCE(
'Sealed Ball Bearing - 12 x 32 x 10 mm:3',
'Sealed Ball Bearing - 12 x 32 x 10 mm:3',
'Sealed Ball Bearing - 12 x 32 x 10 mm:3',#63106,#63118,
'Sealed Ball Bearing - 12 x 32 x 10 mm:3');
#779=NEXT_ASSEMBLY_USAGE_OCCURRENCE('M4x10 Cap Screw:18',
'M4x10 Cap Screw:18','M4x10 Cap Screw:18',#63106,#63130,
'M4x10 Cap Screw:18');
#780=NEXT_ASSEMBLY_USAGE_OCCURRENCE('M4x10 Cap Screw:19',
'M4x10 Cap Screw:19','M4x10 Cap Screw:19',#63106,#63130,
'M4x10 Cap Screw:19');
#781=NEXT_ASSEMBLY_USAGE_OCCURRENCE('M4x10 Cap Screw:20',
'M4x10 Cap Screw:20','M4x10 Cap Screw:20',#63106,#63130,
'M4x10 Cap Screw:20');
#782=NEXT_ASSEMBLY_USAGE_OCCURRENCE('M4x10 Cap Screw:21',
'M4x10 Cap Screw:21','M4x10 Cap Screw:21',#63106,#63130,
'M4x10 Cap Screw:21');
#783=NEXT_ASSEMBLY_USAGE_OCCURRENCE('M4x10 Cap Screw:22',
'M4x10 Cap Screw:22','M4x10 Cap Screw:22',#63106,#63130,
'M4x10 Cap Screw:22');
#784=NEXT_ASSEMBLY_USAGE_OCCURRENCE('M4x10 Cap Screw:23',
'M4x10 Cap Screw:23','M4x10 Cap Screw:23',#63106,#63130,
'M4x10 Cap Screw:23');
#785=NEXT_ASSEMBLY_USAGE_OCCURRENCE('M4x10 Cap Screw:24',
'M4x10 Cap Screw:24','M4x10 Cap Screw:24',#63106,#63130,
'M4x10 Cap Screw:24');
#786=NEXT_ASSEMBLY_USAGE_OCCURRENCE('M4x10 Cap Screw:25',
'M4x10 Cap Screw:25','M4x10 Cap Screw:25',#63106,#63130,
'M4x10 Cap Screw:25');
#787=NEXT_ASSEMBLY_USAGE_OCCURRENCE(
'Sealed Ball Bearing - 20 x 47 x 14 mm:3',
'Sealed Ball Bearing - 20 x 47 x 14 mm:3',
'Sealed Ball Bearing - 20 x 47 x 14 mm:3',#63106,#63124,
'Sealed Ball Bearing - 20 x 47 x 14 mm:3');
#788=NEXT_ASSEMBLY_USAGE_OCCURRENCE('M4x10 Cap Screw:26',
'M4x10 Cap Screw:26','M4x10 Cap Screw:26',#63106,#63130,
'M4x10 Cap Screw:26');
#789=NEXT_ASSEMBLY_USAGE_OCCURRENCE('M4x10 Cap Screw:27',
'M4x10 Cap Screw:27','M4x10 Cap Screw:27',#63106,#63130,
'M4x10 Cap Screw:27');
#790=NEXT_ASSEMBLY_USAGE_OCCURRENCE('M4x10 Cap Screw:28',
'M4x10 Cap Screw:28','M4x10 Cap Screw:28',#63106,#63130,
'M4x10 Cap Screw:28');
#791=NEXT_ASSEMBLY_USAGE_OCCURRENCE('M4x10 Cap Screw:29',
'M4x10 Cap Screw:29','M4x10 Cap Screw:29',#63106,#63130,
'M4x10 Cap Screw:29');
#792=NEXT_ASSEMBLY_USAGE_OCCURRENCE('M4x10 Cap Screw:30',
'M4x10 Cap Screw:30','M4x10 Cap Screw:30',#63106,#63130,
'M4x10 Cap Screw:30');
#793=NEXT_ASSEMBLY_USAGE_OCCURRENCE('M4x10 Cap Screw:31',
'M4x10 Cap Screw:31','M4x10 Cap Screw:31',#63106,#63130,
'M4x10 Cap Screw:31');
#794=NEXT_ASSEMBLY_USAGE_OCCURRENCE('M4x10 Cap Screw:32',
'M4x10 Cap Screw:32','M4x10 Cap Screw:32',#63106,#63130,
'M4x10 Cap Screw:32');
#795=NEXT_ASSEMBLY_USAGE_OCCURRENCE('M4x10 Cap Screw:33',
'M4x10 Cap Screw:33','M4x10 Cap Screw:33',#63106,#63130,
'M4x10 Cap Screw:33');
#796=NEXT_ASSEMBLY_USAGE_OCCURRENCE('Output dial:1','Output dial:1',
'Output dial:1',#63106,#63131,'Output dial:1');
#797=NEXT_ASSEMBLY_USAGE_OCCURRENCE('Dial post:1','Dial post:1',
'Dial post:1',#63106,#63132,'Dial post:1');
#798=NEXT_ASSEMBLY_USAGE_OCCURRENCE('Dial post (1):1','Dial post (1):1',
'Dial post (1):1',#63106,#63133,'Dial post (1):1');
#799=NEXT_ASSEMBLY_USAGE_OCCURRENCE('Foot strip:1','Foot strip:1',
'Foot strip:1',#63106,#63134,'Foot strip:1');
#800=NEXT_ASSEMBLY_USAGE_OCCURRENCE('Foot strip (1):1',
'Foot strip (1):1','Foot strip (1):1',#63106,#63135,'Foot strip (1):1');
#801=NEXT_ASSEMBLY_USAGE_OCCURRENCE('Cap Screw - M4x16:6',
'Cap Screw - M4x16:6','Cap Screw - M4x16:6',#63106,#63175,
'Cap Screw - M4x16:6');
#802=NEXT_ASSEMBLY_USAGE_OCCURRENCE('M4x30 post bolt:2',
'M4x30 post bolt:2','M4x30 post bolt:2',#63106,#63136,
'M4x30 post bolt:2');
#803=NEXT_ASSEMBLY_USAGE_OCCURRENCE('Cap Screw - M4x16:7',
'Cap Screw - M4x16:7','Cap Screw - M4x16:7',#63106,#63175,
'Cap Screw - M4x16:7');
#804=NEXT_ASSEMBLY_USAGE_OCCURRENCE('M4x30 post bolt:3',
'M4x30 post bolt:3','M4x30 post bolt:3',#63106,#63136,
'M4x30 post bolt:3');
#805=NEXT_ASSEMBLY_USAGE_OCCURRENCE('Shaft 1:1','Shaft 1:1','Shaft 1:1',
#63137,#63138,'Shaft 1:1');
#806=NEXT_ASSEMBLY_USAGE_OCCURRENCE('mm gear spacer:1',
'mm gear spacer:1','mm gear spacer:1',#63137,#63139,'mm gear spacer:1');
#807=NEXT_ASSEMBLY_USAGE_OCCURRENCE('mm rear spacer:1',
'mm rear spacer:1','mm rear spacer:1',#63137,#63140,'mm rear spacer:1');
#808=NEXT_ASSEMBLY_USAGE_OCCURRENCE('mm rear collar:1',
'mm rear collar:1','mm rear collar:1',#63137,#63141,'mm rear collar:1');
#809=NEXT_ASSEMBLY_USAGE_OCCURRENCE('Crank arm:1','Crank arm:1',
'Crank arm:1',#63137,#63142,'Crank arm:1');
#810=NEXT_ASSEMBLY_USAGE_OCCURRENCE('Crank spacer:1','Crank spacer:1',
'Crank spacer:1',#63137,#63143,'Crank spacer:1');
#811=NEXT_ASSEMBLY_USAGE_OCCURRENCE('Crank spacer (1):1',
'Crank spacer (1):1','Crank spacer (1):1',#63137,#63144,
'Crank spacer (1):1');
#812=NEXT_ASSEMBLY_USAGE_OCCURRENCE('Crank keeper:1','Crank keeper:1',
'Crank keeper:1',#63137,#63145,'Crank keeper:1');
#813=NEXT_ASSEMBLY_USAGE_OCCURRENCE('Grip sleeve:1','Grip sleeve:1',
'Grip sleeve:1',#63137,#63146,'Grip sleeve:1');
#814=NEXT_ASSEMBLY_USAGE_OCCURRENCE('Socket Set Screw - M5x8:2',
'Socket Set Screw - M5x8:2','Socket Set Screw - M5x8:2',#63137,#63174,
'Socket Set Screw - M5x8:2');
#815=NEXT_ASSEMBLY_USAGE_OCCURRENCE(
'Spur Gear - Module 2, 20 Teeth, 12 mm Bore:2',
'Spur Gear - Module 2, 20 Teeth, 12 mm Bore:2',
'Spur Gear - Module 2, 20 Teeth, 12 mm Bore:2',#63137,#63161,
'Spur Gear - Module 2, 20 Teeth, 12 mm Bore:2');
#816=NEXT_ASSEMBLY_USAGE_OCCURRENCE('Key 4x4x14:2','Key 4x4x14:2',
'Key 4x4x14:2',#63137,#63162,'Key 4x4x14:2');
#817=NEXT_ASSEMBLY_USAGE_OCCURRENCE('Key 4x4x14:3','Key 4x4x14:3',
'Key 4x4x14:3',#63137,#63162,'Key 4x4x14:3');
#818=NEXT_ASSEMBLY_USAGE_OCCURRENCE('Cap Screw - M4x16:2',
'Cap Screw - M4x16:2','Cap Screw - M4x16:2',#63137,#63175,
'Cap Screw - M4x16:2');
#819=NEXT_ASSEMBLY_USAGE_OCCURRENCE('Flat Washer - M6:2',
'Flat Washer - M6:2','Flat Washer - M6:2',#63137,#63147,
'Flat Washer - M6:2');
#820=NEXT_ASSEMBLY_USAGE_OCCURRENCE('M6x30 handle bolt:2',
'M6x30 handle bolt:2','M6x30 handle bolt:2',#63137,#63148,
'M6x30 handle bolt:2');
#821=NEXT_ASSEMBLY_USAGE_OCCURRENCE('Shaft 2:1','Shaft 2:1','Shaft 2:1',
#63149,#63150,'Shaft 2:1');
#822=NEXT_ASSEMBLY_USAGE_OCCURRENCE('mm gear spacer (1):1',
'mm gear spacer (1):1','mm gear spacer (1):1',#63149,#63151,
'mm gear spacer (1):1');
#823=NEXT_ASSEMBLY_USAGE_OCCURRENCE('mm rear spacer (1):1',
'mm rear spacer (1):1','mm rear spacer (1):1',#63149,#63152,
'mm rear spacer (1):1');
#824=NEXT_ASSEMBLY_USAGE_OCCURRENCE('mm rear collar (1):1',
'mm rear collar (1):1','mm rear collar (1):1',#63149,#63153,
'mm rear collar (1):1');
#825=NEXT_ASSEMBLY_USAGE_OCCURRENCE('mm shaft keeper:1',
'mm shaft keeper:1','mm shaft keeper:1',#63149,#63154,
'mm shaft keeper:1');
#826=NEXT_ASSEMBLY_USAGE_OCCURRENCE('Socket Set Screw - M5x8:3',
'Socket Set Screw - M5x8:3','Socket Set Screw - M5x8:3',#63149,#63174,
'Socket Set Screw - M5x8:3');
#827=NEXT_ASSEMBLY_USAGE_OCCURRENCE(
'Spur Gear - Module 2, 40 Teeth, 20 mm Bore:2',
'Spur Gear - Module 2, 40 Teeth, 20 mm Bore:2',
'Spur Gear - Module 2, 40 Teeth, 20 mm Bore:2',#63149,#63172,
'Spur Gear - Module 2, 40 Teeth, 20 mm Bore:2');
#828=NEXT_ASSEMBLY_USAGE_OCCURRENCE('Key 6x6x20:2','Key 6x6x20:2',
'Key 6x6x20:2',#63149,#63173,'Key 6x6x20:2');
#829=NEXT_ASSEMBLY_USAGE_OCCURRENCE('Cap Screw - M4x16:3',
'Cap Screw - M4x16:3','Cap Screw - M4x16:3',#63149,#63175,
'Cap Screw - M4x16:3');
#830=NEXT_ASSEMBLY_USAGE_OCCURRENCE('Shaft 3:1','Shaft 3:1','Shaft 3:1',
#63155,#63156,'Shaft 3:1');
#831=NEXT_ASSEMBLY_USAGE_OCCURRENCE('mm gear spacer (2):1',
'mm gear spacer (2):1','mm gear spacer (2):1',#63155,#63157,
'mm gear spacer (2):1');
#832=NEXT_ASSEMBLY_USAGE_OCCURRENCE('mm rear spacer (2):1',
'mm rear spacer (2):1','mm rear spacer (2):1',#63155,#63158,
'mm rear spacer (2):1');
#833=NEXT_ASSEMBLY_USAGE_OCCURRENCE('mm rear collar (2):1',
'mm rear collar (2):1','mm rear collar (2):1',#63155,#63159,
'mm rear collar (2):1');
#834=NEXT_ASSEMBLY_USAGE_OCCURRENCE('mm shaft keeper (1):1',
'mm shaft keeper (1):1','mm shaft keeper (1):1',#63155,#63160,
'mm shaft keeper (1):1');
#835=NEXT_ASSEMBLY_USAGE_OCCURRENCE('Socket Set Screw - M5x8:4',
'Socket Set Screw - M5x8:4','Socket Set Screw - M5x8:4',#63155,#63174,
'Socket Set Screw - M5x8:4');
#836=NEXT_ASSEMBLY_USAGE_OCCURRENCE(
'Spur Gear - Module 2, 20 Teeth, 12 mm Bore:3',
'Spur Gear - Module 2, 20 Teeth, 12 mm Bore:3',
'Spur Gear - Module 2, 20 Teeth, 12 mm Bore:3',#63155,#63161,
'Spur Gear - Module 2, 20 Teeth, 12 mm Bore:3');
#837=NEXT_ASSEMBLY_USAGE_OCCURRENCE('Key 4x4x14:4','Key 4x4x14:4',
'Key 4x4x14:4',#63155,#63162,'Key 4x4x14:4');
#838=NEXT_ASSEMBLY_USAGE_OCCURRENCE('Cap Screw - M4x16:4',
'Cap Screw - M4x16:4','Cap Screw - M4x16:4',#63155,#63175,
'Cap Screw - M4x16:4');
#839=NEXT_ASSEMBLY_USAGE_OCCURRENCE('Shaft 4:1','Shaft 4:1','Shaft 4:1',
#63163,#63164,'Shaft 4:1');
#840=NEXT_ASSEMBLY_USAGE_OCCURRENCE('mm gear spacer (3):1',
'mm gear spacer (3):1','mm gear spacer (3):1',#63163,#63165,
'mm gear spacer (3):1');
#841=NEXT_ASSEMBLY_USAGE_OCCURRENCE('mm rear spacer (3):1',
'mm rear spacer (3):1','mm rear spacer (3):1',#63163,#63166,
'mm rear spacer (3):1');
#842=NEXT_ASSEMBLY_USAGE_OCCURRENCE('mm rear collar (3):1',
'mm rear collar (3):1','mm rear collar (3):1',#63163,#63167,
'mm rear collar (3):1');
#843=NEXT_ASSEMBLY_USAGE_OCCURRENCE('Dial rear spacer:1',
'Dial rear spacer:1','Dial rear spacer:1',#63163,#63168,
'Dial rear spacer:1');
#844=NEXT_ASSEMBLY_USAGE_OCCURRENCE('Dial front spacer:1',
'Dial front spacer:1','Dial front spacer:1',#63163,#63169,
'Dial front spacer:1');
#845=NEXT_ASSEMBLY_USAGE_OCCURRENCE('Pointer:1','Pointer:1','Pointer:1',
#63163,#63170,'Pointer:1');
#846=NEXT_ASSEMBLY_USAGE_OCCURRENCE('Output keeper:1','Output keeper:1',
'Output keeper:1',#63163,#63171,'Output keeper:1');
#847=NEXT_ASSEMBLY_USAGE_OCCURRENCE('Socket Set Screw - M5x8:5',
'Socket Set Screw - M5x8:5','Socket Set Screw - M5x8:5',#63163,#63174,
'Socket Set Screw - M5x8:5');
#848=NEXT_ASSEMBLY_USAGE_OCCURRENCE(
'Spur Gear - Module 2, 40 Teeth, 20 mm Bore:3',
'Spur Gear - Module 2, 40 Teeth, 20 mm Bore:3',
'Spur Gear - Module 2, 40 Teeth, 20 mm Bore:3',#63163,#63172,
'Spur Gear - Module 2, 40 Teeth, 20 mm Bore:3');
#849=NEXT_ASSEMBLY_USAGE_OCCURRENCE('Key 6x6x20:3','Key 6x6x20:3',
'Key 6x6x20:3',#63163,#63173,'Key 6x6x20:3');
#850=NEXT_ASSEMBLY_USAGE_OCCURRENCE('Socket Set Screw - M5x8:6',
'Socket Set Screw - M5x8:6','Socket Set Screw - M5x8:6',#63163,#63174,
'Socket Set Screw - M5x8:6');
#851=NEXT_ASSEMBLY_USAGE_OCCURRENCE('Cap Screw - M4x16:5',
'Cap Screw - M4x16:5','Cap Screw - M4x16:5',#63163,#63175,
'Cap Screw - M4x16:5');
#852=NEXT_ASSEMBLY_USAGE_OCCURRENCE('Revolving grip:1',
'Revolving grip:1','Revolving grip:1',#63176,#63177,'Revolving grip:1');
#853=NEXT_ASSEMBLY_USAGE_OCCURRENCE('Bearing plate and dial:1',
'Bearing plate and dial:1','Bearing plate and dial:1',#63105,#63106,
'Bearing plate and dial:1');
#854=NEXT_ASSEMBLY_USAGE_OCCURRENCE('Rotor 1:1','Rotor 1:1','Rotor 1:1',
#63105,#63137,'Rotor 1:1');
#855=NEXT_ASSEMBLY_USAGE_OCCURRENCE('Rotor 2:1','Rotor 2:1','Rotor 2:1',
#63105,#63149,'Rotor 2:1');
#856=NEXT_ASSEMBLY_USAGE_OCCURRENCE('Rotor 3:1','Rotor 3:1','Rotor 3:1',
#63105,#63155,'Rotor 3:1');
#857=NEXT_ASSEMBLY_USAGE_OCCURRENCE('Rotor 4:1','Rotor 4:1','Rotor 4:1',
#63105,#63163,'Rotor 4:1');
#858=NEXT_ASSEMBLY_USAGE_OCCURRENCE('Revolving grip (1):1',
'Revolving grip (1):1','Revolving grip (1):1',#63105,#63176,
'Revolving grip (1):1');
#859=B_SPLINE_CURVE_WITH_KNOTS('',3,(#24083,#24084,#24085,#24086,#24087,
#24088,#24089,#24090,#24091,#24092,#24093,#24094,#24095,#24096,#24097,#24098,
#24099,#24100,#24101,#24102,#24103,#24104),.UNSPECIFIED.,.F.,.F.,(4,2,2,
2,2,2,2,2,2,2,4),(0.0591825211272536,0.157966726598481,0.236950089897721,
0.315933453196962,0.391576304923761,0.46721915665056,0.54286200837736,0.618504860104159,
0.697488223403399,0.77647158670264,0.875255792173867),.UNSPECIFIED.);
#860=B_SPLINE_CURVE_WITH_KNOTS('',3,(#24108,#24109,#24110,#24111,#24112,
#24113,#24114,#24115,#24116,#24117,#24118,#24119,#24120,#24121,#24122,#24123,
#24124,#24125,#24126,#24127,#24128,#24129),.UNSPECIFIED.,.F.,.F.,(4,2,2,
2,2,2,2,2,2,2,4),(0.0581119756758434,0.106553146291161,0.213106292582322,
0.30849933801665,0.386091982889075,0.4636846277615,0.541277272633925,0.61886991750635,
0.714262962940678,0.820816109231839,0.869257279847157),.UNSPECIFIED.);
#861=B_SPLINE_CURVE_WITH_KNOTS('',3,(#24135,#24136,#24137,#24138,#24139,
#24140,#24141,#24142,#24143,#24144,#24145,#24146,#24147,#24148,#24149,#24150,
#24151,#24152,#24153,#24154,#24155,#24156),.UNSPECIFIED.,.F.,.F.,(4,2,2,
2,2,2,2,2,2,2,4),(0.0581119756758434,0.106553146291161,0.213106292582322,
0.30849933801665,0.386091982889075,0.4636846277615,0.541277272633925,0.61886991750635,
0.714262962940679,0.820816109231839,0.869257279847157),.UNSPECIFIED.);
#862=B_SPLINE_CURVE_WITH_KNOTS('',3,(#24160,#24161,#24162,#24163,#24164,
#24165,#24166,#24167,#24168,#24169,#24170,#24171,#24172,#24173,#24174,#24175,
#24176,#24177,#24178,#24179,#24180,#24181),.UNSPECIFIED.,.F.,.F.,(4,2,2,
2,2,2,2,2,2,2,4),(0.0581119756758433,0.106553146291161,0.213106292582322,
0.308499338016649,0.386091982889075,0.4636846277615,0.541277272633925,0.61886991750635,
0.714262962940678,0.820816109231839,0.869257279847157),.UNSPECIFIED.);
#863=B_SPLINE_CURVE_WITH_KNOTS('',3,(#24190,#24191,#24192,#24193,#24194,
#24195,#24196,#24197,#24198,#24199,#24200,#24201,#24202,#24203,#24204,#24205,
#24206,#24207,#24208,#24209,#24210,#24211),.UNSPECIFIED.,.F.,.F.,(4,2,2,
2,2,2,2,2,2,2,4),(0.0581119756758433,0.106553146291161,0.213106292582322,
0.30849933801665,0.386091982889075,0.4636846277615,0.541277272633925,0.61886991750635,
0.714262962940678,0.820816109231839,0.869257279847157),.UNSPECIFIED.);
#864=B_SPLINE_CURVE_WITH_KNOTS('',3,(#24215,#24216,#24217,#24218,#24219,
#24220,#24221,#24222,#24223,#24224,#24225,#24226,#24227,#24228,#24229,#24230,
#24231,#24232,#24233,#24234,#24235,#24236),.UNSPECIFIED.,.F.,.F.,(4,2,2,
2,2,2,2,2,2,2,4),(0.0581119756758434,0.106553146291161,0.213106292582322,
0.30849933801665,0.386091982889075,0.4636846277615,0.541277272633925,0.61886991750635,
0.714262962940678,0.820816109231839,0.869257279847157),.UNSPECIFIED.);
#865=B_SPLINE_CURVE_WITH_KNOTS('',3,(#24240,#24241,#24242,#24243,#24244,
#24245,#24246,#24247,#24248,#24249,#24250,#24251,#24252,#24253,#24254,#24255,
#24256,#24257,#24258,#24259,#24260,#24261),.UNSPECIFIED.,.F.,.F.,(4,2,2,
2,2,2,2,2,2,2,4),(0.0581119756758434,0.106553146291161,0.213106292582322,
0.30849933801665,0.386091982889075,0.4636846277615,0.541277272633925,0.61886991750635,
0.714262962940678,0.820816109231839,0.869257279847157),.UNSPECIFIED.);
#866=B_SPLINE_CURVE_WITH_KNOTS('',3,(#24265,#24266,#24267,#24268,#24269,
#24270,#24271,#24272,#24273,#24274,#24275,#24276,#24277,#24278,#24279,#24280,
#24281,#24282,#24283,#24284,#24285,#24286),.UNSPECIFIED.,.F.,.F.,(4,2,2,
2,2,2,2,2,2,2,4),(0.0581119756758433,0.106553146291161,0.213106292582322,
0.30849933801665,0.386091982889075,0.4636846277615,0.541277272633925,0.61886991750635,
0.714262962940678,0.820816109231839,0.869257279847157),.UNSPECIFIED.);
#867=B_SPLINE_CURVE_WITH_KNOTS('',3,(#24294,#24295,#24296,#24297,#24298,
#24299,#24300,#24301,#24302,#24303,#24304,#24305,#24306,#24307,#24308,#24309,
#24310,#24311,#24312,#24313,#24314,#24315),.UNSPECIFIED.,.F.,.F.,(4,2,2,
2,2,2,2,2,2,2,4),(0.0591825211272536,0.157966726598481,0.236950089897721,
0.315933453196962,0.391576304923761,0.467219156650561,0.54286200837736,
0.618504860104159,0.697488223403399,0.77647158670264,0.875255792173867),
 .UNSPECIFIED.);
#868=B_SPLINE_CURVE_WITH_KNOTS('',3,(#24323,#24324,#24325,#24326,#24327,
#24328,#24329,#24330,#24331,#24332,#24333,#24334,#24335,#24336,#24337,#24338,
#24339,#24340,#24341,#24342,#24343,#24344),.UNSPECIFIED.,.F.,.F.,(4,2,2,
2,2,2,2,2,2,2,4),(0.0591825211272536,0.157966726598481,0.236950089897722,
0.315933453196962,0.391576304923761,0.467219156650561,0.54286200837736,
0.618504860104159,0.697488223403399,0.77647158670264,0.875255792173867),
 .UNSPECIFIED.);
#869=B_SPLINE_CURVE_WITH_KNOTS('',3,(#24354,#24355,#24356,#24357,#24358,
#24359,#24360,#24361,#24362,#24363,#24364,#24365,#24366,#24367,#24368,#24369,
#24370,#24371,#24372,#24373,#24374,#24375),.UNSPECIFIED.,.F.,.F.,(4,2,2,
2,2,2,2,2,2,2,4),(0.0591825211272536,0.157966726598481,0.236950089897721,
0.315933453196962,0.391576304923761,0.46721915665056,0.54286200837736,0.618504860104159,
0.697488223403399,0.77647158670264,0.875255792173867),.UNSPECIFIED.);
#870=B_SPLINE_CURVE_WITH_KNOTS('',3,(#24383,#24384,#24385,#24386,#24387,
#24388,#24389,#24390,#24391,#24392,#24393,#24394,#24395,#24396,#24397,#24398,
#24399,#24400,#24401,#24402,#24403,#24404),.UNSPECIFIED.,.F.,.F.,(4,2,2,
2,2,2,2,2,2,2,4),(0.0591825211272536,0.157966726598481,0.236950089897721,
0.315933453196962,0.391576304923761,0.46721915665056,0.542862008377359,
0.618504860104159,0.697488223403399,0.776471586702639,0.875255792173867),
 .UNSPECIFIED.);
#871=B_SPLINE_CURVE_WITH_KNOTS('',3,(#24412,#24413,#24414,#24415,#24416,
#24417,#24418,#24419,#24420,#24421,#24422,#24423,#24424,#24425,#24426,#24427,
#24428,#24429,#24430,#24431,#24432,#24433),.UNSPECIFIED.,.F.,.F.,(4,2,2,
2,2,2,2,2,2,2,4),(0.0591825211272536,0.157966726598481,0.236950089897721,
0.315933453196962,0.391576304923761,0.46721915665056,0.54286200837736,0.618504860104159,
0.697488223403399,0.77647158670264,0.875255792173867),.UNSPECIFIED.);
#872=B_SPLINE_CURVE_WITH_KNOTS('',3,(#24442,#24443,#24444,#24445,#24446,
#24447,#24448,#24449,#24450,#24451,#24452,#24453,#24454,#24455,#24456,#24457,
#24458,#24459,#24460,#24461,#24462,#24463),.UNSPECIFIED.,.F.,.F.,(4,2,2,
2,2,2,2,2,2,2,4),(0.0591825211272536,0.157966726598481,0.236950089897721,
0.315933453196962,0.391576304923761,0.46721915665056,0.542862008377359,
0.618504860104159,0.697488223403399,0.776471586702639,0.875255792173867),
 .UNSPECIFIED.);
#873=B_SPLINE_CURVE_WITH_KNOTS('',3,(#24613,#24614,#24615,#24616,#24617,
#24618,#24619,#24620,#24621,#24622,#24623,#24624,#24625,#24626,#24627,#24628,
#24629,#24630,#24631,#24632,#24633,#24634),.UNSPECIFIED.,.F.,.F.,(4,2,2,
2,2,2,2,2,2,2,4),(0.0789094028588958,0.210573405340968,0.315860108011452,
0.421146810681936,0.522142632548711,0.623138454415485,0.72413427628226,
0.825130098149035,0.930416800819519,1.03570350349,1.16736750597208),
 .UNSPECIFIED.);
#874=B_SPLINE_CURVE_WITH_KNOTS('',3,(#24638,#24639,#24640,#24641,#24642,
#24643,#24644,#24645,#24646,#24647,#24648,#24649,#24650,#24651,#24652,#24653,
#24654,#24655,#24656,#24657,#24658,#24659),.UNSPECIFIED.,.F.,.F.,(4,2,2,
2,2,2,2,2,2,2,4),(0.0774793363974613,0.142088896491891,0.284177792983782,
0.411119756996526,0.514392970548519,0.617666184100513,0.720939397652506,
0.8242126112045,0.951154575217244,1.09324347170913,1.15785303180356),
 .UNSPECIFIED.);
#875=B_SPLINE_CURVE_WITH_KNOTS('',3,(#24665,#24666,#24667,#24668,#24669,
#24670,#24671,#24672,#24673,#24674,#24675,#24676,#24677,#24678,#24679,#24680,
#24681,#24682,#24683,#24684,#24685,#24686),.UNSPECIFIED.,.F.,.F.,(4,2,2,
2,2,2,2,2,2,2,4),(0.0774793363974613,0.142088896491891,0.284177792983782,
0.411119756996525,0.514392970548519,0.617666184100513,0.720939397652506,
0.8242126112045,0.951154575217243,1.09324347170913,1.15785303180356),
 .UNSPECIFIED.);
#876=B_SPLINE_CURVE_WITH_KNOTS('',3,(#24690,#24691,#24692,#24693,#24694,
#24695,#24696,#24697,#24698,#24699,#24700,#24701,#24702,#24703,#24704,#24705,
#24706,#24707,#24708,#24709,#24710,#24711),.UNSPECIFIED.,.F.,.F.,(4,2,2,
2,2,2,2,2,2,2,4),(0.0774793363974614,0.142088896491891,0.284177792983781,
0.411119756996525,0.514392970548519,0.617666184100512,0.720939397652506,
0.824212611204499,0.951154575217243,1.09324347170913,1.15785303180356),
 .UNSPECIFIED.);
#877=B_SPLINE_CURVE_WITH_KNOTS('',3,(#24715,#24716,#24717,#24718,#24719,
#24720,#24721,#24722,#24723,#24724,#24725,#24726),.UNSPECIFIED.,.F.,.F.,
(4,2,2,2,2,4),(0.0774793363974613,0.142088896491891,0.284177792983781,0.411119756996525,
0.514392970548519,0.617666184100512),.UNSPECIFIED.);
#878=B_SPLINE_CURVE_WITH_KNOTS('',3,(#24731,#24732,#24733,#24734,#24735,
#24736,#24737,#24738,#24739,#24740,#24741,#24742),.UNSPECIFIED.,.F.,.F.,
(4,2,2,2,2,4),(0.617666184100512,0.720939397652506,0.824212611204499,0.951154575217243,
1.09324347170913,1.15785303180356),.UNSPECIFIED.);
#879=B_SPLINE_CURVE_WITH_KNOTS('',3,(#24746,#24747,#24748,#24749,#24750,
#24751,#24752,#24753,#24754,#24755,#24756,#24757,#24758,#24759,#24760,#24761,
#24762,#24763,#24764,#24765,#24766,#24767),.UNSPECIFIED.,.F.,.F.,(4,2,2,
2,2,2,2,2,2,2,4),(0.0774793363974613,0.142088896491891,0.284177792983782,
0.411119756996526,0.514392970548519,0.617666184100513,0.720939397652507,
0.8242126112045,0.951154575217245,1.09324347170914,1.15785303180356),
 .UNSPECIFIED.);
#880=B_SPLINE_CURVE_WITH_KNOTS('',3,(#24771,#24772,#24773,#24774,#24775,
#24776,#24777,#24778,#24779,#24780,#24781,#24782,#24783,#24784,#24785,#24786,
#24787,#24788,#24789,#24790,#24791,#24792),.UNSPECIFIED.,.F.,.F.,(4,2,2,
2,2,2,2,2,2,2,4),(0.0774793363974613,0.142088896491891,0.284177792983782,
0.411119756996526,0.514392970548519,0.617666184100513,0.720939397652506,
0.824212611204499,0.951154575217243,1.09324347170913,1.15785303180356),
 .UNSPECIFIED.);
#881=B_SPLINE_CURVE_WITH_KNOTS('',3,(#24796,#24797,#24798,#24799,#24800,
#24801,#24802,#24803,#24804,#24805,#24806,#24807,#24808,#24809,#24810,#24811,
#24812,#24813,#24814,#24815,#24816,#24817),.UNSPECIFIED.,.F.,.F.,(4,2,2,
2,2,2,2,2,2,2,4),(0.0774793363974613,0.142088896491891,0.284177792983782,
0.411119756996526,0.514392970548519,0.617666184100513,0.720939397652506,
0.8242126112045,0.951154575217244,1.09324347170913,1.15785303180356),
 .UNSPECIFIED.);
#882=B_SPLINE_CURVE_WITH_KNOTS('',3,(#24821,#24822,#24823,#24824,#24825,
#24826,#24827,#24828,#24829,#24830,#24831,#24832,#24833,#24834,#24835,#24836,
#24837,#24838,#24839,#24840,#24841,#24842),.UNSPECIFIED.,.F.,.F.,(4,2,2,
2,2,2,2,2,2,2,4),(0.0774793363974613,0.142088896491891,0.284177792983782,
0.411119756996526,0.514392970548519,0.617666184100513,0.720939397652506,
0.8242126112045,0.951154575217243,1.09324347170913,1.15785303180356),
 .UNSPECIFIED.);
#883=B_SPLINE_CURVE_WITH_KNOTS('',3,(#24850,#24851,#24852,#24853,#24854,
#24855,#24856,#24857,#24858,#24859,#24860,#24861,#24862,#24863,#24864,#24865,
#24866,#24867,#24868,#24869,#24870,#24871),.UNSPECIFIED.,.F.,.F.,(4,2,2,
2,2,2,2,2,2,2,4),(0.0789094028588958,0.210573405340968,0.315860108011452,
0.421146810681936,0.522142632548711,0.623138454415485,0.72413427628226,
0.825130098149035,0.930416800819519,1.03570350349,1.16736750597208),
 .UNSPECIFIED.);
#884=B_SPLINE_CURVE_WITH_KNOTS('',3,(#24879,#24880,#24881,#24882,#24883,
#24884,#24885,#24886,#24887,#24888,#24889,#24890,#24891,#24892,#24893,#24894,
#24895,#24896,#24897,#24898,#24899,#24900),.UNSPECIFIED.,.F.,.F.,(4,2,2,
2,2,2,2,2,2,2,4),(0.0789094028588958,0.210573405340969,0.315860108011453,
0.421146810681937,0.522142632548712,0.623138454415486,0.724134276282261,
0.825130098149035,0.930416800819519,1.03570350349,1.16736750597208),
 .UNSPECIFIED.);
#885=B_SPLINE_CURVE_WITH_KNOTS('',3,(#24909,#24910,#24911,#24912,#24913,
#24914,#24915,#24916,#24917,#24918,#24919,#24920),.UNSPECIFIED.,.F.,.F.,
(4,2,2,2,2,4),(0.0789094028588958,0.210573405340968,0.315860108011452,0.421146810681937,
0.522142632548711,0.623138454415486),.UNSPECIFIED.);
#886=B_SPLINE_CURVE_WITH_KNOTS('',3,(#24922,#24923,#24924,#24925,#24926,
#24927,#24928,#24929,#24930,#24931,#24932,#24933),.UNSPECIFIED.,.F.,.F.,
(4,2,2,2,2,4),(0.623138454415486,0.72413427628226,0.825130098149035,0.930416800819519,
1.03570350349,1.16736750597208),.UNSPECIFIED.);
#887=B_SPLINE_CURVE_WITH_KNOTS('',3,(#24940,#24941,#24942,#24943,#24944,
#24945,#24946,#24947,#24948,#24949,#24950,#24951,#24952,#24953,#24954,#24955,
#24956,#24957,#24958,#24959,#24960,#24961),.UNSPECIFIED.,.F.,.F.,(4,2,2,
2,2,2,2,2,2,2,4),(0.0789094028588958,0.210573405340968,0.315860108011452,
0.421146810681936,0.522142632548711,0.623138454415486,0.72413427628226,
0.825130098149035,0.930416800819519,1.03570350349,1.16736750597208),
 .UNSPECIFIED.);
#888=B_SPLINE_CURVE_WITH_KNOTS('',3,(#24969,#24970,#24971,#24972,#24973,
#24974,#24975,#24976,#24977,#24978,#24979,#24980,#24981,#24982,#24983,#24984,
#24985,#24986,#24987,#24988,#24989,#24990),.UNSPECIFIED.,.F.,.F.,(4,2,2,
2,2,2,2,2,2,2,4),(0.0789094028588957,0.210573405340968,0.315860108011452,
0.421146810681936,0.522142632548711,0.623138454415485,0.72413427628226,
0.825130098149035,0.930416800819519,1.03570350349,1.16736750597207),
 .UNSPECIFIED.);
#889=B_SPLINE_CURVE_WITH_KNOTS('',3,(#24998,#24999,#25000,#25001,#25002,
#25003,#25004,#25005,#25006,#25007,#25008,#25009,#25010,#25011,#25012,#25013,
#25014,#25015,#25016,#25017,#25018,#25019),.UNSPECIFIED.,.F.,.F.,(4,2,2,
2,2,2,2,2,2,2,4),(0.0789094028588958,0.210573405340968,0.315860108011452,
0.421146810681936,0.522142632548711,0.623138454415486,0.72413427628226,
0.825130098149035,0.930416800819519,1.03570350349,1.16736750597208),
 .UNSPECIFIED.);
#890=B_SPLINE_CURVE_WITH_KNOTS('',3,(#25028,#25029,#25030,#25031,#25032,
#25033,#25034,#25035,#25036,#25037,#25038,#25039,#25040,#25041,#25042,#25043,
#25044,#25045,#25046,#25047,#25048,#25049),.UNSPECIFIED.,.F.,.F.,(4,2,2,
2,2,2,2,2,2,2,4),(0.0789094028588958,0.210573405340968,0.315860108011452,
0.421146810681936,0.522142632548711,0.623138454415485,0.72413427628226,
0.825130098149035,0.930416800819519,1.03570350349,1.16736750597208),
 .UNSPECIFIED.);
#891=B_SPLINE_CURVE_WITH_KNOTS('',3,(#26102,#26103,#26104,#26105,#26106,
#26107,#26108,#26109,#26110,#26111),.UNSPECIFIED.,.F.,.F.,(4,2,2,2,4),(0.818088904349178,
0.878131747417164,0.957937926194035,1.03774410497091,1.09778694803889),
 .UNSPECIFIED.);
#892=B_SPLINE_CURVE_WITH_KNOTS('',3,(#26117,#26118,#26119,#26120,#26121,
#26122,#26123,#26124,#26125,#26126,#26127,#26128,#26129,#26130,#26131,#26132,
#26133,#26134),.UNSPECIFIED.,.F.,.F.,(4,2,2,2,2,2,2,2,4),(0.,0.0793616477694785,
0.158723295538957,0.238079516586307,0.317435737633656,0.396791958681006,
0.476148179728355,0.555509827497834,0.634871475267312),.UNSPECIFIED.);
#893=B_SPLINE_CURVE_WITH_KNOTS('',3,(#26135,#26136,#26137,#26138,#26139,
#26140,#26141,#26142,#26143,#26144,#26145,#26146,#26147,#26148,#26149,#26150,
#26151,#26152),.UNSPECIFIED.,.F.,.F.,(4,2,2,2,2,2,2,2,4),(0.634871475267312,
0.714233123036791,0.793594770806269,0.872950991853619,0.952307212900969,
1.03166343394832,1.11101965499567,1.19038130276515,1.26974295053462),
 .UNSPECIFIED.);
#894=B_SPLINE_CURVE_WITH_KNOTS('',3,(#26155,#26156,#26157,#26158,#26159,
#26160,#26161,#26162,#26163,#26164),.UNSPECIFIED.,.F.,.F.,(4,2,2,2,4),(0.179463620219821,
0.239506463287807,0.319312642064678,0.399118820841549,0.459161663909536),
 .UNSPECIFIED.);
#895=B_SPLINE_CURVE_WITH_KNOTS('',3,(#26487,#26488,#26489,#26490,#26491,
#26492,#26493,#26494,#26495,#26496,#26497,#26498,#26499,#26500),
 .UNSPECIFIED.,.F.,.F.,(4,2,2,2,2,2,4),(0.75600573798703,0.793568827564647,
0.872922520054202,0.952276212543757,1.03162990503331,1.11098359752287,1.14854668710048),
 .UNSPECIFIED.);
#896=B_SPLINE_CURVE_WITH_KNOTS('',3,(#26506,#26507,#26508,#26509,#26510,
#26511,#26512,#26513,#26514,#26515,#26516,#26517,#26518,#26519,#26520,#26521,
#26522,#26523),.UNSPECIFIED.,.F.,.F.,(4,2,2,2,2,2,2,2,4),(0.,0.0792334805614372,
0.158466961122874,0.237699060165217,0.31693115920756,0.396163258249903,
0.475395357292246,0.554628837853683,0.63386231841512),.UNSPECIFIED.);
#897=B_SPLINE_CURVE_WITH_KNOTS('',3,(#26524,#26525,#26526,#26527,#26528,
#26529,#26530,#26531,#26532,#26533,#26534,#26535,#26536,#26537,#26538,#26539,
#26540,#26541),.UNSPECIFIED.,.F.,.F.,(4,2,2,2,2,2,2,2,4),(0.63386231841512,
0.713095798976557,0.792329279537994,0.871561378580337,0.95079347762268,
1.03002557666502,1.10925767570737,1.1884911562688,1.26772463683024),
 .UNSPECIFIED.);
#898=B_SPLINE_CURVE_WITH_KNOTS('',3,(#26544,#26545,#26546,#26547,#26548,
#26549,#26550,#26551,#26552,#26553,#26554,#26555,#26556,#26557),
 .UNSPECIFIED.,.F.,.F.,(4,2,2,2,2,2,4),(0.121154929624526,0.158718019202142,
0.238071711691697,0.317425404181252,0.396779096670807,0.476132789160362,
0.513695878737979),.UNSPECIFIED.);
#899=B_SPLINE_CURVE_WITH_KNOTS('',3,(#26683,#26684,#26685,#26686,#26687,
#26688,#26689,#26690,#26691,#26692),.UNSPECIFIED.,.F.,.F.,(4,2,2,2,4),(0.81808890434921,
0.878131747417167,0.957937926194039,1.03774410497091,1.09778694803887),
 .UNSPECIFIED.);
#900=B_SPLINE_CURVE_WITH_KNOTS('',3,(#26698,#26699,#26700,#26701,#26702,
#26703,#26704,#26705,#26706,#26707,#26708,#26709,#26710,#26711,#26712,#26713,
#26714,#26715),.UNSPECIFIED.,.F.,.F.,(4,2,2,2,2,2,2,2,4),(0.,0.0793616477694788,
0.158723295538958,0.238079516586307,0.317435737633657,0.396791958681007,
0.476148179728357,0.555509827497836,0.634871475267315),.UNSPECIFIED.);
#901=B_SPLINE_CURVE_WITH_KNOTS('',3,(#26716,#26717,#26718,#26719,#26720,
#26721,#26722,#26723,#26724,#26725,#26726,#26727,#26728,#26729,#26730,#26731,
#26732,#26733),.UNSPECIFIED.,.F.,.F.,(4,2,2,2,2,2,2,2,4),(0.634871475267315,
0.714233123036793,0.793594770806272,0.872950991853622,0.952307212900972,
1.03166343394832,1.11101965499567,1.19038130276515,1.26974295053463),
 .UNSPECIFIED.);
#902=B_SPLINE_CURVE_WITH_KNOTS('',3,(#26736,#26737,#26738,#26739,#26740,
#26741,#26742,#26743,#26744,#26745),.UNSPECIFIED.,.F.,.F.,(4,2,2,2,4),(0.17946362021985,
0.239506463287808,0.31931264206468,0.399118820841551,0.459161663909509),
 .UNSPECIFIED.);
#903=B_SPLINE_CURVE_WITH_KNOTS('',3,(#38516,#38517,#38518,#38519,#38520,
#38521,#38522,#38523,#38524,#38525,#38526,#38527,#38528,#38529),
 .UNSPECIFIED.,.F.,.F.,(4,2,2,2,2,2,4),(0.756005737987044,0.793568827564651,
0.872922520054207,0.952276212543762,1.03162990503332,1.11098359752287,1.14854668710048),
 .UNSPECIFIED.);
#904=B_SPLINE_CURVE_WITH_KNOTS('',3,(#38535,#38536,#38537,#38538,#38539,
#38540,#38541,#38542,#38543,#38544,#38545,#38546,#38547,#38548,#38549,#38550,
#38551,#38552),.UNSPECIFIED.,.F.,.F.,(4,2,2,2,2,2,2,2,4),(0.,0.0792334805614372,
0.158466961122874,0.237699060165218,0.316931159207562,0.396163258249906,
0.47539535729225,0.554628837853687,0.633862318415124),.UNSPECIFIED.);
#905=B_SPLINE_CURVE_WITH_KNOTS('',3,(#38553,#38554,#38555,#38556,#38557,
#38558,#38559,#38560,#38561,#38562,#38563,#38564,#38565,#38566,#38567,#38568,
#38569,#38570),.UNSPECIFIED.,.F.,.F.,(4,2,2,2,2,2,2,2,4),(0.633862318415124,
0.713095798976561,0.792329279537998,0.871561378580342,0.950793477622686,
1.03002557666503,1.10925767570737,1.18849115626881,1.26772463683025),
 .UNSPECIFIED.);
#906=B_SPLINE_CURVE_WITH_KNOTS('',3,(#38573,#38574,#38575,#38576,#38577,
#38578,#38579,#38580,#38581,#38582,#38583,#38584,#38585,#38586),
 .UNSPECIFIED.,.F.,.F.,(4,2,2,2,2,2,4),(0.121154929624534,0.158718019202142,
0.238071711691698,0.317425404181254,0.39677909667081,0.476132789160366,
0.513695878737972),.UNSPECIFIED.);
#907=B_SPLINE_CURVE_WITH_KNOTS('',3,(#38641,#38642,#38643,#38644,#38645,
#38646,#38647,#38648,#38649,#38650),.UNSPECIFIED.,.F.,.F.,(4,2,2,2,4),(0.803821788694094,
0.872950991853624,0.952307212900975,1.03166343394833,1.10079263710785),
 .UNSPECIFIED.);
#908=B_SPLINE_CURVE_WITH_KNOTS('',3,(#38656,#38657,#38658,#38659,#38660,
#38661,#38662,#38663,#38664,#38665,#38666,#38667,#38668,#38669,#38670,#38671,
#38672,#38673),.UNSPECIFIED.,.F.,.F.,(4,2,2,2,2,2,2,2,4),(0.,0.0792165807733629,
0.158433161546726,0.237648697074571,0.316864232602417,0.396079768130262,
0.475295303658107,0.55451188443147,0.633728465204833),.UNSPECIFIED.);
#909=B_SPLINE_CURVE_WITH_KNOTS('',3,(#38674,#38675,#38676,#38677,#38678,
#38679,#38680,#38681,#38682,#38683,#38684,#38685,#38686,#38687,#38688,#38689,
#38690,#38691),.UNSPECIFIED.,.F.,.F.,(4,2,2,2,2,2,2,2,4),(0.633728465204833,
0.712945045978196,0.792161626751559,0.871377162279404,0.95059269780725,
1.0298082333351,1.10902376886294,1.1882403496363,1.26745693040967),
 .UNSPECIFIED.);
#910=B_SPLINE_CURVE_WITH_KNOTS('',3,(#38694,#38695,#38696,#38697,#38698,
#38699,#38700,#38701,#38702,#38703),.UNSPECIFIED.,.F.,.F.,(4,2,2,2,4),(0.168950313426782,
0.238079516586308,0.317435737633658,0.396791958681009,0.465921161840539),
 .UNSPECIFIED.);
#911=B_SPLINE_CURVE_WITH_KNOTS('',3,(#44768,#44769,#44770,#44771,#44772,
#44773),.UNSPECIFIED.,.F.,.F.,(4,2,4),(0.,1.,2.),.UNSPECIFIED.);
#912=B_SPLINE_CURVE_WITH_KNOTS('',3,(#44987,#44988,#44989,#44990,#44991,
#44992),.UNSPECIFIED.,.F.,.F.,(4,2,4),(0.,1.,2.),.UNSPECIFIED.);
#913=B_SPLINE_CURVE_WITH_KNOTS('',3,(#45070,#45071,#45072,#45073,#45074,
#45075),.UNSPECIFIED.,.F.,.F.,(4,2,4),(0.,1.,2.),.UNSPECIFIED.);
#914=B_SPLINE_CURVE_WITH_KNOTS('',3,(#45429,#45430,#45431,#45432,#45433,
#45434),.UNSPECIFIED.,.F.,.F.,(4,2,4),(0.,1.,2.),.UNSPECIFIED.);
#915=B_SPLINE_CURVE_WITH_KNOTS('',3,(#45512,#45513,#45514,#45515,#45516,
#45517),.UNSPECIFIED.,.F.,.F.,(4,2,4),(0.,1.,2.),.UNSPECIFIED.);
#916=B_SPLINE_CURVE_WITH_KNOTS('',3,(#45871,#45872,#45873,#45874,#45875,
#45876),.UNSPECIFIED.,.F.,.F.,(4,2,4),(0.,1.,2.),.UNSPECIFIED.);
#917=B_SPLINE_CURVE_WITH_KNOTS('',3,(#45954,#45955,#45956,#45957,#45958,
#45959),.UNSPECIFIED.,.F.,.F.,(4,2,4),(0.,1.,2.),.UNSPECIFIED.);
#918=B_SPLINE_CURVE_WITH_KNOTS('',3,(#46313,#46314,#46315,#46316,#46317,
#46318),.UNSPECIFIED.,.F.,.F.,(4,2,4),(0.,1.,2.),.UNSPECIFIED.);
#919=B_SPLINE_CURVE_WITH_KNOTS('',3,(#46396,#46397,#46398,#46399,#46400,
#46401),.UNSPECIFIED.,.F.,.F.,(4,2,4),(0.,1.,2.),.UNSPECIFIED.);
#920=B_SPLINE_CURVE_WITH_KNOTS('',3,(#46755,#46756,#46757,#46758,#46759,
#46760),.UNSPECIFIED.,.F.,.F.,(4,2,4),(0.,1.,2.),.UNSPECIFIED.);
#921=B_SPLINE_CURVE_WITH_KNOTS('',3,(#46838,#46839,#46840,#46841,#46842,
#46843),.UNSPECIFIED.,.F.,.F.,(4,2,4),(0.,1.,2.),.UNSPECIFIED.);
#922=B_SPLINE_CURVE_WITH_KNOTS('',3,(#47197,#47198,#47199,#47200,#47201,
#47202),.UNSPECIFIED.,.F.,.F.,(4,2,4),(0.,1.,2.),.UNSPECIFIED.);
#923=B_SPLINE_CURVE_WITH_KNOTS('',3,(#47280,#47281,#47282,#47283,#47284,
#47285),.UNSPECIFIED.,.F.,.F.,(4,2,4),(0.,1.,2.),.UNSPECIFIED.);
#924=B_SPLINE_CURVE_WITH_KNOTS('',3,(#47639,#47640,#47641,#47642,#47643,
#47644),.UNSPECIFIED.,.F.,.F.,(4,2,4),(0.,1.,2.),.UNSPECIFIED.);
#925=B_SPLINE_CURVE_WITH_KNOTS('',3,(#47722,#47723,#47724,#47725,#47726,
#47727),.UNSPECIFIED.,.F.,.F.,(4,2,4),(0.,1.,2.),.UNSPECIFIED.);
#926=B_SPLINE_CURVE_WITH_KNOTS('',3,(#48081,#48082,#48083,#48084,#48085,
#48086),.UNSPECIFIED.,.F.,.F.,(4,2,4),(0.,1.,2.),.UNSPECIFIED.);
#927=B_SPLINE_CURVE_WITH_KNOTS('',3,(#48164,#48165,#48166,#48167,#48168,
#48169),.UNSPECIFIED.,.F.,.F.,(4,2,4),(0.,1.,2.),.UNSPECIFIED.);
#928=B_SPLINE_CURVE_WITH_KNOTS('',3,(#48523,#48524,#48525,#48526,#48527,
#48528),.UNSPECIFIED.,.F.,.F.,(4,2,4),(0.,1.,2.),.UNSPECIFIED.);
#929=B_SPLINE_CURVE_WITH_KNOTS('',3,(#48606,#48607,#48608,#48609,#48610,
#48611),.UNSPECIFIED.,.F.,.F.,(4,2,4),(0.,1.,2.),.UNSPECIFIED.);
#930=B_SPLINE_CURVE_WITH_KNOTS('',3,(#48965,#48966,#48967,#48968,#48969,
#48970),.UNSPECIFIED.,.F.,.F.,(4,2,4),(0.,1.,2.),.UNSPECIFIED.);
#931=B_SPLINE_CURVE_WITH_KNOTS('',3,(#49048,#49049,#49050,#49051,#49052,
#49053),.UNSPECIFIED.,.F.,.F.,(4,2,4),(0.,1.,2.),.UNSPECIFIED.);
#932=B_SPLINE_CURVE_WITH_KNOTS('',3,(#49407,#49408,#49409,#49410,#49411,
#49412),.UNSPECIFIED.,.F.,.F.,(4,2,4),(0.,1.,2.),.UNSPECIFIED.);
#933=B_SPLINE_CURVE_WITH_KNOTS('',3,(#49490,#49491,#49492,#49493,#49494,
#49495),.UNSPECIFIED.,.F.,.F.,(4,2,4),(0.,1.,2.),.UNSPECIFIED.);
#934=B_SPLINE_CURVE_WITH_KNOTS('',3,(#49849,#49850,#49851,#49852,#49853,
#49854),.UNSPECIFIED.,.F.,.F.,(4,2,4),(0.,1.,2.),.UNSPECIFIED.);
#935=B_SPLINE_CURVE_WITH_KNOTS('',3,(#49932,#49933,#49934,#49935,#49936,
#49937),.UNSPECIFIED.,.F.,.F.,(4,2,4),(0.,1.,2.),.UNSPECIFIED.);
#936=B_SPLINE_CURVE_WITH_KNOTS('',3,(#50291,#50292,#50293,#50294,#50295,
#50296),.UNSPECIFIED.,.F.,.F.,(4,2,4),(0.,1.,2.),.UNSPECIFIED.);
#937=B_SPLINE_CURVE_WITH_KNOTS('',3,(#50374,#50375,#50376,#50377,#50378,
#50379),.UNSPECIFIED.,.F.,.F.,(4,2,4),(0.,1.,2.),.UNSPECIFIED.);
#938=B_SPLINE_CURVE_WITH_KNOTS('',3,(#50733,#50734,#50735,#50736,#50737,
#50738),.UNSPECIFIED.,.F.,.F.,(4,2,4),(0.,1.,2.),.UNSPECIFIED.);
#939=B_SPLINE_CURVE_WITH_KNOTS('',3,(#50816,#50817,#50818,#50819,#50820,
#50821),.UNSPECIFIED.,.F.,.F.,(4,2,4),(0.,1.,2.),.UNSPECIFIED.);
#940=B_SPLINE_CURVE_WITH_KNOTS('',3,(#51175,#51176,#51177,#51178,#51179,
#51180),.UNSPECIFIED.,.F.,.F.,(4,2,4),(0.,1.,2.),.UNSPECIFIED.);
#941=B_SPLINE_CURVE_WITH_KNOTS('',3,(#51258,#51259,#51260,#51261,#51262,
#51263),.UNSPECIFIED.,.F.,.F.,(4,2,4),(0.,1.,2.),.UNSPECIFIED.);
#942=B_SPLINE_CURVE_WITH_KNOTS('',3,(#51617,#51618,#51619,#51620,#51621,
#51622),.UNSPECIFIED.,.F.,.F.,(4,2,4),(0.,1.,2.),.UNSPECIFIED.);
#943=B_SPLINE_CURVE_WITH_KNOTS('',3,(#51700,#51701,#51702,#51703,#51704,
#51705),.UNSPECIFIED.,.F.,.F.,(4,2,4),(0.,1.,2.),.UNSPECIFIED.);
#944=B_SPLINE_CURVE_WITH_KNOTS('',3,(#52059,#52060,#52061,#52062,#52063,
#52064),.UNSPECIFIED.,.F.,.F.,(4,2,4),(0.,1.,2.),.UNSPECIFIED.);
#945=B_SPLINE_CURVE_WITH_KNOTS('',3,(#52142,#52143,#52144,#52145,#52146,
#52147),.UNSPECIFIED.,.F.,.F.,(4,2,4),(0.,1.,2.),.UNSPECIFIED.);
#946=B_SPLINE_CURVE_WITH_KNOTS('',3,(#52501,#52502,#52503,#52504,#52505,
#52506),.UNSPECIFIED.,.F.,.F.,(4,2,4),(0.,1.,2.),.UNSPECIFIED.);
#947=B_SPLINE_CURVE_WITH_KNOTS('',3,(#52584,#52585,#52586,#52587,#52588,
#52589),.UNSPECIFIED.,.F.,.F.,(4,2,4),(0.,1.,2.),.UNSPECIFIED.);
#948=B_SPLINE_CURVE_WITH_KNOTS('',3,(#52943,#52944,#52945,#52946,#52947,
#52948),.UNSPECIFIED.,.F.,.F.,(4,2,4),(0.,1.,2.),.UNSPECIFIED.);
#949=B_SPLINE_CURVE_WITH_KNOTS('',3,(#53026,#53027,#53028,#53029,#53030,
#53031),.UNSPECIFIED.,.F.,.F.,(4,2,4),(0.,1.,2.),.UNSPECIFIED.);
#950=B_SPLINE_CURVE_WITH_KNOTS('',3,(#53385,#53386,#53387,#53388,#53389,
#53390),.UNSPECIFIED.,.F.,.F.,(4,2,4),(0.,1.,2.),.UNSPECIFIED.);
#951=B_SPLINE_CURVE_WITH_KNOTS('',3,(#53468,#53469,#53470,#53471,#53472,
#53473),.UNSPECIFIED.,.F.,.F.,(4,2,4),(0.,1.,2.),.UNSPECIFIED.);
#952=B_SPLINE_CURVE_WITH_KNOTS('',3,(#53827,#53828,#53829,#53830,#53831,
#53832),.UNSPECIFIED.,.F.,.F.,(4,2,4),(0.,1.,2.),.UNSPECIFIED.);
#953=B_SPLINE_CURVE_WITH_KNOTS('',3,(#53910,#53911,#53912,#53913,#53914,
#53915),.UNSPECIFIED.,.F.,.F.,(4,2,4),(0.,1.,2.),.UNSPECIFIED.);
#954=B_SPLINE_CURVE_WITH_KNOTS('',3,(#54269,#54270,#54271,#54272,#54273,
#54274),.UNSPECIFIED.,.F.,.F.,(4,2,4),(0.,1.,2.),.UNSPECIFIED.);
#955=B_SPLINE_CURVE_WITH_KNOTS('',3,(#54352,#54353,#54354,#54355,#54356,
#54357),.UNSPECIFIED.,.F.,.F.,(4,2,4),(0.,1.,2.),.UNSPECIFIED.);
#956=B_SPLINE_CURVE_WITH_KNOTS('',3,(#54711,#54712,#54713,#54714,#54715,
#54716),.UNSPECIFIED.,.F.,.F.,(4,2,4),(0.,1.,2.),.UNSPECIFIED.);
#957=B_SPLINE_CURVE_WITH_KNOTS('',3,(#54794,#54795,#54796,#54797,#54798,
#54799),.UNSPECIFIED.,.F.,.F.,(4,2,4),(0.,1.,2.),.UNSPECIFIED.);
#958=B_SPLINE_CURVE_WITH_KNOTS('',3,(#55153,#55154,#55155,#55156,#55157,
#55158),.UNSPECIFIED.,.F.,.F.,(4,2,4),(0.,1.,2.),.UNSPECIFIED.);
#959=B_SPLINE_CURVE_WITH_KNOTS('',3,(#55236,#55237,#55238,#55239,#55240,
#55241),.UNSPECIFIED.,.F.,.F.,(4,2,4),(0.,1.,2.),.UNSPECIFIED.);
#960=B_SPLINE_CURVE_WITH_KNOTS('',3,(#55595,#55596,#55597,#55598,#55599,
#55600),.UNSPECIFIED.,.F.,.F.,(4,2,4),(0.,1.,2.),.UNSPECIFIED.);
#961=B_SPLINE_CURVE_WITH_KNOTS('',3,(#55678,#55679,#55680,#55681,#55682,
#55683),.UNSPECIFIED.,.F.,.F.,(4,2,4),(0.,1.,2.),.UNSPECIFIED.);
#962=B_SPLINE_CURVE_WITH_KNOTS('',3,(#56037,#56038,#56039,#56040,#56041,
#56042),.UNSPECIFIED.,.F.,.F.,(4,2,4),(0.,1.,2.),.UNSPECIFIED.);
#963=B_SPLINE_CURVE_WITH_KNOTS('',3,(#56120,#56121,#56122,#56123,#56124,
#56125),.UNSPECIFIED.,.F.,.F.,(4,2,4),(0.,1.,2.),.UNSPECIFIED.);
#964=B_SPLINE_CURVE_WITH_KNOTS('',3,(#56479,#56480,#56481,#56482,#56483,
#56484),.UNSPECIFIED.,.F.,.F.,(4,2,4),(0.,1.,2.),.UNSPECIFIED.);
#965=B_SPLINE_CURVE_WITH_KNOTS('',3,(#56562,#56563,#56564,#56565,#56566,
#56567),.UNSPECIFIED.,.F.,.F.,(4,2,4),(0.,1.,2.),.UNSPECIFIED.);
#966=B_SPLINE_CURVE_WITH_KNOTS('',3,(#56921,#56922,#56923,#56924,#56925,
#56926),.UNSPECIFIED.,.F.,.F.,(4,2,4),(0.,1.,2.),.UNSPECIFIED.);
#967=B_SPLINE_CURVE_WITH_KNOTS('',3,(#57004,#57005,#57006,#57007,#57008,
#57009),.UNSPECIFIED.,.F.,.F.,(4,2,4),(0.,1.,2.),.UNSPECIFIED.);
#968=B_SPLINE_CURVE_WITH_KNOTS('',3,(#57363,#57364,#57365,#57366,#57367,
#57368),.UNSPECIFIED.,.F.,.F.,(4,2,4),(0.,1.,2.),.UNSPECIFIED.);
#969=B_SPLINE_CURVE_WITH_KNOTS('',3,(#57446,#57447,#57448,#57449,#57450,
#57451),.UNSPECIFIED.,.F.,.F.,(4,2,4),(0.,1.,2.),.UNSPECIFIED.);
#970=B_SPLINE_CURVE_WITH_KNOTS('',3,(#57805,#57806,#57807,#57808,#57809,
#57810),.UNSPECIFIED.,.F.,.F.,(4,2,4),(0.,1.,2.),.UNSPECIFIED.);
#971=B_SPLINE_CURVE_WITH_KNOTS('',3,(#57888,#57889,#57890,#57891,#57892,
#57893),.UNSPECIFIED.,.F.,.F.,(4,2,4),(0.,1.,2.),.UNSPECIFIED.);
#972=B_SPLINE_CURVE_WITH_KNOTS('',3,(#58247,#58248,#58249,#58250,#58251,
#58252),.UNSPECIFIED.,.F.,.F.,(4,2,4),(0.,1.,2.),.UNSPECIFIED.);
#973=B_SPLINE_CURVE_WITH_KNOTS('',3,(#58330,#58331,#58332,#58333,#58334,
#58335),.UNSPECIFIED.,.F.,.F.,(4,2,4),(0.,1.,2.),.UNSPECIFIED.);
#974=B_SPLINE_CURVE_WITH_KNOTS('',3,(#58689,#58690,#58691,#58692,#58693,
#58694),.UNSPECIFIED.,.F.,.F.,(4,2,4),(0.,1.,2.),.UNSPECIFIED.);
#975=B_SPLINE_CURVE_WITH_KNOTS('',3,(#58772,#58773,#58774,#58775,#58776,
#58777),.UNSPECIFIED.,.F.,.F.,(4,2,4),(0.,1.,2.),.UNSPECIFIED.);
#976=B_SPLINE_CURVE_WITH_KNOTS('',3,(#59131,#59132,#59133,#59134,#59135,
#59136),.UNSPECIFIED.,.F.,.F.,(4,2,4),(0.,1.,2.),.UNSPECIFIED.);
#977=B_SPLINE_CURVE_WITH_KNOTS('',3,(#59214,#59215,#59216,#59217,#59218,
#59219),.UNSPECIFIED.,.F.,.F.,(4,2,4),(0.,1.,2.),.UNSPECIFIED.);
#978=B_SPLINE_CURVE_WITH_KNOTS('',3,(#59573,#59574,#59575,#59576,#59577,
#59578),.UNSPECIFIED.,.F.,.F.,(4,2,4),(0.,1.,2.),.UNSPECIFIED.);
#979=B_SPLINE_CURVE_WITH_KNOTS('',3,(#59656,#59657,#59658,#59659,#59660,
#59661),.UNSPECIFIED.,.F.,.F.,(4,2,4),(0.,1.,2.),.UNSPECIFIED.);
#980=B_SPLINE_CURVE_WITH_KNOTS('',3,(#60015,#60016,#60017,#60018,#60019,
#60020),.UNSPECIFIED.,.F.,.F.,(4,2,4),(0.,1.,2.),.UNSPECIFIED.);
#981=B_SPLINE_CURVE_WITH_KNOTS('',3,(#60098,#60099,#60100,#60101,#60102,
#60103),.UNSPECIFIED.,.F.,.F.,(4,2,4),(0.,1.,2.),.UNSPECIFIED.);
#982=B_SPLINE_CURVE_WITH_KNOTS('',3,(#60457,#60458,#60459,#60460,#60461,
#60462),.UNSPECIFIED.,.F.,.F.,(4,2,4),(0.,1.,2.),.UNSPECIFIED.);
#983=B_SPLINE_CURVE_WITH_KNOTS('',3,(#60540,#60541,#60542,#60543,#60544,
#60545),.UNSPECIFIED.,.F.,.F.,(4,2,4),(0.,1.,2.),.UNSPECIFIED.);
#984=B_SPLINE_CURVE_WITH_KNOTS('',3,(#60899,#60900,#60901,#60902,#60903,
#60904),.UNSPECIFIED.,.F.,.F.,(4,2,4),(0.,1.,2.),.UNSPECIFIED.);
#985=B_SPLINE_CURVE_WITH_KNOTS('',3,(#60982,#60983,#60984,#60985,#60986,
#60987),.UNSPECIFIED.,.F.,.F.,(4,2,4),(0.,1.,2.),.UNSPECIFIED.);
#986=B_SPLINE_CURVE_WITH_KNOTS('',3,(#61341,#61342,#61343,#61344,#61345,
#61346),.UNSPECIFIED.,.F.,.F.,(4,2,4),(0.,1.,2.),.UNSPECIFIED.);
#987=B_SPLINE_CURVE_WITH_KNOTS('',3,(#61424,#61425,#61426,#61427,#61428,
#61429),.UNSPECIFIED.,.F.,.F.,(4,2,4),(0.,1.,2.),.UNSPECIFIED.);
#988=B_SPLINE_CURVE_WITH_KNOTS('',3,(#61787,#61788,#61789,#61790,#61791,
#61792),.UNSPECIFIED.,.F.,.F.,(4,2,4),(0.,1.,2.),.UNSPECIFIED.);
#989=B_SPLINE_CURVE_WITH_KNOTS('',3,(#61866,#61867,#61868,#61869,#61870,
#61871),.UNSPECIFIED.,.F.,.F.,(4,2,4),(0.,1.,2.),.UNSPECIFIED.);
#990=B_SPLINE_CURVE_WITH_KNOTS('',3,(#62013,#62014,#62015,#62016,#62017,
#62018),.UNSPECIFIED.,.F.,.F.,(4,2,4),(0.,1.,2.),.UNSPECIFIED.);
#991=SPHERICAL_SURFACE('',#17526,0.29765);
#992=SPHERICAL_SURFACE('',#17528,0.29765);
#993=SPHERICAL_SURFACE('',#17530,0.29765);
#994=SPHERICAL_SURFACE('',#17532,0.29765);
#995=SPHERICAL_SURFACE('',#17534,0.29765);
#996=SPHERICAL_SURFACE('',#17536,0.29765);
#997=SPHERICAL_SURFACE('',#17538,0.29765);
#998=SPHERICAL_SURFACE('',#17541,0.309556);
#999=SPHERICAL_SURFACE('',#17557,0.309556);
#1000=SPHERICAL_SURFACE('',#17562,0.309556);
#1001=SPHERICAL_SURFACE('',#17568,0.309556);
#1002=SPHERICAL_SURFACE('',#17573,0.309556);
#1003=SPHERICAL_SURFACE('',#17578,0.309556);
#1004=SPHERICAL_SURFACE('',#17586,0.309556);
#1005=SPHERICAL_SURFACE('',#17654,0.3969);
#1006=SPHERICAL_SURFACE('',#17656,0.3969);
#1007=SPHERICAL_SURFACE('',#17658,0.3969);
#1008=SPHERICAL_SURFACE('',#17660,0.3969);
#1009=SPHERICAL_SURFACE('',#17662,0.3969);
#1010=SPHERICAL_SURFACE('',#17664,0.3969);
#1011=SPHERICAL_SURFACE('',#17666,0.3969);
#1012=SPHERICAL_SURFACE('',#17668,0.3969);
#1013=SPHERICAL_SURFACE('',#17671,0.412776);
#1014=SPHERICAL_SURFACE('',#17687,0.412776);
#1015=SPHERICAL_SURFACE('',#17692,0.412776);
#1016=SPHERICAL_SURFACE('',#17697,0.412776);
#1017=SPHERICAL_SURFACE('',#17702,0.412776);
#1018=SPHERICAL_SURFACE('',#17707,0.412776);
#1019=SPHERICAL_SURFACE('',#17712,0.412776);
#1020=SPHERICAL_SURFACE('',#17720,0.412776);
#1021=TOROIDAL_SURFACE('',#17486,1.1,0.309556);
#1022=TOROIDAL_SURFACE('',#17506,1.1,0.309556);
#1023=TOROIDAL_SURFACE('',#17614,1.675,0.412776);
#1024=TOROIDAL_SURFACE('',#17634,1.675,0.412776);
#1025=CONICAL_SURFACE('',#17373,0.475,0.785398163397449);
#1026=CONICAL_SURFACE('',#17377,0.485,0.785398163397448);
#1027=CONICAL_SURFACE('',#17381,0.31,0.463647609000806);
#1028=CONICAL_SURFACE('',#17497,0.63,0.785398163397448);
#1029=CONICAL_SURFACE('',#17504,0.63,0.785398163397448);
#1030=CONICAL_SURFACE('',#17517,1.57,0.785398163397449);
#1031=CONICAL_SURFACE('',#17521,1.57,0.785398163397449);
#1032=CONICAL_SURFACE('',#17625,1.05,0.785398163397449);
#1033=CONICAL_SURFACE('',#17632,1.05,0.785398163397449);
#1034=CONICAL_SURFACE('',#17645,2.3,0.785398163397449);
#1035=CONICAL_SURFACE('',#17649,2.3,0.785398163397449);
#1036=CONICAL_SURFACE('',#17759,0.325,0.785398163397448);
#1037=CONICAL_SURFACE('',#17763,0.335,0.785398163397448);
#1038=CONICAL_SURFACE('',#17767,0.21,0.463647609000806);
#1039=CONICAL_SURFACE('',#17961,0.325,0.785398163397448);
#1040=CONICAL_SURFACE('',#17965,0.335,0.785398163397448);
#1041=CONICAL_SURFACE('',#17969,0.21,0.463647609000806);
#1042=CONICAL_SURFACE('',#18124,0.475,0.785398163397449);
#1043=CONICAL_SURFACE('',#18128,0.485,0.785398163397448);
#1044=CONICAL_SURFACE('',#18132,0.31,0.463647609000806);
#1045=CONICAL_SURFACE('',#18676,0.235,0.785398163397448);
#1046=CONICAL_SURFACE('',#18680,0.2125,0.785398163397448);
#1047=CONICAL_SURFACE('',#18686,0.325,0.785398163397448);
#1048=CONICAL_SURFACE('',#18690,0.335,0.785398163397448);
#1049=CONICAL_SURFACE('',#18694,0.21,0.463647609000806);
#1050=CONICAL_SURFACE('',#18698,0.18,0.785398163397448);
#1051=ORIENTED_CLOSED_SHELL('',*,#16375,.F.);
#1052=ORIENTED_CLOSED_SHELL('',*,#16406,.F.);
#1053=ORIENTED_CLOSED_SHELL('',*,#16413,.F.);
#1054=ORIENTED_CLOSED_SHELL('',*,#16425,.F.);
#1055=ORIENTED_CLOSED_SHELL('',*,#16451,.F.);
#1056=BREP_WITH_VOIDS('Body1',#16376,(#1051));
#1057=BREP_WITH_VOIDS('Body1',#16407,(#1052));
#1058=BREP_WITH_VOIDS('Body1',#16414,(#1053));
#1059=BREP_WITH_VOIDS('Body1',#16426,(#1054));
#1060=BREP_WITH_VOIDS('Body1',#16450,(#1055));
#1061=SHAPE_REPRESENTATION_RELATIONSHIP('SRR','None',#63033,#1125);
#1062=SHAPE_REPRESENTATION_RELATIONSHIP('SRR','None',#63034,#1126);
#1063=SHAPE_REPRESENTATION_RELATIONSHIP('SRR','None',#63035,#1127);
#1064=SHAPE_REPRESENTATION_RELATIONSHIP('SRR','None',#63036,#1128);
#1065=SHAPE_REPRESENTATION_RELATIONSHIP('SRR','None',#63037,#1129);
#1066=SHAPE_REPRESENTATION_RELATIONSHIP('SRR','None',#63038,#1130);
#1067=SHAPE_REPRESENTATION_RELATIONSHIP('SRR','None',#63039,#1131);
#1068=SHAPE_REPRESENTATION_RELATIONSHIP('SRR','None',#63040,#1132);
#1069=SHAPE_REPRESENTATION_RELATIONSHIP('SRR','None',#63041,#1133);
#1070=SHAPE_REPRESENTATION_RELATIONSHIP('SRR','None',#63042,#1134);
#1071=SHAPE_REPRESENTATION_RELATIONSHIP('SRR','None',#63043,#1135);
#1072=SHAPE_REPRESENTATION_RELATIONSHIP('SRR','None',#63045,#1136);
#1073=SHAPE_REPRESENTATION_RELATIONSHIP('SRR','None',#63046,#1137);
#1074=SHAPE_REPRESENTATION_RELATIONSHIP('SRR','None',#63047,#1138);
#1075=SHAPE_REPRESENTATION_RELATIONSHIP('SRR','None',#63048,#1139);
#1076=SHAPE_REPRESENTATION_RELATIONSHIP('SRR','None',#63049,#1140);
#1077=SHAPE_REPRESENTATION_RELATIONSHIP('SRR','None',#63051,#1141);
#1078=SHAPE_REPRESENTATION_RELATIONSHIP('SRR','None',#63052,#1142);
#1079=SHAPE_REPRESENTATION_RELATIONSHIP('SRR','None',#63053,#1143);
#1080=SHAPE_REPRESENTATION_RELATIONSHIP('SRR','None',#63054,#1144);
#1081=SHAPE_REPRESENTATION_RELATIONSHIP('SRR','None',#63055,#1145);
#1082=SHAPE_REPRESENTATION_RELATIONSHIP('SRR','None',#63056,#1146);
#1083=SHAPE_REPRESENTATION_RELATIONSHIP('SRR','None',#63057,#1147);
#1084=SHAPE_REPRESENTATION_RELATIONSHIP('SRR','None',#63058,#1148);
#1085=SHAPE_REPRESENTATION_RELATIONSHIP('SRR','None',#63059,#1149);
#1086=SHAPE_REPRESENTATION_RELATIONSHIP('SRR','None',#63060,#1150);
#1087=SHAPE_REPRESENTATION_RELATIONSHIP('SRR','None',#63061,#1151);
#1088=SHAPE_REPRESENTATION_RELATIONSHIP('SRR','None',#63062,#1152);
#1089=SHAPE_REPRESENTATION_RELATIONSHIP('SRR','None',#63064,#1153);
#1090=SHAPE_REPRESENTATION_RELATIONSHIP('SRR','None',#63065,#1154);
#1091=SHAPE_REPRESENTATION_RELATIONSHIP('SRR','None',#63066,#1155);
#1092=SHAPE_REPRESENTATION_RELATIONSHIP('SRR','None',#63067,#1156);
#1093=SHAPE_REPRESENTATION_RELATIONSHIP('SRR','None',#63068,#1157);
#1094=SHAPE_REPRESENTATION_RELATIONSHIP('SRR','None',#63069,#1158);
#1095=SHAPE_REPRESENTATION_RELATIONSHIP('SRR','None',#63070,#1159);
#1096=SHAPE_REPRESENTATION_RELATIONSHIP('SRR','None',#63071,#1160);
#1097=SHAPE_REPRESENTATION_RELATIONSHIP('SRR','None',#63072,#1161);
#1098=SHAPE_REPRESENTATION_RELATIONSHIP('SRR','None',#63073,#1162);
#1099=SHAPE_REPRESENTATION_RELATIONSHIP('SRR','None',#63074,#1163);
#1100=SHAPE_REPRESENTATION_RELATIONSHIP('SRR','None',#63076,#1164);
#1101=SHAPE_REPRESENTATION_RELATIONSHIP('SRR','None',#63077,#1165);
#1102=SHAPE_REPRESENTATION_RELATIONSHIP('SRR','None',#63078,#1166);
#1103=SHAPE_REPRESENTATION_RELATIONSHIP('SRR','None',#63079,#1167);
#1104=SHAPE_REPRESENTATION_RELATIONSHIP('SRR','None',#63080,#1168);
#1105=SHAPE_REPRESENTATION_RELATIONSHIP('SRR','None',#63082,#1169);
#1106=SHAPE_REPRESENTATION_RELATIONSHIP('SRR','None',#63083,#1170);
#1107=SHAPE_REPRESENTATION_RELATIONSHIP('SRR','None',#63084,#1171);
#1108=SHAPE_REPRESENTATION_RELATIONSHIP('SRR','None',#63085,#1172);
#1109=SHAPE_REPRESENTATION_RELATIONSHIP('SRR','None',#63086,#1173);
#1110=SHAPE_REPRESENTATION_RELATIONSHIP('SRR','None',#63087,#1174);
#1111=SHAPE_REPRESENTATION_RELATIONSHIP('SRR','None',#63088,#1175);
#1112=SHAPE_REPRESENTATION_RELATIONSHIP('SRR','None',#63090,#1176);
#1113=SHAPE_REPRESENTATION_RELATIONSHIP('SRR','None',#63091,#1177);
#1114=SHAPE_REPRESENTATION_RELATIONSHIP('SRR','None',#63092,#1178);
#1115=SHAPE_REPRESENTATION_RELATIONSHIP('SRR','None',#63093,#1179);
#1116=SHAPE_REPRESENTATION_RELATIONSHIP('SRR','None',#63094,#1180);
#1117=SHAPE_REPRESENTATION_RELATIONSHIP('SRR','None',#63095,#1181);
#1118=SHAPE_REPRESENTATION_RELATIONSHIP('SRR','None',#63096,#1182);
#1119=SHAPE_REPRESENTATION_RELATIONSHIP('SRR','None',#63097,#1183);
#1120=SHAPE_REPRESENTATION_RELATIONSHIP('SRR','None',#63098,#1184);
#1121=SHAPE_REPRESENTATION_RELATIONSHIP('SRR','None',#63099,#1185);
#1122=SHAPE_REPRESENTATION_RELATIONSHIP('SRR','None',#63100,#1186);
#1123=SHAPE_REPRESENTATION_RELATIONSHIP('SRR','None',#63101,#1187);
#1124=SHAPE_REPRESENTATION_RELATIONSHIP('SRR','None',#63103,#1188);
#1125=ADVANCED_BREP_SHAPE_REPRESENTATION('',(#1268),#62687);
#1126=ADVANCED_BREP_SHAPE_REPRESENTATION('',(#1269),#62688);
#1127=ADVANCED_BREP_SHAPE_REPRESENTATION('',(#1270),#62689);
#1128=ADVANCED_BREP_SHAPE_REPRESENTATION('',(#1271),#62690);
#1129=ADVANCED_BREP_SHAPE_REPRESENTATION('',(#1272),#62691);
#1130=ADVANCED_BREP_SHAPE_REPRESENTATION('',(#1273),#62692);
#1131=ADVANCED_BREP_SHAPE_REPRESENTATION('',(#1056),#62693);
#1132=ADVANCED_BREP_SHAPE_REPRESENTATION('',(#1274),#62694);
#1133=ADVANCED_BREP_SHAPE_REPRESENTATION('',(#1275),#62695);
#1134=ADVANCED_BREP_SHAPE_REPRESENTATION('',(#1276),#62696);
#1135=ADVANCED_BREP_SHAPE_REPRESENTATION('',(#1277),#62697);
#1136=ADVANCED_BREP_SHAPE_REPRESENTATION('',(#1278),#62699);
#1137=ADVANCED_BREP_SHAPE_REPRESENTATION('',(#1279),#62700);
#1138=ADVANCED_BREP_SHAPE_REPRESENTATION('',(#1280,#1281,#1282,#1283,#1284,
#1285,#1286),#62701);
#1139=ADVANCED_BREP_SHAPE_REPRESENTATION('',(#1287),#62702);
#1140=ADVANCED_BREP_SHAPE_REPRESENTATION('',(#1288,#1289),#62703);
#1141=ADVANCED_BREP_SHAPE_REPRESENTATION('',(#1290),#62705);
#1142=ADVANCED_BREP_SHAPE_REPRESENTATION('',(#1291),#62706);
#1143=ADVANCED_BREP_SHAPE_REPRESENTATION('',(#1292,#1293,#1294,#1295,#1296,
#1297,#1298,#1299),#62707);
#1144=ADVANCED_BREP_SHAPE_REPRESENTATION('',(#1300),#62708);
#1145=ADVANCED_BREP_SHAPE_REPRESENTATION('',(#1301,#1302),#62709);
#1146=ADVANCED_BREP_SHAPE_REPRESENTATION('',(#1057),#62710);
#1147=ADVANCED_BREP_SHAPE_REPRESENTATION('',(#1303),#62711);
#1148=ADVANCED_BREP_SHAPE_REPRESENTATION('',(#1304),#62712);
#1149=ADVANCED_BREP_SHAPE_REPRESENTATION('',(#1305),#62713);
#1150=ADVANCED_BREP_SHAPE_REPRESENTATION('',(#1306),#62714);
#1151=ADVANCED_BREP_SHAPE_REPRESENTATION('',(#1307),#62715);
#1152=ADVANCED_BREP_SHAPE_REPRESENTATION('',(#1058),#62716);
#1153=ADVANCED_BREP_SHAPE_REPRESENTATION('',(#1308),#62718);
#1154=ADVANCED_BREP_SHAPE_REPRESENTATION('',(#1309),#62719);
#1155=ADVANCED_BREP_SHAPE_REPRESENTATION('',(#1310),#62720);
#1156=ADVANCED_BREP_SHAPE_REPRESENTATION('',(#1311),#62721);
#1157=ADVANCED_BREP_SHAPE_REPRESENTATION('',(#1312),#62722);
#1158=ADVANCED_BREP_SHAPE_REPRESENTATION('',(#1313),#62723);
#1159=ADVANCED_BREP_SHAPE_REPRESENTATION('',(#1314),#62724);
#1160=ADVANCED_BREP_SHAPE_REPRESENTATION('',(#1315),#62725);
#1161=ADVANCED_BREP_SHAPE_REPRESENTATION('',(#1316),#62726);
#1162=ADVANCED_BREP_SHAPE_REPRESENTATION('',(#1317),#62727);
#1163=ADVANCED_BREP_SHAPE_REPRESENTATION('',(#1059),#62728);
#1164=ADVANCED_BREP_SHAPE_REPRESENTATION('',(#1318),#62730);
#1165=ADVANCED_BREP_SHAPE_REPRESENTATION('',(#1319),#62731);
#1166=ADVANCED_BREP_SHAPE_REPRESENTATION('',(#1320),#62732);
#1167=ADVANCED_BREP_SHAPE_REPRESENTATION('',(#1321),#62733);
#1168=ADVANCED_BREP_SHAPE_REPRESENTATION('',(#1322),#62734);
#1169=ADVANCED_BREP_SHAPE_REPRESENTATION('',(#1323),#62736);
#1170=ADVANCED_BREP_SHAPE_REPRESENTATION('',(#1324),#62737);
#1171=ADVANCED_BREP_SHAPE_REPRESENTATION('',(#1325),#62738);
#1172=ADVANCED_BREP_SHAPE_REPRESENTATION('',(#1326),#62739);
#1173=ADVANCED_BREP_SHAPE_REPRESENTATION('',(#1327),#62740);
#1174=ADVANCED_BREP_SHAPE_REPRESENTATION('',(#1328),#62741);
#1175=ADVANCED_BREP_SHAPE_REPRESENTATION('',(#1329),#62742);
#1176=ADVANCED_BREP_SHAPE_REPRESENTATION('',(#1330),#62744);
#1177=ADVANCED_BREP_SHAPE_REPRESENTATION('',(#1331),#62745);
#1178=ADVANCED_BREP_SHAPE_REPRESENTATION('',(#1332),#62746);
#1179=ADVANCED_BREP_SHAPE_REPRESENTATION('',(#1333),#62747);
#1180=ADVANCED_BREP_SHAPE_REPRESENTATION('',(#1334),#62748);
#1181=ADVANCED_BREP_SHAPE_REPRESENTATION('',(#1335),#62749);
#1182=ADVANCED_BREP_SHAPE_REPRESENTATION('',(#1336),#62750);
#1183=ADVANCED_BREP_SHAPE_REPRESENTATION('',(#1337),#62751);
#1184=ADVANCED_BREP_SHAPE_REPRESENTATION('',(#1338),#62752);
#1185=ADVANCED_BREP_SHAPE_REPRESENTATION('',(#1339),#62753);
#1186=ADVANCED_BREP_SHAPE_REPRESENTATION('',(#1340),#62754);
#1187=ADVANCED_BREP_SHAPE_REPRESENTATION('',(#1060),#62755);
#1188=ADVANCED_BREP_SHAPE_REPRESENTATION('',(#1341),#62757);
#1189=STYLED_ITEM('',(#63441),#1268);
#1190=STYLED_ITEM('',(#63462),#1269);
#1191=STYLED_ITEM('',(#63462),#1270);
#1192=STYLED_ITEM('',(#63462),#1271);
#1193=STYLED_ITEM('',(#63462),#1272);
#1194=STYLED_ITEM('',(#63462),#1273);
#1195=STYLED_ITEM('',(#63469),#1056);
#1196=STYLED_ITEM('',(#63462),#1274);
#1197=STYLED_ITEM('',(#63462),#1275);
#1198=STYLED_ITEM('',(#63462),#1276);
#1199=STYLED_ITEM('',(#63462),#1277);
#1200=STYLED_ITEM('',(#63462),#1278);
#1201=STYLED_ITEM('',(#63462),#1279);
#1202=STYLED_ITEM('',(#63462),#1280);
#1203=STYLED_ITEM('',(#63462),#1281);
#1204=STYLED_ITEM('',(#63462),#1282);
#1205=STYLED_ITEM('',(#63462),#1283);
#1206=STYLED_ITEM('',(#63462),#1284);
#1207=STYLED_ITEM('',(#63462),#1285);
#1208=STYLED_ITEM('',(#63462),#1286);
#1209=STYLED_ITEM('',(#63462),#1287);
#1210=STYLED_ITEM('',(#63462),#1288);
#1211=STYLED_ITEM('',(#63462),#1289);
#1212=STYLED_ITEM('',(#63462),#1290);
#1213=STYLED_ITEM('',(#63462),#1291);
#1214=STYLED_ITEM('',(#63462),#1292);
#1215=STYLED_ITEM('',(#63462),#1293);
#1216=STYLED_ITEM('',(#63462),#1294);
#1217=STYLED_ITEM('',(#63462),#1295);
#1218=STYLED_ITEM('',(#63462),#1296);
#1219=STYLED_ITEM('',(#63462),#1297);
#1220=STYLED_ITEM('',(#63462),#1298);
#1221=STYLED_ITEM('',(#63462),#1299);
#1222=STYLED_ITEM('',(#63462),#1300);
#1223=STYLED_ITEM('',(#63462),#1301);
#1224=STYLED_ITEM('',(#63462),#1302);
#1225=STYLED_ITEM('',(#63469),#1057);
#1226=STYLED_ITEM('',(#63476),#1303);
#1227=STYLED_ITEM('',(#63455),#1304);
#1228=STYLED_ITEM('',(#63455),#1305);
#1229=STYLED_ITEM('',(#63448),#1306);
#1230=STYLED_ITEM('',(#63448),#1307);
#1231=STYLED_ITEM('',(#63469),#1058);
#1232=STYLED_ITEM('',(#63462),#1308);
#1233=STYLED_ITEM('',(#63476),#1309);
#1234=STYLED_ITEM('',(#63476),#1310);
#1235=STYLED_ITEM('',(#63448),#1311);
#1236=STYLED_ITEM('',(#63455),#1312);
#1237=STYLED_ITEM('',(#63455),#1313);
#1238=STYLED_ITEM('',(#63455),#1314);
#1239=STYLED_ITEM('',(#63448),#1315);
#1240=STYLED_ITEM('',(#63469),#1316);
#1241=STYLED_ITEM('',(#63469),#1317);
#1242=STYLED_ITEM('',(#63469),#1059);
#1243=STYLED_ITEM('',(#63462),#1318);
#1244=STYLED_ITEM('',(#63476),#1319);
#1245=STYLED_ITEM('',(#63476),#1320);
#1246=STYLED_ITEM('',(#63448),#1321);
#1247=STYLED_ITEM('',(#63462),#1322);
#1248=STYLED_ITEM('',(#63462),#1323);
#1249=STYLED_ITEM('',(#63476),#1324);
#1250=STYLED_ITEM('',(#63476),#1325);
#1251=STYLED_ITEM('',(#63448),#1326);
#1252=STYLED_ITEM('',(#63462),#1327);
#1253=STYLED_ITEM('',(#63476),#1328);
#1254=STYLED_ITEM('',(#63462),#1329);
#1255=STYLED_ITEM('',(#63462),#1330);
#1256=STYLED_ITEM('',(#63476),#1331);
#1257=STYLED_ITEM('',(#63476),#1332);
#1258=STYLED_ITEM('',(#63448),#1333);
#1259=STYLED_ITEM('',(#63455),#1334);
#1260=STYLED_ITEM('',(#63455),#1335);
#1261=STYLED_ITEM('',(#63455),#1336);
#1262=STYLED_ITEM('',(#63476),#1337);
#1263=STYLED_ITEM('',(#63455),#1338);
#1264=STYLED_ITEM('',(#63462),#1339);
#1265=STYLED_ITEM('',(#63469),#1340);
#1266=STYLED_ITEM('',(#63469),#1060);
#1267=STYLED_ITEM('',(#63469),#1341);
#1268=MANIFOLD_SOLID_BREP('Body1',#16369);
#1269=MANIFOLD_SOLID_BREP('Body1',#16370);
#1270=MANIFOLD_SOLID_BREP('Body1',#16371);
#1271=MANIFOLD_SOLID_BREP('Body1',#16372);
#1272=MANIFOLD_SOLID_BREP('Body1',#16373);
#1273=MANIFOLD_SOLID_BREP('Body1',#16374);
#1274=MANIFOLD_SOLID_BREP('Body1',#16377);
#1275=MANIFOLD_SOLID_BREP('Body1',#16378);
#1276=MANIFOLD_SOLID_BREP('Body1',#16379);
#1277=MANIFOLD_SOLID_BREP('Body1',#16380);
#1278=MANIFOLD_SOLID_BREP('Body1',#16381);
#1279=MANIFOLD_SOLID_BREP('Body1',#16382);
#1280=MANIFOLD_SOLID_BREP('Body1',#16383);
#1281=MANIFOLD_SOLID_BREP('Body2',#16384);
#1282=MANIFOLD_SOLID_BREP('Body3',#16385);
#1283=MANIFOLD_SOLID_BREP('Body4',#16386);
#1284=MANIFOLD_SOLID_BREP('Body5',#16387);
#1285=MANIFOLD_SOLID_BREP('Body6',#16388);
#1286=MANIFOLD_SOLID_BREP('Body7',#16389);
#1287=MANIFOLD_SOLID_BREP('Continuous crown cage',#16390);
#1288=MANIFOLD_SOLID_BREP('Body1',#16391);
#1289=MANIFOLD_SOLID_BREP('Body2',#16392);
#1290=MANIFOLD_SOLID_BREP('Body1',#16393);
#1291=MANIFOLD_SOLID_BREP('Body1',#16394);
#1292=MANIFOLD_SOLID_BREP('Body1',#16395);
#1293=MANIFOLD_SOLID_BREP('Body2',#16396);
#1294=MANIFOLD_SOLID_BREP('Body3',#16397);
#1295=MANIFOLD_SOLID_BREP('Body4',#16398);
#1296=MANIFOLD_SOLID_BREP('Body5',#16399);
#1297=MANIFOLD_SOLID_BREP('Body6',#16400);
#1298=MANIFOLD_SOLID_BREP('Body7',#16401);
#1299=MANIFOLD_SOLID_BREP('Body8',#16402);
#1300=MANIFOLD_SOLID_BREP('Continuous crown cage',#16403);
#1301=MANIFOLD_SOLID_BREP('Body1',#16404);
#1302=MANIFOLD_SOLID_BREP('Body2',#16405);
#1303=MANIFOLD_SOLID_BREP('Body1',#16408);
#1304=MANIFOLD_SOLID_BREP('Body1',#16409);
#1305=MANIFOLD_SOLID_BREP('Body1',#16410);
#1306=MANIFOLD_SOLID_BREP('Body1',#16411);
#1307=MANIFOLD_SOLID_BREP('Body1',#16412);
#1308=MANIFOLD_SOLID_BREP('Body1',#16415);
#1309=MANIFOLD_SOLID_BREP('Body1',#16416);
#1310=MANIFOLD_SOLID_BREP('Body1',#16417);
#1311=MANIFOLD_SOLID_BREP('Body1',#16418);
#1312=MANIFOLD_SOLID_BREP('Body1',#16419);
#1313=MANIFOLD_SOLID_BREP('Body1',#16420);
#1314=MANIFOLD_SOLID_BREP('Body1',#16421);
#1315=MANIFOLD_SOLID_BREP('Body1',#16422);
#1316=MANIFOLD_SOLID_BREP('Body1',#16423);
#1317=MANIFOLD_SOLID_BREP('Body1',#16424);
#1318=MANIFOLD_SOLID_BREP('Body1',#16427);
#1319=MANIFOLD_SOLID_BREP('Body1',#16428);
#1320=MANIFOLD_SOLID_BREP('Body1',#16429);
#1321=MANIFOLD_SOLID_BREP('Body1',#16430);
#1322=MANIFOLD_SOLID_BREP('Body1',#16431);
#1323=MANIFOLD_SOLID_BREP('Body1',#16432);
#1324=MANIFOLD_SOLID_BREP('Body1',#16433);
#1325=MANIFOLD_SOLID_BREP('Body1',#16434);
#1326=MANIFOLD_SOLID_BREP('Body1',#16435);
#1327=MANIFOLD_SOLID_BREP('Body1',#16436);
#1328=MANIFOLD_SOLID_BREP('Body1',#16437);
#1329=MANIFOLD_SOLID_BREP('Body1',#16438);
#1330=MANIFOLD_SOLID_BREP('Body1',#16439);
#1331=MANIFOLD_SOLID_BREP('Body1',#16440);
#1332=MANIFOLD_SOLID_BREP('Body1',#16441);
#1333=MANIFOLD_SOLID_BREP('Body1',#16442);
#1334=MANIFOLD_SOLID_BREP('Body1',#16443);
#1335=MANIFOLD_SOLID_BREP('Body1',#16444);
#1336=MANIFOLD_SOLID_BREP('Body1',#16445);
#1337=MANIFOLD_SOLID_BREP('Body1',#16446);
#1338=MANIFOLD_SOLID_BREP('Body1',#16447);
#1339=MANIFOLD_SOLID_BREP('Body1',#16448);
#1340=MANIFOLD_SOLID_BREP('Body1',#16449);
#1341=MANIFOLD_SOLID_BREP('Body1',#16452);
#1342=FACE_BOUND('',#3067,.T.);
#1343=FACE_BOUND('',#3068,.T.);
#1344=FACE_BOUND('',#3069,.T.);
#1345=FACE_BOUND('',#3071,.T.);
#1346=FACE_BOUND('',#3072,.T.);
#1347=FACE_BOUND('',#3073,.T.);
#1348=FACE_BOUND('',#3100,.T.);
#1349=FACE_BOUND('',#3101,.T.);
#1350=FACE_BOUND('',#3102,.T.);
#1351=FACE_BOUND('',#3105,.T.);
#1352=FACE_BOUND('',#3106,.T.);
#1353=FACE_BOUND('',#3107,.T.);
#1354=FACE_BOUND('',#3108,.T.);
#1355=FACE_BOUND('',#3109,.T.);
#1356=FACE_BOUND('',#3110,.T.);
#1357=FACE_BOUND('',#3111,.T.);
#1358=FACE_BOUND('',#3112,.T.);
#1359=FACE_BOUND('',#3113,.T.);
#1360=FACE_BOUND('',#3114,.T.);
#1361=FACE_BOUND('',#3115,.T.);
#1362=FACE_BOUND('',#3116,.T.);
#1363=FACE_BOUND('',#3117,.T.);
#1364=FACE_BOUND('',#3118,.T.);
#1365=FACE_BOUND('',#3119,.T.);
#1366=FACE_BOUND('',#3120,.T.);
#1367=FACE_BOUND('',#3121,.T.);
#1368=FACE_BOUND('',#3122,.T.);
#1369=FACE_BOUND('',#3123,.T.);
#1370=FACE_BOUND('',#3124,.T.);
#1371=FACE_BOUND('',#3125,.T.);
#1372=FACE_BOUND('',#3126,.T.);
#1373=FACE_BOUND('',#3129,.T.);
#1374=FACE_BOUND('',#3130,.T.);
#1375=FACE_BOUND('',#3131,.T.);
#1376=FACE_BOUND('',#3132,.T.);
#1377=FACE_BOUND('',#3133,.T.);
#1378=FACE_BOUND('',#3134,.T.);
#1379=FACE_BOUND('',#3135,.T.);
#1380=FACE_BOUND('',#3136,.T.);
#1381=FACE_BOUND('',#3137,.T.);
#1382=FACE_BOUND('',#3138,.T.);
#1383=FACE_BOUND('',#3139,.T.);
#1384=FACE_BOUND('',#3140,.T.);
#1385=FACE_BOUND('',#3141,.T.);
#1386=FACE_BOUND('',#3142,.T.);
#1387=FACE_BOUND('',#3143,.T.);
#1388=FACE_BOUND('',#3144,.T.);
#1389=FACE_BOUND('',#3145,.T.);
#1390=FACE_BOUND('',#3146,.T.);
#1391=FACE_BOUND('',#3147,.T.);
#1392=FACE_BOUND('',#3148,.T.);
#1393=FACE_BOUND('',#3149,.T.);
#1394=FACE_BOUND('',#3150,.T.);
#1395=FACE_BOUND('',#3154,.T.);
#1396=FACE_BOUND('',#3155,.T.);
#1397=FACE_BOUND('',#3156,.T.);
#1398=FACE_BOUND('',#3163,.T.);
#1399=FACE_BOUND('',#3167,.T.);
#1400=FACE_BOUND('',#3168,.T.);
#1401=FACE_BOUND('',#3169,.T.);
#1402=FACE_BOUND('',#3170,.T.);
#1403=FACE_BOUND('',#3171,.T.);
#1404=FACE_BOUND('',#3173,.T.);
#1405=FACE_BOUND('',#3174,.T.);
#1406=FACE_BOUND('',#3175,.T.);
#1407=FACE_BOUND('',#3176,.T.);
#1408=FACE_BOUND('',#3177,.T.);
#1409=FACE_BOUND('',#3184,.T.);
#1410=FACE_BOUND('',#3188,.T.);
#1411=FACE_BOUND('',#3189,.T.);
#1412=FACE_BOUND('',#3190,.T.);
#1413=FACE_BOUND('',#3191,.T.);
#1414=FACE_BOUND('',#3192,.T.);
#1415=FACE_BOUND('',#3194,.T.);
#1416=FACE_BOUND('',#3195,.T.);
#1417=FACE_BOUND('',#3196,.T.);
#1418=FACE_BOUND('',#3197,.T.);
#1419=FACE_BOUND('',#3198,.T.);
#1420=FACE_BOUND('',#3205,.T.);
#1421=FACE_BOUND('',#3209,.T.);
#1422=FACE_BOUND('',#3210,.T.);
#1423=FACE_BOUND('',#3211,.T.);
#1424=FACE_BOUND('',#3212,.T.);
#1425=FACE_BOUND('',#3213,.T.);
#1426=FACE_BOUND('',#3215,.T.);
#1427=FACE_BOUND('',#3216,.T.);
#1428=FACE_BOUND('',#3217,.T.);
#1429=FACE_BOUND('',#3218,.T.);
#1430=FACE_BOUND('',#3219,.T.);
#1431=FACE_BOUND('',#3226,.T.);
#1432=FACE_BOUND('',#3230,.T.);
#1433=FACE_BOUND('',#3231,.T.);
#1434=FACE_BOUND('',#3232,.T.);
#1435=FACE_BOUND('',#3233,.T.);
#1436=FACE_BOUND('',#3234,.T.);
#1437=FACE_BOUND('',#3236,.T.);
#1438=FACE_BOUND('',#3237,.T.);
#1439=FACE_BOUND('',#3238,.T.);
#1440=FACE_BOUND('',#3239,.T.);
#1441=FACE_BOUND('',#3240,.T.);
#1442=FACE_BOUND('',#3255,.T.);
#1443=FACE_BOUND('',#3264,.T.);
#1444=FACE_BOUND('',#3268,.T.);
#1445=FACE_BOUND('',#3269,.T.);
#1446=FACE_BOUND('',#3270,.T.);
#1447=FACE_BOUND('',#3271,.T.);
#1448=FACE_BOUND('',#3272,.T.);
#1449=FACE_BOUND('',#3274,.T.);
#1450=FACE_BOUND('',#3275,.T.);
#1451=FACE_BOUND('',#3276,.T.);
#1452=FACE_BOUND('',#3277,.T.);
#1453=FACE_BOUND('',#3278,.T.);
#1454=FACE_BOUND('',#3285,.T.);
#1455=FACE_BOUND('',#3289,.T.);
#1456=FACE_BOUND('',#3290,.T.);
#1457=FACE_BOUND('',#3291,.T.);
#1458=FACE_BOUND('',#3292,.T.);
#1459=FACE_BOUND('',#3293,.T.);
#1460=FACE_BOUND('',#3295,.T.);
#1461=FACE_BOUND('',#3296,.T.);
#1462=FACE_BOUND('',#3297,.T.);
#1463=FACE_BOUND('',#3298,.T.);
#1464=FACE_BOUND('',#3299,.T.);
#1465=FACE_BOUND('',#3306,.T.);
#1466=FACE_BOUND('',#3310,.T.);
#1467=FACE_BOUND('',#3311,.T.);
#1468=FACE_BOUND('',#3312,.T.);
#1469=FACE_BOUND('',#3313,.T.);
#1470=FACE_BOUND('',#3314,.T.);
#1471=FACE_BOUND('',#3316,.T.);
#1472=FACE_BOUND('',#3317,.T.);
#1473=FACE_BOUND('',#3318,.T.);
#1474=FACE_BOUND('',#3319,.T.);
#1475=FACE_BOUND('',#3320,.T.);
#1476=FACE_BOUND('',#3327,.T.);
#1477=FACE_BOUND('',#3331,.T.);
#1478=FACE_BOUND('',#3332,.T.);
#1479=FACE_BOUND('',#3333,.T.);
#1480=FACE_BOUND('',#3334,.T.);
#1481=FACE_BOUND('',#3335,.T.);
#1482=FACE_BOUND('',#3337,.T.);
#1483=FACE_BOUND('',#3338,.T.);
#1484=FACE_BOUND('',#3339,.T.);
#1485=FACE_BOUND('',#3340,.T.);
#1486=FACE_BOUND('',#3341,.T.);
#1487=FACE_BOUND('',#3347,.T.);
#1488=FACE_BOUND('',#3350,.T.);
#1489=FACE_BOUND('',#3355,.T.);
#1490=FACE_BOUND('',#3360,.T.);
#1491=FACE_BOUND('',#3385,.T.);
#1492=FACE_BOUND('',#3388,.T.);
#1493=FACE_BOUND('',#3391,.T.);
#1494=FACE_BOUND('',#3394,.T.);
#1495=FACE_BOUND('',#3397,.T.);
#1496=FACE_BOUND('',#3404,.T.);
#1497=FACE_BOUND('',#3407,.T.);
#1498=FACE_BOUND('',#3412,.T.);
#1499=FACE_BOUND('',#3417,.T.);
#1500=FACE_BOUND('',#3445,.T.);
#1501=FACE_BOUND('',#3448,.T.);
#1502=FACE_BOUND('',#3451,.T.);
#1503=FACE_BOUND('',#3454,.T.);
#1504=FACE_BOUND('',#3457,.T.);
#1505=FACE_BOUND('',#3473,.T.);
#1506=FACE_BOUND('',#3606,.T.);
#1507=FACE_BOUND('',#3607,.T.);
#1508=FACE_BOUND('',#3608,.T.);
#1509=FACE_BOUND('',#3611,.T.);
#1510=FACE_BOUND('',#3612,.T.);
#1511=FACE_BOUND('',#3613,.T.);
#1512=FACE_BOUND('',#3614,.T.);
#1513=FACE_BOUND('',#3615,.T.);
#1514=FACE_BOUND('',#3616,.T.);
#1515=FACE_BOUND('',#3617,.T.);
#1516=FACE_BOUND('',#3618,.T.);
#1517=FACE_BOUND('',#3619,.T.);
#1518=FACE_BOUND('',#3620,.T.);
#1519=FACE_BOUND('',#3621,.T.);
#1520=FACE_BOUND('',#3622,.T.);
#1521=FACE_BOUND('',#3623,.T.);
#1522=FACE_BOUND('',#3624,.T.);
#1523=FACE_BOUND('',#3625,.T.);
#1524=FACE_BOUND('',#3626,.T.);
#1525=FACE_BOUND('',#3627,.T.);
#1526=FACE_BOUND('',#3628,.T.);
#1527=FACE_BOUND('',#3629,.T.);
#1528=FACE_BOUND('',#3630,.T.);
#1529=FACE_BOUND('',#3631,.T.);
#1530=FACE_BOUND('',#3632,.T.);
#1531=FACE_BOUND('',#3633,.T.);
#1532=FACE_BOUND('',#3634,.T.);
#1533=FACE_BOUND('',#3635,.T.);
#1534=FACE_BOUND('',#3636,.T.);
#1535=FACE_BOUND('',#3637,.T.);
#1536=FACE_BOUND('',#3642,.T.);
#1537=FACE_BOUND('',#3644,.T.);
#1538=FACE_BOUND('',#3648,.T.);
#1539=FACE_BOUND('',#3650,.T.);
#1540=FACE_BOUND('',#3672,.T.);
#1541=FACE_BOUND('',#3680,.T.);
#1542=FACE_BOUND('',#3696,.T.);
#1543=FACE_BOUND('',#3698,.T.);
#1544=FACE_BOUND('',#3702,.T.);
#1545=FACE_BOUND('',#3703,.T.);
#1546=FACE_BOUND('',#3705,.T.);
#1547=FACE_BOUND('',#3710,.T.);
#1548=FACE_BOUND('',#3712,.T.);
#1549=FACE_BOUND('',#3716,.T.);
#1550=FACE_BOUND('',#3718,.T.);
#1551=FACE_BOUND('',#3723,.T.);
#1552=FACE_BOUND('',#3725,.T.);
#1553=FACE_BOUND('',#3727,.T.);
#1554=FACE_BOUND('',#3729,.T.);
#1555=FACE_BOUND('',#3735,.T.);
#1556=FACE_BOUND('',#3739,.T.);
#1557=FACE_BOUND('',#3742,.T.);
#1558=FACE_BOUND('',#3745,.T.);
#1559=FACE_BOUND('',#3747,.T.);
#1560=FACE_BOUND('',#3751,.T.);
#1561=FACE_BOUND('',#3753,.T.);
#1562=FACE_BOUND('',#3757,.T.);
#1563=FACE_BOUND('',#3759,.T.);
#1564=FACE_BOUND('',#3763,.T.);
#1565=FACE_BOUND('',#3765,.T.);
#1566=FACE_BOUND('',#3769,.T.);
#1567=FACE_BOUND('',#3771,.T.);
#1568=FACE_BOUND('',#3775,.T.);
#1569=FACE_BOUND('',#3777,.T.);
#1570=FACE_BOUND('',#3787,.T.);
#1571=FACE_BOUND('',#3795,.T.);
#1572=FACE_BOUND('',#3806,.T.);
#1573=FACE_BOUND('',#3808,.T.);
#1574=FACE_BOUND('',#3812,.T.);
#1575=FACE_BOUND('',#3814,.T.);
#1576=FACE_BOUND('',#3819,.T.);
#1577=FACE_BOUND('',#3821,.T.);
#1578=FACE_BOUND('',#3825,.T.);
#1579=FACE_BOUND('',#3827,.T.);
#1580=FACE_BOUND('',#3832,.T.);
#1581=FACE_BOUND('',#3834,.T.);
#1582=FACE_BOUND('',#3836,.T.);
#1583=FACE_BOUND('',#3838,.T.);
#1584=FACE_BOUND('',#3842,.T.);
#1585=FACE_BOUND('',#3844,.T.);
#1586=FACE_BOUND('',#3853,.T.);
#1587=FACE_BOUND('',#3855,.T.);
#1588=FACE_BOUND('',#3859,.T.);
#1589=FACE_BOUND('',#3861,.T.);
#1590=FACE_BOUND('',#3866,.T.);
#1591=FACE_BOUND('',#3868,.T.);
#1592=FACE_BOUND('',#3872,.T.);
#1593=FACE_BOUND('',#3874,.T.);
#1594=FACE_BOUND('',#3879,.T.);
#1595=FACE_BOUND('',#3881,.T.);
#1596=FACE_BOUND('',#3883,.T.);
#1597=FACE_BOUND('',#3885,.T.);
#1598=FACE_BOUND('',#3889,.T.);
#1599=FACE_BOUND('',#3891,.T.);
#1600=FACE_BOUND('',#3896,.T.);
#1601=FACE_BOUND('',#3900,.T.);
#1602=FACE_BOUND('',#3981,.T.);
#1603=FACE_BOUND('',#4001,.T.);
#1604=FACE_BOUND('',#4003,.T.);
#1605=FACE_BOUND('',#4007,.T.);
#1606=FACE_BOUND('',#4009,.T.);
#1607=FACE_BOUND('',#4014,.T.);
#1608=FACE_BOUND('',#4016,.T.);
#1609=FACE_BOUND('',#4020,.T.);
#1610=FACE_BOUND('',#4022,.T.);
#1611=FACE_BOUND('',#4027,.T.);
#1612=FACE_BOUND('',#4029,.T.);
#1613=FACE_BOUND('',#4031,.T.);
#1614=FACE_BOUND('',#4033,.T.);
#1615=FACE_BOUND('',#4037,.T.);
#1616=FACE_BOUND('',#4039,.T.);
#1617=FACE_BOUND('',#4043,.T.);
#1618=FACE_BOUND('',#4045,.T.);
#1619=FACE_BOUND('',#4054,.T.);
#1620=FACE_BOUND('',#4056,.T.);
#1621=FACE_BOUND('',#4057,.T.);
#1622=FACE_BOUND('',#4059,.T.);
#1623=FACE_BOUND('',#4061,.T.);
#1624=FACE_BOUND('',#4065,.T.);
#1625=FACE_BOUND('',#4067,.T.);
#1626=FACE_BOUND('',#4072,.T.);
#1627=FACE_BOUND('',#4076,.T.);
#1628=FACE_BOUND('',#4237,.T.);
#1629=FACE_BOUND('',#4257,.T.);
#1630=FACE_BOUND('',#4267,.T.);
#1631=FACE_BOUND('',#4283,.T.);
#1632=FACE_BOUND('',#4285,.T.);
#1633=PLANE('',#17170);
#1634=PLANE('',#17171);
#1635=PLANE('',#17172);
#1636=PLANE('',#17173);
#1637=PLANE('',#17174);
#1638=PLANE('',#17175);
#1639=PLANE('',#17252);
#1640=PLANE('',#17253);
#1641=PLANE('',#17254);
#1642=PLANE('',#17255);
#1643=PLANE('',#17256);
#1644=PLANE('',#17257);
#1645=PLANE('',#17258);
#1646=PLANE('',#17259);
#1647=PLANE('',#17276);
#1648=PLANE('',#17283);
#1649=PLANE('',#17284);
#1650=PLANE('',#17301);
#1651=PLANE('',#17308);
#1652=PLANE('',#17309);
#1653=PLANE('',#17326);
#1654=PLANE('',#17333);
#1655=PLANE('',#17334);
#1656=PLANE('',#17351);
#1657=PLANE('',#17358);
#1658=PLANE('',#17359);
#1659=PLANE('',#17361);
#1660=PLANE('',#17362);
#1661=PLANE('',#17363);
#1662=PLANE('',#17364);
#1663=PLANE('',#17365);
#1664=PLANE('',#17366);
#1665=PLANE('',#17367);
#1666=PLANE('',#17368);
#1667=PLANE('',#17369);
#1668=PLANE('',#17371);
#1669=PLANE('',#17379);
#1670=PLANE('',#17400);
#1671=PLANE('',#17407);
#1672=PLANE('',#17408);
#1673=PLANE('',#17425);
#1674=PLANE('',#17432);
#1675=PLANE('',#17433);
#1676=PLANE('',#17450);
#1677=PLANE('',#17457);
#1678=PLANE('',#17458);
#1679=PLANE('',#17475);
#1680=PLANE('',#17482);
#1681=PLANE('',#17483);
#1682=PLANE('',#17499);
#1683=PLANE('',#17502);
#1684=PLANE('',#17514);
#1685=PLANE('',#17523);
#1686=PLANE('',#17554);
#1687=PLANE('',#17559);
#1688=PLANE('',#17564);
#1689=PLANE('',#17570);
#1690=PLANE('',#17575);
#1691=PLANE('',#17584);
#1692=PLANE('',#17588);
#1693=PLANE('',#17589);
#1694=PLANE('',#17591);
#1695=PLANE('',#17596);
#1696=PLANE('',#17599);
#1697=PLANE('',#17604);
#1698=PLANE('',#17627);
#1699=PLANE('',#17630);
#1700=PLANE('',#17642);
#1701=PLANE('',#17651);
#1702=PLANE('',#17684);
#1703=PLANE('',#17689);
#1704=PLANE('',#17694);
#1705=PLANE('',#17699);
#1706=PLANE('',#17704);
#1707=PLANE('',#17709);
#1708=PLANE('',#17718);
#1709=PLANE('',#17722);
#1710=PLANE('',#17723);
#1711=PLANE('',#17725);
#1712=PLANE('',#17730);
#1713=PLANE('',#17733);
#1714=PLANE('',#17738);
#1715=PLANE('',#17747);
#1716=PLANE('',#17748);
#1717=PLANE('',#17749);
#1718=PLANE('',#17750);
#1719=PLANE('',#17751);
#1720=PLANE('',#17752);
#1721=PLANE('',#17753);
#1722=PLANE('',#17754);
#1723=PLANE('',#17755);
#1724=PLANE('',#17757);
#1725=PLANE('',#17765);
#1726=PLANE('',#17771);
#1727=PLANE('',#17772);
#1728=PLANE('',#17773);
#1729=PLANE('',#17774);
#1730=PLANE('',#17775);
#1731=PLANE('',#17776);
#1732=PLANE('',#17777);
#1733=PLANE('',#17778);
#1734=PLANE('',#17779);
#1735=PLANE('',#17780);
#1736=PLANE('',#17781);
#1737=PLANE('',#17782);
#1738=PLANE('',#17783);
#1739=PLANE('',#17784);
#1740=PLANE('',#17785);
#1741=PLANE('',#17786);
#1742=PLANE('',#17787);
#1743=PLANE('',#17788);
#1744=PLANE('',#17789);
#1745=PLANE('',#17790);
#1746=PLANE('',#17791);
#1747=PLANE('',#17792);
#1748=PLANE('',#17793);
#1749=PLANE('',#17794);
#1750=PLANE('',#17795);
#1751=PLANE('',#17796);
#1752=PLANE('',#17797);
#1753=PLANE('',#17798);
#1754=PLANE('',#17799);
#1755=PLANE('',#17800);
#1756=PLANE('',#17801);
#1757=PLANE('',#17802);
#1758=PLANE('',#17803);
#1759=PLANE('',#17804);
#1760=PLANE('',#17805);
#1761=PLANE('',#17806);
#1762=PLANE('',#17807);
#1763=PLANE('',#17808);
#1764=PLANE('',#17809);
#1765=PLANE('',#17810);
#1766=PLANE('',#17811);
#1767=PLANE('',#17812);
#1768=PLANE('',#17813);
#1769=PLANE('',#17814);
#1770=PLANE('',#17815);
#1771=PLANE('',#17816);
#1772=PLANE('',#17817);
#1773=PLANE('',#17818);
#1774=PLANE('',#17819);
#1775=PLANE('',#17820);
#1776=PLANE('',#17821);
#1777=PLANE('',#17822);
#1778=PLANE('',#17823);
#1779=PLANE('',#17824);
#1780=PLANE('',#17825);
#1781=PLANE('',#17826);
#1782=PLANE('',#17827);
#1783=PLANE('',#17828);
#1784=PLANE('',#17829);
#1785=PLANE('',#17830);
#1786=PLANE('',#17831);
#1787=PLANE('',#17832);
#1788=PLANE('',#17833);
#1789=PLANE('',#17834);
#1790=PLANE('',#17835);
#1791=PLANE('',#17836);
#1792=PLANE('',#17837);
#1793=PLANE('',#17838);
#1794=PLANE('',#17839);
#1795=PLANE('',#17840);
#1796=PLANE('',#17841);
#1797=PLANE('',#17842);
#1798=PLANE('',#17843);
#1799=PLANE('',#17844);
#1800=PLANE('',#17845);
#1801=PLANE('',#17846);
#1802=PLANE('',#17847);
#1803=PLANE('',#17848);
#1804=PLANE('',#17849);
#1805=PLANE('',#17850);
#1806=PLANE('',#17851);
#1807=PLANE('',#17852);
#1808=PLANE('',#17853);
#1809=PLANE('',#17854);
#1810=PLANE('',#17855);
#1811=PLANE('',#17856);
#1812=PLANE('',#17857);
#1813=PLANE('',#17858);
#1814=PLANE('',#17859);
#1815=PLANE('',#17860);
#1816=PLANE('',#17861);
#1817=PLANE('',#17862);
#1818=PLANE('',#17863);
#1819=PLANE('',#17864);
#1820=PLANE('',#17865);
#1821=PLANE('',#17866);
#1822=PLANE('',#17867);
#1823=PLANE('',#17868);
#1824=PLANE('',#17869);
#1825=PLANE('',#17870);
#1826=PLANE('',#17871);
#1827=PLANE('',#17872);
#1828=PLANE('',#17873);
#1829=PLANE('',#17874);
#1830=PLANE('',#17875);
#1831=PLANE('',#17876);
#1832=PLANE('',#17877);
#1833=PLANE('',#17878);
#1834=PLANE('',#17879);
#1835=PLANE('',#17880);
#1836=PLANE('',#17881);
#1837=PLANE('',#17882);
#1838=PLANE('',#17883);
#1839=PLANE('',#17884);
#1840=PLANE('',#17885);
#1841=PLANE('',#17886);
#1842=PLANE('',#17887);
#1843=PLANE('',#17888);
#1844=PLANE('',#17889);
#1845=PLANE('',#17890);
#1846=PLANE('',#17900);
#1847=PLANE('',#17901);
#1848=PLANE('',#17902);
#1849=PLANE('',#17903);
#1850=PLANE('',#17904);
#1851=PLANE('',#17905);
#1852=PLANE('',#17906);
#1853=PLANE('',#17908);
#1854=PLANE('',#17909);
#1855=PLANE('',#17919);
#1856=PLANE('',#17920);
#1857=PLANE('',#17928);
#1858=PLANE('',#17929);
#1859=PLANE('',#17931);
#1860=PLANE('',#17932);
#1861=PLANE('',#17933);
#1862=PLANE('',#17934);
#1863=PLANE('',#17935);
#1864=PLANE('',#17936);
#1865=PLANE('',#17938);
#1866=PLANE('',#17939);
#1867=PLANE('',#17940);
#1868=PLANE('',#17941);
#1869=PLANE('',#17942);
#1870=PLANE('',#17943);
#1871=PLANE('',#17945);
#1872=PLANE('',#17946);
#1873=PLANE('',#17947);
#1874=PLANE('',#17948);
#1875=PLANE('',#17949);
#1876=PLANE('',#17950);
#1877=PLANE('',#17951);
#1878=PLANE('',#17952);
#1879=PLANE('',#17953);
#1880=PLANE('',#17958);
#1881=PLANE('',#17959);
#1882=PLANE('',#17967);
#1883=PLANE('',#17977);
#1884=PLANE('',#17978);
#1885=PLANE('',#17979);
#1886=PLANE('',#17981);
#1887=PLANE('',#17982);
#1888=PLANE('',#17983);
#1889=PLANE('',#17985);
#1890=PLANE('',#17986);
#1891=PLANE('',#17988);
#1892=PLANE('',#17989);
#1893=PLANE('',#17990);
#1894=PLANE('',#17992);
#1895=PLANE('',#17995);
#1896=PLANE('',#18003);
#1897=PLANE('',#18004);
#1898=PLANE('',#18012);
#1899=PLANE('',#18013);
#1900=PLANE('',#18021);
#1901=PLANE('',#18022);
#1902=PLANE('',#18024);
#1903=PLANE('',#18029);
#1904=PLANE('',#18036);
#1905=PLANE('',#18037);
#1906=PLANE('',#18042);
#1907=PLANE('',#18043);
#1908=PLANE('',#18044);
#1909=PLANE('',#18045);
#1910=PLANE('',#18053);
#1911=PLANE('',#18055);
#1912=PLANE('',#18056);
#1913=PLANE('',#18058);
#1914=PLANE('',#18061);
#1915=PLANE('',#18069);
#1916=PLANE('',#18070);
#1917=PLANE('',#18078);
#1918=PLANE('',#18079);
#1919=PLANE('',#18087);
#1920=PLANE('',#18088);
#1921=PLANE('',#18096);
#1922=PLANE('',#18097);
#1923=PLANE('',#18105);
#1924=PLANE('',#18106);
#1925=PLANE('',#18108);
#1926=PLANE('',#18109);
#1927=PLANE('',#18110);
#1928=PLANE('',#18111);
#1929=PLANE('',#18112);
#1930=PLANE('',#18113);
#1931=PLANE('',#18114);
#1932=PLANE('',#18115);
#1933=PLANE('',#18116);
#1934=PLANE('',#18121);
#1935=PLANE('',#18122);
#1936=PLANE('',#18130);
#1937=PLANE('',#18140);
#1938=PLANE('',#18141);
#1939=PLANE('',#18142);
#1940=PLANE('',#18144);
#1941=PLANE('',#18145);
#1942=PLANE('',#18146);
#1943=PLANE('',#18148);
#1944=PLANE('',#18151);
#1945=PLANE('',#18159);
#1946=PLANE('',#18160);
#1947=PLANE('',#18168);
#1948=PLANE('',#18169);
#1949=PLANE('',#18177);
#1950=PLANE('',#18178);
#1951=PLANE('',#18180);
#1952=PLANE('',#18185);
#1953=PLANE('',#18192);
#1954=PLANE('',#18193);
#1955=PLANE('',#18201);
#1956=PLANE('',#18202);
#1957=PLANE('',#18208);
#1958=PLANE('',#18209);
#1959=PLANE('',#18210);
#1960=PLANE('',#18212);
#1961=PLANE('',#18213);
#1962=PLANE('',#18214);
#1963=PLANE('',#18216);
#1964=PLANE('',#18219);
#1965=PLANE('',#18227);
#1966=PLANE('',#18228);
#1967=PLANE('',#18236);
#1968=PLANE('',#18237);
#1969=PLANE('',#18245);
#1970=PLANE('',#18246);
#1971=PLANE('',#18248);
#1972=PLANE('',#18253);
#1973=PLANE('',#18260);
#1974=PLANE('',#18261);
#1975=PLANE('',#18269);
#1976=PLANE('',#18270);
#1977=PLANE('',#18272);
#1978=PLANE('',#18273);
#1979=PLANE('',#18274);
#1980=PLANE('',#18275);
#1981=PLANE('',#18302);
#1982=PLANE('',#18303);
#1983=PLANE('',#18306);
#1984=PLANE('',#18309);
#1985=PLANE('',#18312);
#1986=PLANE('',#18315);
#1987=PLANE('',#18318);
#1988=PLANE('',#18321);
#1989=PLANE('',#18324);
#1990=PLANE('',#18327);
#1991=PLANE('',#18330);
#1992=PLANE('',#18333);
#1993=PLANE('',#18336);
#1994=PLANE('',#18339);
#1995=PLANE('',#18342);
#1996=PLANE('',#18345);
#1997=PLANE('',#18348);
#1998=PLANE('',#18351);
#1999=PLANE('',#18354);
#2000=PLANE('',#18357);
#2001=PLANE('',#18360);
#2002=PLANE('',#18361);
#2003=PLANE('',#18365);
#2004=PLANE('',#18366);
#2005=PLANE('',#18367);
#2006=PLANE('',#18368);
#2007=PLANE('',#18369);
#2008=PLANE('',#18370);
#2009=PLANE('',#18371);
#2010=PLANE('',#18372);
#2011=PLANE('',#18373);
#2012=PLANE('',#18374);
#2013=PLANE('',#18380);
#2014=PLANE('',#18381);
#2015=PLANE('',#18382);
#2016=PLANE('',#18384);
#2017=PLANE('',#18385);
#2018=PLANE('',#18386);
#2019=PLANE('',#18388);
#2020=PLANE('',#18391);
#2021=PLANE('',#18399);
#2022=PLANE('',#18400);
#2023=PLANE('',#18408);
#2024=PLANE('',#18409);
#2025=PLANE('',#18417);
#2026=PLANE('',#18418);
#2027=PLANE('',#18420);
#2028=PLANE('',#18425);
#2029=PLANE('',#18432);
#2030=PLANE('',#18433);
#2031=PLANE('',#18441);
#2032=PLANE('',#18442);
#2033=PLANE('',#18450);
#2034=PLANE('',#18451);
#2035=PLANE('',#18453);
#2036=PLANE('',#18458);
#2037=PLANE('',#18459);
#2038=PLANE('',#18460);
#2039=PLANE('',#18462);
#2040=PLANE('',#18464);
#2041=PLANE('',#18471);
#2042=PLANE('',#18472);
#2043=PLANE('',#18480);
#2044=PLANE('',#18481);
#2045=PLANE('',#18483);
#2046=PLANE('',#18484);
#2047=PLANE('',#18485);
#2048=PLANE('',#18486);
#2049=PLANE('',#18533);
#2050=PLANE('',#18534);
#2051=PLANE('',#18537);
#2052=PLANE('',#18540);
#2053=PLANE('',#18543);
#2054=PLANE('',#18546);
#2055=PLANE('',#18549);
#2056=PLANE('',#18552);
#2057=PLANE('',#18555);
#2058=PLANE('',#18558);
#2059=PLANE('',#18561);
#2060=PLANE('',#18564);
#2061=PLANE('',#18567);
#2062=PLANE('',#18570);
#2063=PLANE('',#18573);
#2064=PLANE('',#18576);
#2065=PLANE('',#18579);
#2066=PLANE('',#18582);
#2067=PLANE('',#18585);
#2068=PLANE('',#18588);
#2069=PLANE('',#18591);
#2070=PLANE('',#18594);
#2071=PLANE('',#18597);
#2072=PLANE('',#18600);
#2073=PLANE('',#18603);
#2074=PLANE('',#18606);
#2075=PLANE('',#18609);
#2076=PLANE('',#18612);
#2077=PLANE('',#18615);
#2078=PLANE('',#18618);
#2079=PLANE('',#18621);
#2080=PLANE('',#18624);
#2081=PLANE('',#18627);
#2082=PLANE('',#18630);
#2083=PLANE('',#18633);
#2084=PLANE('',#18636);
#2085=PLANE('',#18639);
#2086=PLANE('',#18642);
#2087=PLANE('',#18645);
#2088=PLANE('',#18648);
#2089=PLANE('',#18651);
#2090=PLANE('',#18652);
#2091=PLANE('',#18656);
#2092=PLANE('',#18657);
#2093=PLANE('',#18658);
#2094=PLANE('',#18659);
#2095=PLANE('',#18660);
#2096=PLANE('',#18661);
#2097=PLANE('',#18662);
#2098=PLANE('',#18663);
#2099=PLANE('',#18664);
#2100=PLANE('',#18665);
#2101=PLANE('',#18667);
#2102=PLANE('',#18668);
#2103=PLANE('',#18669);
#2104=PLANE('',#18670);
#2105=PLANE('',#18671);
#2106=PLANE('',#18672);
#2107=PLANE('',#18673);
#2108=PLANE('',#18674);
#2109=PLANE('',#18682);
#2110=PLANE('',#18684);
#2111=PLANE('',#18692);
#2112=PLANE('',#18700);
#2113=PLANE('',#18701);
#2114=PLANE('',#18702);
#2115=PLANE('',#18703);
#2116=PLANE('',#18704);
#2117=PLANE('',#18705);
#2118=PLANE('',#18706);
#2119=PLANE('',#18707);
#2120=PLANE('',#18708);
#2121=PLANE('',#18822);
#2122=PLANE('',#18823);
#2123=FACE_OUTER_BOUND('',#3059,.T.);
#2124=FACE_OUTER_BOUND('',#3060,.T.);
#2125=FACE_OUTER_BOUND('',#3061,.T.);
#2126=FACE_OUTER_BOUND('',#3062,.T.);
#2127=FACE_OUTER_BOUND('',#3063,.T.);
#2128=FACE_OUTER_BOUND('',#3064,.T.);
#2129=FACE_OUTER_BOUND('',#3065,.T.);
#2130=FACE_OUTER_BOUND('',#3066,.T.);
#2131=FACE_OUTER_BOUND('',#3070,.T.);
#2132=FACE_OUTER_BOUND('',#3074,.T.);
#2133=FACE_OUTER_BOUND('',#3075,.T.);
#2134=FACE_OUTER_BOUND('',#3076,.T.);
#2135=FACE_OUTER_BOUND('',#3077,.T.);
#2136=FACE_OUTER_BOUND('',#3078,.T.);
#2137=FACE_OUTER_BOUND('',#3079,.T.);
#2138=FACE_OUTER_BOUND('',#3080,.T.);
#2139=FACE_OUTER_BOUND('',#3081,.T.);
#2140=FACE_OUTER_BOUND('',#3082,.T.);
#2141=FACE_OUTER_BOUND('',#3083,.T.);
#2142=FACE_OUTER_BOUND('',#3084,.T.);
#2143=FACE_OUTER_BOUND('',#3085,.T.);
#2144=FACE_OUTER_BOUND('',#3086,.T.);
#2145=FACE_OUTER_BOUND('',#3087,.T.);
#2146=FACE_OUTER_BOUND('',#3088,.T.);
#2147=FACE_OUTER_BOUND('',#3089,.T.);
#2148=FACE_OUTER_BOUND('',#3090,.T.);
#2149=FACE_OUTER_BOUND('',#3091,.T.);
#2150=FACE_OUTER_BOUND('',#3092,.T.);
#2151=FACE_OUTER_BOUND('',#3093,.T.);
#2152=FACE_OUTER_BOUND('',#3094,.T.);
#2153=FACE_OUTER_BOUND('',#3095,.T.);
#2154=FACE_OUTER_BOUND('',#3096,.T.);
#2155=FACE_OUTER_BOUND('',#3097,.T.);
#2156=FACE_OUTER_BOUND('',#3098,.T.);
#2157=FACE_OUTER_BOUND('',#3099,.T.);
#2158=FACE_OUTER_BOUND('',#3103,.T.);
#2159=FACE_OUTER_BOUND('',#3104,.T.);
#2160=FACE_OUTER_BOUND('',#3127,.T.);
#2161=FACE_OUTER_BOUND('',#3128,.T.);
#2162=FACE_OUTER_BOUND('',#3151,.T.);
#2163=FACE_OUTER_BOUND('',#3152,.T.);
#2164=FACE_OUTER_BOUND('',#3153,.T.);
#2165=FACE_OUTER_BOUND('',#3157,.T.);
#2166=FACE_OUTER_BOUND('',#3158,.T.);
#2167=FACE_OUTER_BOUND('',#3159,.T.);
#2168=FACE_OUTER_BOUND('',#3160,.T.);
#2169=FACE_OUTER_BOUND('',#3161,.T.);
#2170=FACE_OUTER_BOUND('',#3162,.T.);
#2171=FACE_OUTER_BOUND('',#3164,.T.);
#2172=FACE_OUTER_BOUND('',#3165,.T.);
#2173=FACE_OUTER_BOUND('',#3166,.T.);
#2174=FACE_OUTER_BOUND('',#3172,.T.);
#2175=FACE_OUTER_BOUND('',#3178,.T.);
#2176=FACE_OUTER_BOUND('',#3179,.T.);
#2177=FACE_OUTER_BOUND('',#3180,.T.);
#2178=FACE_OUTER_BOUND('',#3181,.T.);
#2179=FACE_OUTER_BOUND('',#3182,.T.);
#2180=FACE_OUTER_BOUND('',#3183,.T.);
#2181=FACE_OUTER_BOUND('',#3185,.T.);
#2182=FACE_OUTER_BOUND('',#3186,.T.);
#2183=FACE_OUTER_BOUND('',#3187,.T.);
#2184=FACE_OUTER_BOUND('',#3193,.T.);
#2185=FACE_OUTER_BOUND('',#3199,.T.);
#2186=FACE_OUTER_BOUND('',#3200,.T.);
#2187=FACE_OUTER_BOUND('',#3201,.T.);
#2188=FACE_OUTER_BOUND('',#3202,.T.);
#2189=FACE_OUTER_BOUND('',#3203,.T.);
#2190=FACE_OUTER_BOUND('',#3204,.T.);
#2191=FACE_OUTER_BOUND('',#3206,.T.);
#2192=FACE_OUTER_BOUND('',#3207,.T.);
#2193=FACE_OUTER_BOUND('',#3208,.T.);
#2194=FACE_OUTER_BOUND('',#3214,.T.);
#2195=FACE_OUTER_BOUND('',#3220,.T.);
#2196=FACE_OUTER_BOUND('',#3221,.T.);
#2197=FACE_OUTER_BOUND('',#3222,.T.);
#2198=FACE_OUTER_BOUND('',#3223,.T.);
#2199=FACE_OUTER_BOUND('',#3224,.T.);
#2200=FACE_OUTER_BOUND('',#3225,.T.);
#2201=FACE_OUTER_BOUND('',#3227,.T.);
#2202=FACE_OUTER_BOUND('',#3228,.T.);
#2203=FACE_OUTER_BOUND('',#3229,.T.);
#2204=FACE_OUTER_BOUND('',#3235,.T.);
#2205=FACE_OUTER_BOUND('',#3241,.T.);
#2206=FACE_OUTER_BOUND('',#3242,.T.);
#2207=FACE_OUTER_BOUND('',#3243,.T.);
#2208=FACE_OUTER_BOUND('',#3244,.T.);
#2209=FACE_OUTER_BOUND('',#3245,.T.);
#2210=FACE_OUTER_BOUND('',#3246,.T.);
#2211=FACE_OUTER_BOUND('',#3247,.T.);
#2212=FACE_OUTER_BOUND('',#3248,.T.);
#2213=FACE_OUTER_BOUND('',#3249,.T.);
#2214=FACE_OUTER_BOUND('',#3250,.T.);
#2215=FACE_OUTER_BOUND('',#3251,.T.);
#2216=FACE_OUTER_BOUND('',#3252,.T.);
#2217=FACE_OUTER_BOUND('',#3253,.T.);
#2218=FACE_OUTER_BOUND('',#3254,.T.);
#2219=FACE_OUTER_BOUND('',#3256,.T.);
#2220=FACE_OUTER_BOUND('',#3257,.T.);
#2221=FACE_OUTER_BOUND('',#3258,.T.);
#2222=FACE_OUTER_BOUND('',#3259,.T.);
#2223=FACE_OUTER_BOUND('',#3260,.T.);
#2224=FACE_OUTER_BOUND('',#3261,.T.);
#2225=FACE_OUTER_BOUND('',#3262,.T.);
#2226=FACE_OUTER_BOUND('',#3263,.T.);
#2227=FACE_OUTER_BOUND('',#3265,.T.);
#2228=FACE_OUTER_BOUND('',#3266,.T.);
#2229=FACE_OUTER_BOUND('',#3267,.T.);
#2230=FACE_OUTER_BOUND('',#3273,.T.);
#2231=FACE_OUTER_BOUND('',#3279,.T.);
#2232=FACE_OUTER_BOUND('',#3280,.T.);
#2233=FACE_OUTER_BOUND('',#3281,.T.);
#2234=FACE_OUTER_BOUND('',#3282,.T.);
#2235=FACE_OUTER_BOUND('',#3283,.T.);
#2236=FACE_OUTER_BOUND('',#3284,.T.);
#2237=FACE_OUTER_BOUND('',#3286,.T.);
#2238=FACE_OUTER_BOUND('',#3287,.T.);
#2239=FACE_OUTER_BOUND('',#3288,.T.);
#2240=FACE_OUTER_BOUND('',#3294,.T.);
#2241=FACE_OUTER_BOUND('',#3300,.T.);
#2242=FACE_OUTER_BOUND('',#3301,.T.);
#2243=FACE_OUTER_BOUND('',#3302,.T.);
#2244=FACE_OUTER_BOUND('',#3303,.T.);
#2245=FACE_OUTER_BOUND('',#3304,.T.);
#2246=FACE_OUTER_BOUND('',#3305,.T.);
#2247=FACE_OUTER_BOUND('',#3307,.T.);
#2248=FACE_OUTER_BOUND('',#3308,.T.);
#2249=FACE_OUTER_BOUND('',#3309,.T.);
#2250=FACE_OUTER_BOUND('',#3315,.T.);
#2251=FACE_OUTER_BOUND('',#3321,.T.);
#2252=FACE_OUTER_BOUND('',#3322,.T.);
#2253=FACE_OUTER_BOUND('',#3323,.T.);
#2254=FACE_OUTER_BOUND('',#3324,.T.);
#2255=FACE_OUTER_BOUND('',#3325,.T.);
#2256=FACE_OUTER_BOUND('',#3326,.T.);
#2257=FACE_OUTER_BOUND('',#3328,.T.);
#2258=FACE_OUTER_BOUND('',#3329,.T.);
#2259=FACE_OUTER_BOUND('',#3330,.T.);
#2260=FACE_OUTER_BOUND('',#3336,.T.);
#2261=FACE_OUTER_BOUND('',#3342,.T.);
#2262=FACE_OUTER_BOUND('',#3343,.T.);
#2263=FACE_OUTER_BOUND('',#3344,.T.);
#2264=FACE_OUTER_BOUND('',#3345,.T.);
#2265=FACE_OUTER_BOUND('',#3346,.T.);
#2266=FACE_OUTER_BOUND('',#3348,.T.);
#2267=FACE_OUTER_BOUND('',#3349,.T.);
#2268=FACE_OUTER_BOUND('',#3351,.T.);
#2269=FACE_OUTER_BOUND('',#3352,.T.);
#2270=FACE_OUTER_BOUND('',#3353,.T.);
#2271=FACE_OUTER_BOUND('',#3354,.T.);
#2272=FACE_OUTER_BOUND('',#3356,.T.);
#2273=FACE_OUTER_BOUND('',#3357,.T.);
#2274=FACE_OUTER_BOUND('',#3358,.T.);
#2275=FACE_OUTER_BOUND('',#3359,.T.);
#2276=FACE_OUTER_BOUND('',#3361,.T.);
#2277=FACE_OUTER_BOUND('',#3362,.T.);
#2278=FACE_OUTER_BOUND('',#3363,.T.);
#2279=FACE_OUTER_BOUND('',#3364,.T.);
#2280=FACE_OUTER_BOUND('',#3365,.T.);
#2281=FACE_OUTER_BOUND('',#3366,.T.);
#2282=FACE_OUTER_BOUND('',#3367,.T.);
#2283=FACE_OUTER_BOUND('',#3368,.T.);
#2284=FACE_OUTER_BOUND('',#3369,.T.);
#2285=FACE_OUTER_BOUND('',#3370,.T.);
#2286=FACE_OUTER_BOUND('',#3371,.T.);
#2287=FACE_OUTER_BOUND('',#3372,.T.);
#2288=FACE_OUTER_BOUND('',#3373,.T.);
#2289=FACE_OUTER_BOUND('',#3374,.T.);
#2290=FACE_OUTER_BOUND('',#3375,.T.);
#2291=FACE_OUTER_BOUND('',#3376,.T.);
#2292=FACE_OUTER_BOUND('',#3377,.T.);
#2293=FACE_OUTER_BOUND('',#3378,.T.);
#2294=FACE_OUTER_BOUND('',#3379,.T.);
#2295=FACE_OUTER_BOUND('',#3380,.T.);
#2296=FACE_OUTER_BOUND('',#3381,.T.);
#2297=FACE_OUTER_BOUND('',#3382,.T.);
#2298=FACE_OUTER_BOUND('',#3383,.T.);
#2299=FACE_OUTER_BOUND('',#3384,.T.);
#2300=FACE_OUTER_BOUND('',#3386,.T.);
#2301=FACE_OUTER_BOUND('',#3387,.T.);
#2302=FACE_OUTER_BOUND('',#3389,.T.);
#2303=FACE_OUTER_BOUND('',#3390,.T.);
#2304=FACE_OUTER_BOUND('',#3392,.T.);
#2305=FACE_OUTER_BOUND('',#3393,.T.);
#2306=FACE_OUTER_BOUND('',#3395,.T.);
#2307=FACE_OUTER_BOUND('',#3396,.T.);
#2308=FACE_OUTER_BOUND('',#3398,.T.);
#2309=FACE_OUTER_BOUND('',#3399,.T.);
#2310=FACE_OUTER_BOUND('',#3400,.T.);
#2311=FACE_OUTER_BOUND('',#3401,.T.);
#2312=FACE_OUTER_BOUND('',#3402,.T.);
#2313=FACE_OUTER_BOUND('',#3403,.T.);
#2314=FACE_OUTER_BOUND('',#3405,.T.);
#2315=FACE_OUTER_BOUND('',#3406,.T.);
#2316=FACE_OUTER_BOUND('',#3408,.T.);
#2317=FACE_OUTER_BOUND('',#3409,.T.);
#2318=FACE_OUTER_BOUND('',#3410,.T.);
#2319=FACE_OUTER_BOUND('',#3411,.T.);
#2320=FACE_OUTER_BOUND('',#3413,.T.);
#2321=FACE_OUTER_BOUND('',#3414,.T.);
#2322=FACE_OUTER_BOUND('',#3415,.T.);
#2323=FACE_OUTER_BOUND('',#3416,.T.);
#2324=FACE_OUTER_BOUND('',#3418,.T.);
#2325=FACE_OUTER_BOUND('',#3419,.T.);
#2326=FACE_OUTER_BOUND('',#3420,.T.);
#2327=FACE_OUTER_BOUND('',#3421,.T.);
#2328=FACE_OUTER_BOUND('',#3422,.T.);
#2329=FACE_OUTER_BOUND('',#3423,.T.);
#2330=FACE_OUTER_BOUND('',#3424,.T.);
#2331=FACE_OUTER_BOUND('',#3425,.T.);
#2332=FACE_OUTER_BOUND('',#3426,.T.);
#2333=FACE_OUTER_BOUND('',#3427,.T.);
#2334=FACE_OUTER_BOUND('',#3428,.T.);
#2335=FACE_OUTER_BOUND('',#3429,.T.);
#2336=FACE_OUTER_BOUND('',#3430,.T.);
#2337=FACE_OUTER_BOUND('',#3431,.T.);
#2338=FACE_OUTER_BOUND('',#3432,.T.);
#2339=FACE_OUTER_BOUND('',#3433,.T.);
#2340=FACE_OUTER_BOUND('',#3434,.T.);
#2341=FACE_OUTER_BOUND('',#3435,.T.);
#2342=FACE_OUTER_BOUND('',#3436,.T.);
#2343=FACE_OUTER_BOUND('',#3437,.T.);
#2344=FACE_OUTER_BOUND('',#3438,.T.);
#2345=FACE_OUTER_BOUND('',#3439,.T.);
#2346=FACE_OUTER_BOUND('',#3440,.T.);
#2347=FACE_OUTER_BOUND('',#3441,.T.);
#2348=FACE_OUTER_BOUND('',#3442,.T.);
#2349=FACE_OUTER_BOUND('',#3443,.T.);
#2350=FACE_OUTER_BOUND('',#3444,.T.);
#2351=FACE_OUTER_BOUND('',#3446,.T.);
#2352=FACE_OUTER_BOUND('',#3447,.T.);
#2353=FACE_OUTER_BOUND('',#3449,.T.);
#2354=FACE_OUTER_BOUND('',#3450,.T.);
#2355=FACE_OUTER_BOUND('',#3452,.T.);
#2356=FACE_OUTER_BOUND('',#3453,.T.);
#2357=FACE_OUTER_BOUND('',#3455,.T.);
#2358=FACE_OUTER_BOUND('',#3456,.T.);
#2359=FACE_OUTER_BOUND('',#3458,.T.);
#2360=FACE_OUTER_BOUND('',#3459,.T.);
#2361=FACE_OUTER_BOUND('',#3460,.T.);
#2362=FACE_OUTER_BOUND('',#3461,.T.);
#2363=FACE_OUTER_BOUND('',#3462,.T.);
#2364=FACE_OUTER_BOUND('',#3463,.T.);
#2365=FACE_OUTER_BOUND('',#3464,.T.);
#2366=FACE_OUTER_BOUND('',#3465,.T.);
#2367=FACE_OUTER_BOUND('',#3466,.T.);
#2368=FACE_OUTER_BOUND('',#3467,.T.);
#2369=FACE_OUTER_BOUND('',#3468,.T.);
#2370=FACE_OUTER_BOUND('',#3469,.T.);
#2371=FACE_OUTER_BOUND('',#3470,.T.);
#2372=FACE_OUTER_BOUND('',#3471,.T.);
#2373=FACE_OUTER_BOUND('',#3472,.T.);
#2374=FACE_OUTER_BOUND('',#3474,.T.);
#2375=FACE_OUTER_BOUND('',#3475,.T.);
#2376=FACE_OUTER_BOUND('',#3476,.T.);
#2377=FACE_OUTER_BOUND('',#3477,.T.);
#2378=FACE_OUTER_BOUND('',#3478,.T.);
#2379=FACE_OUTER_BOUND('',#3479,.T.);
#2380=FACE_OUTER_BOUND('',#3480,.T.);
#2381=FACE_OUTER_BOUND('',#3481,.T.);
#2382=FACE_OUTER_BOUND('',#3482,.T.);
#2383=FACE_OUTER_BOUND('',#3483,.T.);
#2384=FACE_OUTER_BOUND('',#3484,.T.);
#2385=FACE_OUTER_BOUND('',#3485,.T.);
#2386=FACE_OUTER_BOUND('',#3486,.T.);
#2387=FACE_OUTER_BOUND('',#3487,.T.);
#2388=FACE_OUTER_BOUND('',#3488,.T.);
#2389=FACE_OUTER_BOUND('',#3489,.T.);
#2390=FACE_OUTER_BOUND('',#3490,.T.);
#2391=FACE_OUTER_BOUND('',#3491,.T.);
#2392=FACE_OUTER_BOUND('',#3492,.T.);
#2393=FACE_OUTER_BOUND('',#3493,.T.);
#2394=FACE_OUTER_BOUND('',#3494,.T.);
#2395=FACE_OUTER_BOUND('',#3495,.T.);
#2396=FACE_OUTER_BOUND('',#3496,.T.);
#2397=FACE_OUTER_BOUND('',#3497,.T.);
#2398=FACE_OUTER_BOUND('',#3498,.T.);
#2399=FACE_OUTER_BOUND('',#3499,.T.);
#2400=FACE_OUTER_BOUND('',#3500,.T.);
#2401=FACE_OUTER_BOUND('',#3501,.T.);
#2402=FACE_OUTER_BOUND('',#3502,.T.);
#2403=FACE_OUTER_BOUND('',#3503,.T.);
#2404=FACE_OUTER_BOUND('',#3504,.T.);
#2405=FACE_OUTER_BOUND('',#3505,.T.);
#2406=FACE_OUTER_BOUND('',#3506,.T.);
#2407=FACE_OUTER_BOUND('',#3507,.T.);
#2408=FACE_OUTER_BOUND('',#3508,.T.);
#2409=FACE_OUTER_BOUND('',#3509,.T.);
#2410=FACE_OUTER_BOUND('',#3510,.T.);
#2411=FACE_OUTER_BOUND('',#3511,.T.);
#2412=FACE_OUTER_BOUND('',#3512,.T.);
#2413=FACE_OUTER_BOUND('',#3513,.T.);
#2414=FACE_OUTER_BOUND('',#3514,.T.);
#2415=FACE_OUTER_BOUND('',#3515,.T.);
#2416=FACE_OUTER_BOUND('',#3516,.T.);
#2417=FACE_OUTER_BOUND('',#3517,.T.);
#2418=FACE_OUTER_BOUND('',#3518,.T.);
#2419=FACE_OUTER_BOUND('',#3519,.T.);
#2420=FACE_OUTER_BOUND('',#3520,.T.);
#2421=FACE_OUTER_BOUND('',#3521,.T.);
#2422=FACE_OUTER_BOUND('',#3522,.T.);
#2423=FACE_OUTER_BOUND('',#3523,.T.);
#2424=FACE_OUTER_BOUND('',#3524,.T.);
#2425=FACE_OUTER_BOUND('',#3525,.T.);
#2426=FACE_OUTER_BOUND('',#3526,.T.);
#2427=FACE_OUTER_BOUND('',#3527,.T.);
#2428=FACE_OUTER_BOUND('',#3528,.T.);
#2429=FACE_OUTER_BOUND('',#3529,.T.);
#2430=FACE_OUTER_BOUND('',#3530,.T.);
#2431=FACE_OUTER_BOUND('',#3531,.T.);
#2432=FACE_OUTER_BOUND('',#3532,.T.);
#2433=FACE_OUTER_BOUND('',#3533,.T.);
#2434=FACE_OUTER_BOUND('',#3534,.T.);
#2435=FACE_OUTER_BOUND('',#3535,.T.);
#2436=FACE_OUTER_BOUND('',#3536,.T.);
#2437=FACE_OUTER_BOUND('',#3537,.T.);
#2438=FACE_OUTER_BOUND('',#3538,.T.);
#2439=FACE_OUTER_BOUND('',#3539,.T.);
#2440=FACE_OUTER_BOUND('',#3540,.T.);
#2441=FACE_OUTER_BOUND('',#3541,.T.);
#2442=FACE_OUTER_BOUND('',#3542,.T.);
#2443=FACE_OUTER_BOUND('',#3543,.T.);
#2444=FACE_OUTER_BOUND('',#3544,.T.);
#2445=FACE_OUTER_BOUND('',#3545,.T.);
#2446=FACE_OUTER_BOUND('',#3546,.T.);
#2447=FACE_OUTER_BOUND('',#3547,.T.);
#2448=FACE_OUTER_BOUND('',#3548,.T.);
#2449=FACE_OUTER_BOUND('',#3549,.T.);
#2450=FACE_OUTER_BOUND('',#3550,.T.);
#2451=FACE_OUTER_BOUND('',#3551,.T.);
#2452=FACE_OUTER_BOUND('',#3552,.T.);
#2453=FACE_OUTER_BOUND('',#3553,.T.);
#2454=FACE_OUTER_BOUND('',#3554,.T.);
#2455=FACE_OUTER_BOUND('',#3555,.T.);
#2456=FACE_OUTER_BOUND('',#3556,.T.);
#2457=FACE_OUTER_BOUND('',#3557,.T.);
#2458=FACE_OUTER_BOUND('',#3558,.T.);
#2459=FACE_OUTER_BOUND('',#3559,.T.);
#2460=FACE_OUTER_BOUND('',#3560,.T.);
#2461=FACE_OUTER_BOUND('',#3561,.T.);
#2462=FACE_OUTER_BOUND('',#3562,.T.);
#2463=FACE_OUTER_BOUND('',#3563,.T.);
#2464=FACE_OUTER_BOUND('',#3564,.T.);
#2465=FACE_OUTER_BOUND('',#3565,.T.);
#2466=FACE_OUTER_BOUND('',#3566,.T.);
#2467=FACE_OUTER_BOUND('',#3567,.T.);
#2468=FACE_OUTER_BOUND('',#3568,.T.);
#2469=FACE_OUTER_BOUND('',#3569,.T.);
#2470=FACE_OUTER_BOUND('',#3570,.T.);
#2471=FACE_OUTER_BOUND('',#3571,.T.);
#2472=FACE_OUTER_BOUND('',#3572,.T.);
#2473=FACE_OUTER_BOUND('',#3573,.T.);
#2474=FACE_OUTER_BOUND('',#3574,.T.);
#2475=FACE_OUTER_BOUND('',#3575,.T.);
#2476=FACE_OUTER_BOUND('',#3576,.T.);
#2477=FACE_OUTER_BOUND('',#3577,.T.);
#2478=FACE_OUTER_BOUND('',#3578,.T.);
#2479=FACE_OUTER_BOUND('',#3579,.T.);
#2480=FACE_OUTER_BOUND('',#3580,.T.);
#2481=FACE_OUTER_BOUND('',#3581,.T.);
#2482=FACE_OUTER_BOUND('',#3582,.T.);
#2483=FACE_OUTER_BOUND('',#3583,.T.);
#2484=FACE_OUTER_BOUND('',#3584,.T.);
#2485=FACE_OUTER_BOUND('',#3585,.T.);
#2486=FACE_OUTER_BOUND('',#3586,.T.);
#2487=FACE_OUTER_BOUND('',#3587,.T.);
#2488=FACE_OUTER_BOUND('',#3588,.T.);
#2489=FACE_OUTER_BOUND('',#3589,.T.);
#2490=FACE_OUTER_BOUND('',#3590,.T.);
#2491=FACE_OUTER_BOUND('',#3591,.T.);
#2492=FACE_OUTER_BOUND('',#3592,.T.);
#2493=FACE_OUTER_BOUND('',#3593,.T.);
#2494=FACE_OUTER_BOUND('',#3594,.T.);
#2495=FACE_OUTER_BOUND('',#3595,.T.);
#2496=FACE_OUTER_BOUND('',#3596,.T.);
#2497=FACE_OUTER_BOUND('',#3597,.T.);
#2498=FACE_OUTER_BOUND('',#3598,.T.);
#2499=FACE_OUTER_BOUND('',#3599,.T.);
#2500=FACE_OUTER_BOUND('',#3600,.T.);
#2501=FACE_OUTER_BOUND('',#3601,.T.);
#2502=FACE_OUTER_BOUND('',#3602,.T.);
#2503=FACE_OUTER_BOUND('',#3603,.T.);
#2504=FACE_OUTER_BOUND('',#3604,.T.);
#2505=FACE_OUTER_BOUND('',#3605,.T.);
#2506=FACE_OUTER_BOUND('',#3609,.T.);
#2507=FACE_OUTER_BOUND('',#3610,.T.);
#2508=FACE_OUTER_BOUND('',#3638,.T.);
#2509=FACE_OUTER_BOUND('',#3639,.T.);
#2510=FACE_OUTER_BOUND('',#3640,.T.);
#2511=FACE_OUTER_BOUND('',#3641,.T.);
#2512=FACE_OUTER_BOUND('',#3643,.T.);
#2513=FACE_OUTER_BOUND('',#3645,.T.);
#2514=FACE_OUTER_BOUND('',#3646,.T.);
#2515=FACE_OUTER_BOUND('',#3647,.T.);
#2516=FACE_OUTER_BOUND('',#3649,.T.);
#2517=FACE_OUTER_BOUND('',#3651,.T.);
#2518=FACE_OUTER_BOUND('',#3652,.T.);
#2519=FACE_OUTER_BOUND('',#3653,.T.);
#2520=FACE_OUTER_BOUND('',#3654,.T.);
#2521=FACE_OUTER_BOUND('',#3655,.T.);
#2522=FACE_OUTER_BOUND('',#3656,.T.);
#2523=FACE_OUTER_BOUND('',#3657,.T.);
#2524=FACE_OUTER_BOUND('',#3658,.T.);
#2525=FACE_OUTER_BOUND('',#3659,.T.);
#2526=FACE_OUTER_BOUND('',#3660,.T.);
#2527=FACE_OUTER_BOUND('',#3661,.T.);
#2528=FACE_OUTER_BOUND('',#3662,.T.);
#2529=FACE_OUTER_BOUND('',#3663,.T.);
#2530=FACE_OUTER_BOUND('',#3664,.T.);
#2531=FACE_OUTER_BOUND('',#3665,.T.);
#2532=FACE_OUTER_BOUND('',#3666,.T.);
#2533=FACE_OUTER_BOUND('',#3667,.T.);
#2534=FACE_OUTER_BOUND('',#3668,.T.);
#2535=FACE_OUTER_BOUND('',#3669,.T.);
#2536=FACE_OUTER_BOUND('',#3670,.T.);
#2537=FACE_OUTER_BOUND('',#3671,.T.);
#2538=FACE_OUTER_BOUND('',#3673,.T.);
#2539=FACE_OUTER_BOUND('',#3674,.T.);
#2540=FACE_OUTER_BOUND('',#3675,.T.);
#2541=FACE_OUTER_BOUND('',#3676,.T.);
#2542=FACE_OUTER_BOUND('',#3677,.T.);
#2543=FACE_OUTER_BOUND('',#3678,.T.);
#2544=FACE_OUTER_BOUND('',#3679,.T.);
#2545=FACE_OUTER_BOUND('',#3681,.T.);
#2546=FACE_OUTER_BOUND('',#3682,.T.);
#2547=FACE_OUTER_BOUND('',#3683,.T.);
#2548=FACE_OUTER_BOUND('',#3684,.T.);
#2549=FACE_OUTER_BOUND('',#3685,.T.);
#2550=FACE_OUTER_BOUND('',#3686,.T.);
#2551=FACE_OUTER_BOUND('',#3687,.T.);
#2552=FACE_OUTER_BOUND('',#3688,.T.);
#2553=FACE_OUTER_BOUND('',#3689,.T.);
#2554=FACE_OUTER_BOUND('',#3690,.T.);
#2555=FACE_OUTER_BOUND('',#3691,.T.);
#2556=FACE_OUTER_BOUND('',#3692,.T.);
#2557=FACE_OUTER_BOUND('',#3693,.T.);
#2558=FACE_OUTER_BOUND('',#3694,.T.);
#2559=FACE_OUTER_BOUND('',#3695,.T.);
#2560=FACE_OUTER_BOUND('',#3697,.T.);
#2561=FACE_OUTER_BOUND('',#3699,.T.);
#2562=FACE_OUTER_BOUND('',#3700,.T.);
#2563=FACE_OUTER_BOUND('',#3701,.T.);
#2564=FACE_OUTER_BOUND('',#3704,.T.);
#2565=FACE_OUTER_BOUND('',#3706,.T.);
#2566=FACE_OUTER_BOUND('',#3707,.T.);
#2567=FACE_OUTER_BOUND('',#3708,.T.);
#2568=FACE_OUTER_BOUND('',#3709,.T.);
#2569=FACE_OUTER_BOUND('',#3711,.T.);
#2570=FACE_OUTER_BOUND('',#3713,.T.);
#2571=FACE_OUTER_BOUND('',#3714,.T.);
#2572=FACE_OUTER_BOUND('',#3715,.T.);
#2573=FACE_OUTER_BOUND('',#3717,.T.);
#2574=FACE_OUTER_BOUND('',#3719,.T.);
#2575=FACE_OUTER_BOUND('',#3720,.T.);
#2576=FACE_OUTER_BOUND('',#3721,.T.);
#2577=FACE_OUTER_BOUND('',#3722,.T.);
#2578=FACE_OUTER_BOUND('',#3724,.T.);
#2579=FACE_OUTER_BOUND('',#3726,.T.);
#2580=FACE_OUTER_BOUND('',#3728,.T.);
#2581=FACE_OUTER_BOUND('',#3730,.T.);
#2582=FACE_OUTER_BOUND('',#3731,.T.);
#2583=FACE_OUTER_BOUND('',#3732,.T.);
#2584=FACE_OUTER_BOUND('',#3733,.T.);
#2585=FACE_OUTER_BOUND('',#3734,.T.);
#2586=FACE_OUTER_BOUND('',#3736,.T.);
#2587=FACE_OUTER_BOUND('',#3737,.T.);
#2588=FACE_OUTER_BOUND('',#3738,.T.);
#2589=FACE_OUTER_BOUND('',#3740,.T.);
#2590=FACE_OUTER_BOUND('',#3741,.T.);
#2591=FACE_OUTER_BOUND('',#3743,.T.);
#2592=FACE_OUTER_BOUND('',#3744,.T.);
#2593=FACE_OUTER_BOUND('',#3746,.T.);
#2594=FACE_OUTER_BOUND('',#3748,.T.);
#2595=FACE_OUTER_BOUND('',#3749,.T.);
#2596=FACE_OUTER_BOUND('',#3750,.T.);
#2597=FACE_OUTER_BOUND('',#3752,.T.);
#2598=FACE_OUTER_BOUND('',#3754,.T.);
#2599=FACE_OUTER_BOUND('',#3755,.T.);
#2600=FACE_OUTER_BOUND('',#3756,.T.);
#2601=FACE_OUTER_BOUND('',#3758,.T.);
#2602=FACE_OUTER_BOUND('',#3760,.T.);
#2603=FACE_OUTER_BOUND('',#3761,.T.);
#2604=FACE_OUTER_BOUND('',#3762,.T.);
#2605=FACE_OUTER_BOUND('',#3764,.T.);
#2606=FACE_OUTER_BOUND('',#3766,.T.);
#2607=FACE_OUTER_BOUND('',#3767,.T.);
#2608=FACE_OUTER_BOUND('',#3768,.T.);
#2609=FACE_OUTER_BOUND('',#3770,.T.);
#2610=FACE_OUTER_BOUND('',#3772,.T.);
#2611=FACE_OUTER_BOUND('',#3773,.T.);
#2612=FACE_OUTER_BOUND('',#3774,.T.);
#2613=FACE_OUTER_BOUND('',#3776,.T.);
#2614=FACE_OUTER_BOUND('',#3778,.T.);
#2615=FACE_OUTER_BOUND('',#3779,.T.);
#2616=FACE_OUTER_BOUND('',#3780,.T.);
#2617=FACE_OUTER_BOUND('',#3781,.T.);
#2618=FACE_OUTER_BOUND('',#3782,.T.);
#2619=FACE_OUTER_BOUND('',#3783,.T.);
#2620=FACE_OUTER_BOUND('',#3784,.T.);
#2621=FACE_OUTER_BOUND('',#3785,.T.);
#2622=FACE_OUTER_BOUND('',#3786,.T.);
#2623=FACE_OUTER_BOUND('',#3788,.T.);
#2624=FACE_OUTER_BOUND('',#3789,.T.);
#2625=FACE_OUTER_BOUND('',#3790,.T.);
#2626=FACE_OUTER_BOUND('',#3791,.T.);
#2627=FACE_OUTER_BOUND('',#3792,.T.);
#2628=FACE_OUTER_BOUND('',#3793,.T.);
#2629=FACE_OUTER_BOUND('',#3794,.T.);
#2630=FACE_OUTER_BOUND('',#3796,.T.);
#2631=FACE_OUTER_BOUND('',#3797,.T.);
#2632=FACE_OUTER_BOUND('',#3798,.T.);
#2633=FACE_OUTER_BOUND('',#3799,.T.);
#2634=FACE_OUTER_BOUND('',#3800,.T.);
#2635=FACE_OUTER_BOUND('',#3801,.T.);
#2636=FACE_OUTER_BOUND('',#3802,.T.);
#2637=FACE_OUTER_BOUND('',#3803,.T.);
#2638=FACE_OUTER_BOUND('',#3804,.T.);
#2639=FACE_OUTER_BOUND('',#3805,.T.);
#2640=FACE_OUTER_BOUND('',#3807,.T.);
#2641=FACE_OUTER_BOUND('',#3809,.T.);
#2642=FACE_OUTER_BOUND('',#3810,.T.);
#2643=FACE_OUTER_BOUND('',#3811,.T.);
#2644=FACE_OUTER_BOUND('',#3813,.T.);
#2645=FACE_OUTER_BOUND('',#3815,.T.);
#2646=FACE_OUTER_BOUND('',#3816,.T.);
#2647=FACE_OUTER_BOUND('',#3817,.T.);
#2648=FACE_OUTER_BOUND('',#3818,.T.);
#2649=FACE_OUTER_BOUND('',#3820,.T.);
#2650=FACE_OUTER_BOUND('',#3822,.T.);
#2651=FACE_OUTER_BOUND('',#3823,.T.);
#2652=FACE_OUTER_BOUND('',#3824,.T.);
#2653=FACE_OUTER_BOUND('',#3826,.T.);
#2654=FACE_OUTER_BOUND('',#3828,.T.);
#2655=FACE_OUTER_BOUND('',#3829,.T.);
#2656=FACE_OUTER_BOUND('',#3830,.T.);
#2657=FACE_OUTER_BOUND('',#3831,.T.);
#2658=FACE_OUTER_BOUND('',#3833,.T.);
#2659=FACE_OUTER_BOUND('',#3835,.T.);
#2660=FACE_OUTER_BOUND('',#3837,.T.);
#2661=FACE_OUTER_BOUND('',#3839,.T.);
#2662=FACE_OUTER_BOUND('',#3840,.T.);
#2663=FACE_OUTER_BOUND('',#3841,.T.);
#2664=FACE_OUTER_BOUND('',#3843,.T.);
#2665=FACE_OUTER_BOUND('',#3845,.T.);
#2666=FACE_OUTER_BOUND('',#3846,.T.);
#2667=FACE_OUTER_BOUND('',#3847,.T.);
#2668=FACE_OUTER_BOUND('',#3848,.T.);
#2669=FACE_OUTER_BOUND('',#3849,.T.);
#2670=FACE_OUTER_BOUND('',#3850,.T.);
#2671=FACE_OUTER_BOUND('',#3851,.T.);
#2672=FACE_OUTER_BOUND('',#3852,.T.);
#2673=FACE_OUTER_BOUND('',#3854,.T.);
#2674=FACE_OUTER_BOUND('',#3856,.T.);
#2675=FACE_OUTER_BOUND('',#3857,.T.);
#2676=FACE_OUTER_BOUND('',#3858,.T.);
#2677=FACE_OUTER_BOUND('',#3860,.T.);
#2678=FACE_OUTER_BOUND('',#3862,.T.);
#2679=FACE_OUTER_BOUND('',#3863,.T.);
#2680=FACE_OUTER_BOUND('',#3864,.T.);
#2681=FACE_OUTER_BOUND('',#3865,.T.);
#2682=FACE_OUTER_BOUND('',#3867,.T.);
#2683=FACE_OUTER_BOUND('',#3869,.T.);
#2684=FACE_OUTER_BOUND('',#3870,.T.);
#2685=FACE_OUTER_BOUND('',#3871,.T.);
#2686=FACE_OUTER_BOUND('',#3873,.T.);
#2687=FACE_OUTER_BOUND('',#3875,.T.);
#2688=FACE_OUTER_BOUND('',#3876,.T.);
#2689=FACE_OUTER_BOUND('',#3877,.T.);
#2690=FACE_OUTER_BOUND('',#3878,.T.);
#2691=FACE_OUTER_BOUND('',#3880,.T.);
#2692=FACE_OUTER_BOUND('',#3882,.T.);
#2693=FACE_OUTER_BOUND('',#3884,.T.);
#2694=FACE_OUTER_BOUND('',#3886,.T.);
#2695=FACE_OUTER_BOUND('',#3887,.T.);
#2696=FACE_OUTER_BOUND('',#3888,.T.);
#2697=FACE_OUTER_BOUND('',#3890,.T.);
#2698=FACE_OUTER_BOUND('',#3892,.T.);
#2699=FACE_OUTER_BOUND('',#3893,.T.);
#2700=FACE_OUTER_BOUND('',#3894,.T.);
#2701=FACE_OUTER_BOUND('',#3895,.T.);
#2702=FACE_OUTER_BOUND('',#3897,.T.);
#2703=FACE_OUTER_BOUND('',#3898,.T.);
#2704=FACE_OUTER_BOUND('',#3899,.T.);
#2705=FACE_OUTER_BOUND('',#3901,.T.);
#2706=FACE_OUTER_BOUND('',#3902,.T.);
#2707=FACE_OUTER_BOUND('',#3903,.T.);
#2708=FACE_OUTER_BOUND('',#3904,.T.);
#2709=FACE_OUTER_BOUND('',#3905,.T.);
#2710=FACE_OUTER_BOUND('',#3906,.T.);
#2711=FACE_OUTER_BOUND('',#3907,.T.);
#2712=FACE_OUTER_BOUND('',#3908,.T.);
#2713=FACE_OUTER_BOUND('',#3909,.T.);
#2714=FACE_OUTER_BOUND('',#3910,.T.);
#2715=FACE_OUTER_BOUND('',#3911,.T.);
#2716=FACE_OUTER_BOUND('',#3912,.T.);
#2717=FACE_OUTER_BOUND('',#3913,.T.);
#2718=FACE_OUTER_BOUND('',#3914,.T.);
#2719=FACE_OUTER_BOUND('',#3915,.T.);
#2720=FACE_OUTER_BOUND('',#3916,.T.);
#2721=FACE_OUTER_BOUND('',#3917,.T.);
#2722=FACE_OUTER_BOUND('',#3918,.T.);
#2723=FACE_OUTER_BOUND('',#3919,.T.);
#2724=FACE_OUTER_BOUND('',#3920,.T.);
#2725=FACE_OUTER_BOUND('',#3921,.T.);
#2726=FACE_OUTER_BOUND('',#3922,.T.);
#2727=FACE_OUTER_BOUND('',#3923,.T.);
#2728=FACE_OUTER_BOUND('',#3924,.T.);
#2729=FACE_OUTER_BOUND('',#3925,.T.);
#2730=FACE_OUTER_BOUND('',#3926,.T.);
#2731=FACE_OUTER_BOUND('',#3927,.T.);
#2732=FACE_OUTER_BOUND('',#3928,.T.);
#2733=FACE_OUTER_BOUND('',#3929,.T.);
#2734=FACE_OUTER_BOUND('',#3930,.T.);
#2735=FACE_OUTER_BOUND('',#3931,.T.);
#2736=FACE_OUTER_BOUND('',#3932,.T.);
#2737=FACE_OUTER_BOUND('',#3933,.T.);
#2738=FACE_OUTER_BOUND('',#3934,.T.);
#2739=FACE_OUTER_BOUND('',#3935,.T.);
#2740=FACE_OUTER_BOUND('',#3936,.T.);
#2741=FACE_OUTER_BOUND('',#3937,.T.);
#2742=FACE_OUTER_BOUND('',#3938,.T.);
#2743=FACE_OUTER_BOUND('',#3939,.T.);
#2744=FACE_OUTER_BOUND('',#3940,.T.);
#2745=FACE_OUTER_BOUND('',#3941,.T.);
#2746=FACE_OUTER_BOUND('',#3942,.T.);
#2747=FACE_OUTER_BOUND('',#3943,.T.);
#2748=FACE_OUTER_BOUND('',#3944,.T.);
#2749=FACE_OUTER_BOUND('',#3945,.T.);
#2750=FACE_OUTER_BOUND('',#3946,.T.);
#2751=FACE_OUTER_BOUND('',#3947,.T.);
#2752=FACE_OUTER_BOUND('',#3948,.T.);
#2753=FACE_OUTER_BOUND('',#3949,.T.);
#2754=FACE_OUTER_BOUND('',#3950,.T.);
#2755=FACE_OUTER_BOUND('',#3951,.T.);
#2756=FACE_OUTER_BOUND('',#3952,.T.);
#2757=FACE_OUTER_BOUND('',#3953,.T.);
#2758=FACE_OUTER_BOUND('',#3954,.T.);
#2759=FACE_OUTER_BOUND('',#3955,.T.);
#2760=FACE_OUTER_BOUND('',#3956,.T.);
#2761=FACE_OUTER_BOUND('',#3957,.T.);
#2762=FACE_OUTER_BOUND('',#3958,.T.);
#2763=FACE_OUTER_BOUND('',#3959,.T.);
#2764=FACE_OUTER_BOUND('',#3960,.T.);
#2765=FACE_OUTER_BOUND('',#3961,.T.);
#2766=FACE_OUTER_BOUND('',#3962,.T.);
#2767=FACE_OUTER_BOUND('',#3963,.T.);
#2768=FACE_OUTER_BOUND('',#3964,.T.);
#2769=FACE_OUTER_BOUND('',#3965,.T.);
#2770=FACE_OUTER_BOUND('',#3966,.T.);
#2771=FACE_OUTER_BOUND('',#3967,.T.);
#2772=FACE_OUTER_BOUND('',#3968,.T.);
#2773=FACE_OUTER_BOUND('',#3969,.T.);
#2774=FACE_OUTER_BOUND('',#3970,.T.);
#2775=FACE_OUTER_BOUND('',#3971,.T.);
#2776=FACE_OUTER_BOUND('',#3972,.T.);
#2777=FACE_OUTER_BOUND('',#3973,.T.);
#2778=FACE_OUTER_BOUND('',#3974,.T.);
#2779=FACE_OUTER_BOUND('',#3975,.T.);
#2780=FACE_OUTER_BOUND('',#3976,.T.);
#2781=FACE_OUTER_BOUND('',#3977,.T.);
#2782=FACE_OUTER_BOUND('',#3978,.T.);
#2783=FACE_OUTER_BOUND('',#3979,.T.);
#2784=FACE_OUTER_BOUND('',#3980,.T.);
#2785=FACE_OUTER_BOUND('',#3982,.T.);
#2786=FACE_OUTER_BOUND('',#3983,.T.);
#2787=FACE_OUTER_BOUND('',#3984,.T.);
#2788=FACE_OUTER_BOUND('',#3985,.T.);
#2789=FACE_OUTER_BOUND('',#3986,.T.);
#2790=FACE_OUTER_BOUND('',#3987,.T.);
#2791=FACE_OUTER_BOUND('',#3988,.T.);
#2792=FACE_OUTER_BOUND('',#3989,.T.);
#2793=FACE_OUTER_BOUND('',#3990,.T.);
#2794=FACE_OUTER_BOUND('',#3991,.T.);
#2795=FACE_OUTER_BOUND('',#3992,.T.);
#2796=FACE_OUTER_BOUND('',#3993,.T.);
#2797=FACE_OUTER_BOUND('',#3994,.T.);
#2798=FACE_OUTER_BOUND('',#3995,.T.);
#2799=FACE_OUTER_BOUND('',#3996,.T.);
#2800=FACE_OUTER_BOUND('',#3997,.T.);
#2801=FACE_OUTER_BOUND('',#3998,.T.);
#2802=FACE_OUTER_BOUND('',#3999,.T.);
#2803=FACE_OUTER_BOUND('',#4000,.T.);
#2804=FACE_OUTER_BOUND('',#4002,.T.);
#2805=FACE_OUTER_BOUND('',#4004,.T.);
#2806=FACE_OUTER_BOUND('',#4005,.T.);
#2807=FACE_OUTER_BOUND('',#4006,.T.);
#2808=FACE_OUTER_BOUND('',#4008,.T.);
#2809=FACE_OUTER_BOUND('',#4010,.T.);
#2810=FACE_OUTER_BOUND('',#4011,.T.);
#2811=FACE_OUTER_BOUND('',#4012,.T.);
#2812=FACE_OUTER_BOUND('',#4013,.T.);
#2813=FACE_OUTER_BOUND('',#4015,.T.);
#2814=FACE_OUTER_BOUND('',#4017,.T.);
#2815=FACE_OUTER_BOUND('',#4018,.T.);
#2816=FACE_OUTER_BOUND('',#4019,.T.);
#2817=FACE_OUTER_BOUND('',#4021,.T.);
#2818=FACE_OUTER_BOUND('',#4023,.T.);
#2819=FACE_OUTER_BOUND('',#4024,.T.);
#2820=FACE_OUTER_BOUND('',#4025,.T.);
#2821=FACE_OUTER_BOUND('',#4026,.T.);
#2822=FACE_OUTER_BOUND('',#4028,.T.);
#2823=FACE_OUTER_BOUND('',#4030,.T.);
#2824=FACE_OUTER_BOUND('',#4032,.T.);
#2825=FACE_OUTER_BOUND('',#4034,.T.);
#2826=FACE_OUTER_BOUND('',#4035,.T.);
#2827=FACE_OUTER_BOUND('',#4036,.T.);
#2828=FACE_OUTER_BOUND('',#4038,.T.);
#2829=FACE_OUTER_BOUND('',#4040,.T.);
#2830=FACE_OUTER_BOUND('',#4041,.T.);
#2831=FACE_OUTER_BOUND('',#4042,.T.);
#2832=FACE_OUTER_BOUND('',#4044,.T.);
#2833=FACE_OUTER_BOUND('',#4046,.T.);
#2834=FACE_OUTER_BOUND('',#4047,.T.);
#2835=FACE_OUTER_BOUND('',#4048,.T.);
#2836=FACE_OUTER_BOUND('',#4049,.T.);
#2837=FACE_OUTER_BOUND('',#4050,.T.);
#2838=FACE_OUTER_BOUND('',#4051,.T.);
#2839=FACE_OUTER_BOUND('',#4052,.T.);
#2840=FACE_OUTER_BOUND('',#4053,.T.);
#2841=FACE_OUTER_BOUND('',#4055,.T.);
#2842=FACE_OUTER_BOUND('',#4058,.T.);
#2843=FACE_OUTER_BOUND('',#4060,.T.);
#2844=FACE_OUTER_BOUND('',#4062,.T.);
#2845=FACE_OUTER_BOUND('',#4063,.T.);
#2846=FACE_OUTER_BOUND('',#4064,.T.);
#2847=FACE_OUTER_BOUND('',#4066,.T.);
#2848=FACE_OUTER_BOUND('',#4068,.T.);
#2849=FACE_OUTER_BOUND('',#4069,.T.);
#2850=FACE_OUTER_BOUND('',#4070,.T.);
#2851=FACE_OUTER_BOUND('',#4071,.T.);
#2852=FACE_OUTER_BOUND('',#4073,.T.);
#2853=FACE_OUTER_BOUND('',#4074,.T.);
#2854=FACE_OUTER_BOUND('',#4075,.T.);
#2855=FACE_OUTER_BOUND('',#4077,.T.);
#2856=FACE_OUTER_BOUND('',#4078,.T.);
#2857=FACE_OUTER_BOUND('',#4079,.T.);
#2858=FACE_OUTER_BOUND('',#4080,.T.);
#2859=FACE_OUTER_BOUND('',#4081,.T.);
#2860=FACE_OUTER_BOUND('',#4082,.T.);
#2861=FACE_OUTER_BOUND('',#4083,.T.);
#2862=FACE_OUTER_BOUND('',#4084,.T.);
#2863=FACE_OUTER_BOUND('',#4085,.T.);
#2864=FACE_OUTER_BOUND('',#4086,.T.);
#2865=FACE_OUTER_BOUND('',#4087,.T.);
#2866=FACE_OUTER_BOUND('',#4088,.T.);
#2867=FACE_OUTER_BOUND('',#4089,.T.);
#2868=FACE_OUTER_BOUND('',#4090,.T.);
#2869=FACE_OUTER_BOUND('',#4091,.T.);
#2870=FACE_OUTER_BOUND('',#4092,.T.);
#2871=FACE_OUTER_BOUND('',#4093,.T.);
#2872=FACE_OUTER_BOUND('',#4094,.T.);
#2873=FACE_OUTER_BOUND('',#4095,.T.);
#2874=FACE_OUTER_BOUND('',#4096,.T.);
#2875=FACE_OUTER_BOUND('',#4097,.T.);
#2876=FACE_OUTER_BOUND('',#4098,.T.);
#2877=FACE_OUTER_BOUND('',#4099,.T.);
#2878=FACE_OUTER_BOUND('',#4100,.T.);
#2879=FACE_OUTER_BOUND('',#4101,.T.);
#2880=FACE_OUTER_BOUND('',#4102,.T.);
#2881=FACE_OUTER_BOUND('',#4103,.T.);
#2882=FACE_OUTER_BOUND('',#4104,.T.);
#2883=FACE_OUTER_BOUND('',#4105,.T.);
#2884=FACE_OUTER_BOUND('',#4106,.T.);
#2885=FACE_OUTER_BOUND('',#4107,.T.);
#2886=FACE_OUTER_BOUND('',#4108,.T.);
#2887=FACE_OUTER_BOUND('',#4109,.T.);
#2888=FACE_OUTER_BOUND('',#4110,.T.);
#2889=FACE_OUTER_BOUND('',#4111,.T.);
#2890=FACE_OUTER_BOUND('',#4112,.T.);
#2891=FACE_OUTER_BOUND('',#4113,.T.);
#2892=FACE_OUTER_BOUND('',#4114,.T.);
#2893=FACE_OUTER_BOUND('',#4115,.T.);
#2894=FACE_OUTER_BOUND('',#4116,.T.);
#2895=FACE_OUTER_BOUND('',#4117,.T.);
#2896=FACE_OUTER_BOUND('',#4118,.T.);
#2897=FACE_OUTER_BOUND('',#4119,.T.);
#2898=FACE_OUTER_BOUND('',#4120,.T.);
#2899=FACE_OUTER_BOUND('',#4121,.T.);
#2900=FACE_OUTER_BOUND('',#4122,.T.);
#2901=FACE_OUTER_BOUND('',#4123,.T.);
#2902=FACE_OUTER_BOUND('',#4124,.T.);
#2903=FACE_OUTER_BOUND('',#4125,.T.);
#2904=FACE_OUTER_BOUND('',#4126,.T.);
#2905=FACE_OUTER_BOUND('',#4127,.T.);
#2906=FACE_OUTER_BOUND('',#4128,.T.);
#2907=FACE_OUTER_BOUND('',#4129,.T.);
#2908=FACE_OUTER_BOUND('',#4130,.T.);
#2909=FACE_OUTER_BOUND('',#4131,.T.);
#2910=FACE_OUTER_BOUND('',#4132,.T.);
#2911=FACE_OUTER_BOUND('',#4133,.T.);
#2912=FACE_OUTER_BOUND('',#4134,.T.);
#2913=FACE_OUTER_BOUND('',#4135,.T.);
#2914=FACE_OUTER_BOUND('',#4136,.T.);
#2915=FACE_OUTER_BOUND('',#4137,.T.);
#2916=FACE_OUTER_BOUND('',#4138,.T.);
#2917=FACE_OUTER_BOUND('',#4139,.T.);
#2918=FACE_OUTER_BOUND('',#4140,.T.);
#2919=FACE_OUTER_BOUND('',#4141,.T.);
#2920=FACE_OUTER_BOUND('',#4142,.T.);
#2921=FACE_OUTER_BOUND('',#4143,.T.);
#2922=FACE_OUTER_BOUND('',#4144,.T.);
#2923=FACE_OUTER_BOUND('',#4145,.T.);
#2924=FACE_OUTER_BOUND('',#4146,.T.);
#2925=FACE_OUTER_BOUND('',#4147,.T.);
#2926=FACE_OUTER_BOUND('',#4148,.T.);
#2927=FACE_OUTER_BOUND('',#4149,.T.);
#2928=FACE_OUTER_BOUND('',#4150,.T.);
#2929=FACE_OUTER_BOUND('',#4151,.T.);
#2930=FACE_OUTER_BOUND('',#4152,.T.);
#2931=FACE_OUTER_BOUND('',#4153,.T.);
#2932=FACE_OUTER_BOUND('',#4154,.T.);
#2933=FACE_OUTER_BOUND('',#4155,.T.);
#2934=FACE_OUTER_BOUND('',#4156,.T.);
#2935=FACE_OUTER_BOUND('',#4157,.T.);
#2936=FACE_OUTER_BOUND('',#4158,.T.);
#2937=FACE_OUTER_BOUND('',#4159,.T.);
#2938=FACE_OUTER_BOUND('',#4160,.T.);
#2939=FACE_OUTER_BOUND('',#4161,.T.);
#2940=FACE_OUTER_BOUND('',#4162,.T.);
#2941=FACE_OUTER_BOUND('',#4163,.T.);
#2942=FACE_OUTER_BOUND('',#4164,.T.);
#2943=FACE_OUTER_BOUND('',#4165,.T.);
#2944=FACE_OUTER_BOUND('',#4166,.T.);
#2945=FACE_OUTER_BOUND('',#4167,.T.);
#2946=FACE_OUTER_BOUND('',#4168,.T.);
#2947=FACE_OUTER_BOUND('',#4169,.T.);
#2948=FACE_OUTER_BOUND('',#4170,.T.);
#2949=FACE_OUTER_BOUND('',#4171,.T.);
#2950=FACE_OUTER_BOUND('',#4172,.T.);
#2951=FACE_OUTER_BOUND('',#4173,.T.);
#2952=FACE_OUTER_BOUND('',#4174,.T.);
#2953=FACE_OUTER_BOUND('',#4175,.T.);
#2954=FACE_OUTER_BOUND('',#4176,.T.);
#2955=FACE_OUTER_BOUND('',#4177,.T.);
#2956=FACE_OUTER_BOUND('',#4178,.T.);
#2957=FACE_OUTER_BOUND('',#4179,.T.);
#2958=FACE_OUTER_BOUND('',#4180,.T.);
#2959=FACE_OUTER_BOUND('',#4181,.T.);
#2960=FACE_OUTER_BOUND('',#4182,.T.);
#2961=FACE_OUTER_BOUND('',#4183,.T.);
#2962=FACE_OUTER_BOUND('',#4184,.T.);
#2963=FACE_OUTER_BOUND('',#4185,.T.);
#2964=FACE_OUTER_BOUND('',#4186,.T.);
#2965=FACE_OUTER_BOUND('',#4187,.T.);
#2966=FACE_OUTER_BOUND('',#4188,.T.);
#2967=FACE_OUTER_BOUND('',#4189,.T.);
#2968=FACE_OUTER_BOUND('',#4190,.T.);
#2969=FACE_OUTER_BOUND('',#4191,.T.);
#2970=FACE_OUTER_BOUND('',#4192,.T.);
#2971=FACE_OUTER_BOUND('',#4193,.T.);
#2972=FACE_OUTER_BOUND('',#4194,.T.);
#2973=FACE_OUTER_BOUND('',#4195,.T.);
#2974=FACE_OUTER_BOUND('',#4196,.T.);
#2975=FACE_OUTER_BOUND('',#4197,.T.);
#2976=FACE_OUTER_BOUND('',#4198,.T.);
#2977=FACE_OUTER_BOUND('',#4199,.T.);
#2978=FACE_OUTER_BOUND('',#4200,.T.);
#2979=FACE_OUTER_BOUND('',#4201,.T.);
#2980=FACE_OUTER_BOUND('',#4202,.T.);
#2981=FACE_OUTER_BOUND('',#4203,.T.);
#2982=FACE_OUTER_BOUND('',#4204,.T.);
#2983=FACE_OUTER_BOUND('',#4205,.T.);
#2984=FACE_OUTER_BOUND('',#4206,.T.);
#2985=FACE_OUTER_BOUND('',#4207,.T.);
#2986=FACE_OUTER_BOUND('',#4208,.T.);
#2987=FACE_OUTER_BOUND('',#4209,.T.);
#2988=FACE_OUTER_BOUND('',#4210,.T.);
#2989=FACE_OUTER_BOUND('',#4211,.T.);
#2990=FACE_OUTER_BOUND('',#4212,.T.);
#2991=FACE_OUTER_BOUND('',#4213,.T.);
#2992=FACE_OUTER_BOUND('',#4214,.T.);
#2993=FACE_OUTER_BOUND('',#4215,.T.);
#2994=FACE_OUTER_BOUND('',#4216,.T.);
#2995=FACE_OUTER_BOUND('',#4217,.T.);
#2996=FACE_OUTER_BOUND('',#4218,.T.);
#2997=FACE_OUTER_BOUND('',#4219,.T.);
#2998=FACE_OUTER_BOUND('',#4220,.T.);
#2999=FACE_OUTER_BOUND('',#4221,.T.);
#3000=FACE_OUTER_BOUND('',#4222,.T.);
#3001=FACE_OUTER_BOUND('',#4223,.T.);
#3002=FACE_OUTER_BOUND('',#4224,.T.);
#3003=FACE_OUTER_BOUND('',#4225,.T.);
#3004=FACE_OUTER_BOUND('',#4226,.T.);
#3005=FACE_OUTER_BOUND('',#4227,.T.);
#3006=FACE_OUTER_BOUND('',#4228,.T.);
#3007=FACE_OUTER_BOUND('',#4229,.T.);
#3008=FACE_OUTER_BOUND('',#4230,.T.);
#3009=FACE_OUTER_BOUND('',#4231,.T.);
#3010=FACE_OUTER_BOUND('',#4232,.T.);
#3011=FACE_OUTER_BOUND('',#4233,.T.);
#3012=FACE_OUTER_BOUND('',#4234,.T.);
#3013=FACE_OUTER_BOUND('',#4235,.T.);
#3014=FACE_OUTER_BOUND('',#4236,.T.);
#3015=FACE_OUTER_BOUND('',#4238,.T.);
#3016=FACE_OUTER_BOUND('',#4239,.T.);
#3017=FACE_OUTER_BOUND('',#4240,.T.);
#3018=FACE_OUTER_BOUND('',#4241,.T.);
#3019=FACE_OUTER_BOUND('',#4242,.T.);
#3020=FACE_OUTER_BOUND('',#4243,.T.);
#3021=FACE_OUTER_BOUND('',#4244,.T.);
#3022=FACE_OUTER_BOUND('',#4245,.T.);
#3023=FACE_OUTER_BOUND('',#4246,.T.);
#3024=FACE_OUTER_BOUND('',#4247,.T.);
#3025=FACE_OUTER_BOUND('',#4248,.T.);
#3026=FACE_OUTER_BOUND('',#4249,.T.);
#3027=FACE_OUTER_BOUND('',#4250,.T.);
#3028=FACE_OUTER_BOUND('',#4251,.T.);
#3029=FACE_OUTER_BOUND('',#4252,.T.);
#3030=FACE_OUTER_BOUND('',#4253,.T.);
#3031=FACE_OUTER_BOUND('',#4254,.T.);
#3032=FACE_OUTER_BOUND('',#4255,.T.);
#3033=FACE_OUTER_BOUND('',#4256,.T.);
#3034=FACE_OUTER_BOUND('',#4258,.T.);
#3035=FACE_OUTER_BOUND('',#4259,.T.);
#3036=FACE_OUTER_BOUND('',#4260,.T.);
#3037=FACE_OUTER_BOUND('',#4261,.T.);
#3038=FACE_OUTER_BOUND('',#4262,.T.);
#3039=FACE_OUTER_BOUND('',#4263,.T.);
#3040=FACE_OUTER_BOUND('',#4264,.T.);
#3041=FACE_OUTER_BOUND('',#4265,.T.);
#3042=FACE_OUTER_BOUND('',#4266,.T.);
#3043=FACE_OUTER_BOUND('',#4268,.T.);
#3044=FACE_OUTER_BOUND('',#4269,.T.);
#3045=FACE_OUTER_BOUND('',#4270,.T.);
#3046=FACE_OUTER_BOUND('',#4271,.T.);
#3047=FACE_OUTER_BOUND('',#4272,.T.);
#3048=FACE_OUTER_BOUND('',#4273,.T.);
#3049=FACE_OUTER_BOUND('',#4274,.T.);
#3050=FACE_OUTER_BOUND('',#4275,.T.);
#3051=FACE_OUTER_BOUND('',#4276,.T.);
#3052=FACE_OUTER_BOUND('',#4277,.T.);
#3053=FACE_OUTER_BOUND('',#4278,.T.);
#3054=FACE_OUTER_BOUND('',#4279,.T.);
#3055=FACE_OUTER_BOUND('',#4280,.T.);
#3056=FACE_OUTER_BOUND('',#4281,.T.);
#3057=FACE_OUTER_BOUND('',#4282,.T.);
#3058=FACE_OUTER_BOUND('',#4284,.T.);
#3059=EDGE_LOOP('',(#10835,#10836,#10837,#10838));
#3060=EDGE_LOOP('',(#10839,#10840,#10841,#10842));
#3061=EDGE_LOOP('',(#10843,#10844,#10845,#10846));
#3062=EDGE_LOOP('',(#10847,#10848,#10849,#10850));
#3063=EDGE_LOOP('',(#10851,#10852,#10853,#10854));
#3064=EDGE_LOOP('',(#10855,#10856,#10857,#10858));
#3065=EDGE_LOOP('',(#10859,#10860,#10861,#10862));
#3066=EDGE_LOOP('',(#10863,#10864,#10865,#10866));
#3067=EDGE_LOOP('',(#10867));
#3068=EDGE_LOOP('',(#10868));
#3069=EDGE_LOOP('',(#10869));
#3070=EDGE_LOOP('',(#10870,#10871,#10872,#10873));
#3071=EDGE_LOOP('',(#10874));
#3072=EDGE_LOOP('',(#10875));
#3073=EDGE_LOOP('',(#10876));
#3074=EDGE_LOOP('',(#10877,#10878,#10879,#10880));
#3075=EDGE_LOOP('',(#10881,#10882,#10883,#10884));
#3076=EDGE_LOOP('',(#10885,#10886,#10887,#10888));
#3077=EDGE_LOOP('',(#10889,#10890,#10891,#10892));
#3078=EDGE_LOOP('',(#10893,#10894,#10895,#10896));
#3079=EDGE_LOOP('',(#10897,#10898,#10899,#10900));
#3080=EDGE_LOOP('',(#10901,#10902,#10903,#10904));
#3081=EDGE_LOOP('',(#10905,#10906,#10907,#10908));
#3082=EDGE_LOOP('',(#10909,#10910,#10911,#10912));
#3083=EDGE_LOOP('',(#10913,#10914,#10915,#10916));
#3084=EDGE_LOOP('',(#10917,#10918,#10919,#10920));
#3085=EDGE_LOOP('',(#10921,#10922,#10923,#10924));
#3086=EDGE_LOOP('',(#10925,#10926,#10927,#10928));
#3087=EDGE_LOOP('',(#10929,#10930,#10931,#10932));
#3088=EDGE_LOOP('',(#10933,#10934,#10935,#10936));
#3089=EDGE_LOOP('',(#10937,#10938,#10939,#10940));
#3090=EDGE_LOOP('',(#10941,#10942,#10943,#10944));
#3091=EDGE_LOOP('',(#10945,#10946,#10947,#10948));
#3092=EDGE_LOOP('',(#10949,#10950,#10951,#10952));
#3093=EDGE_LOOP('',(#10953,#10954,#10955,#10956));
#3094=EDGE_LOOP('',(#10957,#10958,#10959,#10960));
#3095=EDGE_LOOP('',(#10961,#10962,#10963,#10964));
#3096=EDGE_LOOP('',(#10965,#10966,#10967,#10968));
#3097=EDGE_LOOP('',(#10969,#10970,#10971,#10972));
#3098=EDGE_LOOP('',(#10973,#10974,#10975,#10976));
#3099=EDGE_LOOP('',(#10977,#10978,#10979,#10980));
#3100=EDGE_LOOP('',(#10981));
#3101=EDGE_LOOP('',(#10982));
#3102=EDGE_LOOP('',(#10983));
#3103=EDGE_LOOP('',(#10984,#10985,#10986,#10987));
#3104=EDGE_LOOP('',(#10988,#10989,#10990,#10991));
#3105=EDGE_LOOP('',(#10992));
#3106=EDGE_LOOP('',(#10993));
#3107=EDGE_LOOP('',(#10994));
#3108=EDGE_LOOP('',(#10995));
#3109=EDGE_LOOP('',(#10996));
#3110=EDGE_LOOP('',(#10997));
#3111=EDGE_LOOP('',(#10998));
#3112=EDGE_LOOP('',(#10999));
#3113=EDGE_LOOP('',(#11000));
#3114=EDGE_LOOP('',(#11001));
#3115=EDGE_LOOP('',(#11002));
#3116=EDGE_LOOP('',(#11003));
#3117=EDGE_LOOP('',(#11004));
#3118=EDGE_LOOP('',(#11005));
#3119=EDGE_LOOP('',(#11006));
#3120=EDGE_LOOP('',(#11007));
#3121=EDGE_LOOP('',(#11008));
#3122=EDGE_LOOP('',(#11009));
#3123=EDGE_LOOP('',(#11010));
#3124=EDGE_LOOP('',(#11011));
#3125=EDGE_LOOP('',(#11012));
#3126=EDGE_LOOP('',(#11013));
#3127=EDGE_LOOP('',(#11014,#11015,#11016,#11017,#11018,#11019));
#3128=EDGE_LOOP('',(#11020,#11021,#11022,#11023));
#3129=EDGE_LOOP('',(#11024));
#3130=EDGE_LOOP('',(#11025));
#3131=EDGE_LOOP('',(#11026));
#3132=EDGE_LOOP('',(#11027));
#3133=EDGE_LOOP('',(#11028));
#3134=EDGE_LOOP('',(#11029));
#3135=EDGE_LOOP('',(#11030));
#3136=EDGE_LOOP('',(#11031));
#3137=EDGE_LOOP('',(#11032));
#3138=EDGE_LOOP('',(#11033));
#3139=EDGE_LOOP('',(#11034));
#3140=EDGE_LOOP('',(#11035));
#3141=EDGE_LOOP('',(#11036));
#3142=EDGE_LOOP('',(#11037));
#3143=EDGE_LOOP('',(#11038));
#3144=EDGE_LOOP('',(#11039));
#3145=EDGE_LOOP('',(#11040));
#3146=EDGE_LOOP('',(#11041));
#3147=EDGE_LOOP('',(#11042));
#3148=EDGE_LOOP('',(#11043));
#3149=EDGE_LOOP('',(#11044));
#3150=EDGE_LOOP('',(#11045));
#3151=EDGE_LOOP('',(#11046,#11047,#11048,#11049,#11050,#11051));
#3152=EDGE_LOOP('',(#11052,#11053,#11054,#11055));
#3153=EDGE_LOOP('',(#11056,#11057,#11058,#11059));
#3154=EDGE_LOOP('',(#11060));
#3155=EDGE_LOOP('',(#11061));
#3156=EDGE_LOOP('',(#11062));
#3157=EDGE_LOOP('',(#11063,#11064,#11065,#11066));
#3158=EDGE_LOOP('',(#11067,#11068,#11069,#11070));
#3159=EDGE_LOOP('',(#11071,#11072,#11073,#11074));
#3160=EDGE_LOOP('',(#11075,#11076,#11077,#11078));
#3161=EDGE_LOOP('',(#11079,#11080,#11081,#11082));
#3162=EDGE_LOOP('',(#11083));
#3163=EDGE_LOOP('',(#11084));
#3164=EDGE_LOOP('',(#11085,#11086,#11087,#11088));
#3165=EDGE_LOOP('',(#11089,#11090,#11091,#11092));
#3166=EDGE_LOOP('',(#11093));
#3167=EDGE_LOOP('',(#11094));
#3168=EDGE_LOOP('',(#11095));
#3169=EDGE_LOOP('',(#11096));
#3170=EDGE_LOOP('',(#11097));
#3171=EDGE_LOOP('',(#11098));
#3172=EDGE_LOOP('',(#11099));
#3173=EDGE_LOOP('',(#11100));
#3174=EDGE_LOOP('',(#11101));
#3175=EDGE_LOOP('',(#11102));
#3176=EDGE_LOOP('',(#11103));
#3177=EDGE_LOOP('',(#11104));
#3178=EDGE_LOOP('',(#11105,#11106,#11107,#11108));
#3179=EDGE_LOOP('',(#11109,#11110,#11111,#11112));
#3180=EDGE_LOOP('',(#11113,#11114,#11115,#11116));
#3181=EDGE_LOOP('',(#11117,#11118,#11119,#11120));
#3182=EDGE_LOOP('',(#11121,#11122,#11123,#11124));
#3183=EDGE_LOOP('',(#11125));
#3184=EDGE_LOOP('',(#11126));
#3185=EDGE_LOOP('',(#11127,#11128,#11129,#11130));
#3186=EDGE_LOOP('',(#11131,#11132,#11133,#11134));
#3187=EDGE_LOOP('',(#11135));
#3188=EDGE_LOOP('',(#11136));
#3189=EDGE_LOOP('',(#11137));
#3190=EDGE_LOOP('',(#11138));
#3191=EDGE_LOOP('',(#11139));
#3192=EDGE_LOOP('',(#11140));
#3193=EDGE_LOOP('',(#11141));
#3194=EDGE_LOOP('',(#11142));
#3195=EDGE_LOOP('',(#11143));
#3196=EDGE_LOOP('',(#11144));
#3197=EDGE_LOOP('',(#11145));
#3198=EDGE_LOOP('',(#11146));
#3199=EDGE_LOOP('',(#11147,#11148,#11149,#11150));
#3200=EDGE_LOOP('',(#11151,#11152,#11153,#11154));
#3201=EDGE_LOOP('',(#11155,#11156,#11157,#11158));
#3202=EDGE_LOOP('',(#11159,#11160,#11161,#11162));
#3203=EDGE_LOOP('',(#11163,#11164,#11165,#11166));
#3204=EDGE_LOOP('',(#11167));
#3205=EDGE_LOOP('',(#11168));
#3206=EDGE_LOOP('',(#11169,#11170,#11171,#11172));
#3207=EDGE_LOOP('',(#11173,#11174,#11175,#11176));
#3208=EDGE_LOOP('',(#11177));
#3209=EDGE_LOOP('',(#11178));
#3210=EDGE_LOOP('',(#11179));
#3211=EDGE_LOOP('',(#11180));
#3212=EDGE_LOOP('',(#11181));
#3213=EDGE_LOOP('',(#11182));
#3214=EDGE_LOOP('',(#11183));
#3215=EDGE_LOOP('',(#11184));
#3216=EDGE_LOOP('',(#11185));
#3217=EDGE_LOOP('',(#11186));
#3218=EDGE_LOOP('',(#11187));
#3219=EDGE_LOOP('',(#11188));
#3220=EDGE_LOOP('',(#11189,#11190,#11191,#11192));
#3221=EDGE_LOOP('',(#11193,#11194,#11195,#11196));
#3222=EDGE_LOOP('',(#11197,#11198,#11199,#11200));
#3223=EDGE_LOOP('',(#11201,#11202,#11203,#11204));
#3224=EDGE_LOOP('',(#11205,#11206,#11207,#11208));
#3225=EDGE_LOOP('',(#11209));
#3226=EDGE_LOOP('',(#11210));
#3227=EDGE_LOOP('',(#11211,#11212,#11213,#11214));
#3228=EDGE_LOOP('',(#11215,#11216,#11217,#11218));
#3229=EDGE_LOOP('',(#11219));
#3230=EDGE_LOOP('',(#11220));
#3231=EDGE_LOOP('',(#11221));
#3232=EDGE_LOOP('',(#11222));
#3233=EDGE_LOOP('',(#11223));
#3234=EDGE_LOOP('',(#11224));
#3235=EDGE_LOOP('',(#11225));
#3236=EDGE_LOOP('',(#11226));
#3237=EDGE_LOOP('',(#11227));
#3238=EDGE_LOOP('',(#11228));
#3239=EDGE_LOOP('',(#11229));
#3240=EDGE_LOOP('',(#11230));
#3241=EDGE_LOOP('',(#11231,#11232,#11233,#11234));
#3242=EDGE_LOOP('',(#11235,#11236,#11237,#11238));
#3243=EDGE_LOOP('',(#11239,#11240,#11241,#11242));
#3244=EDGE_LOOP('',(#11243,#11244,#11245,#11246));
#3245=EDGE_LOOP('',(#11247,#11248,#11249,#11250));
#3246=EDGE_LOOP('',(#11251,#11252,#11253,#11254));
#3247=EDGE_LOOP('',(#11255,#11256,#11257,#11258,#11259,#11260));
#3248=EDGE_LOOP('',(#11261,#11262,#11263,#11264,#11265,#11266));
#3249=EDGE_LOOP('',(#11267));
#3250=EDGE_LOOP('',(#11268));
#3251=EDGE_LOOP('',(#11269,#11270,#11271,#11272));
#3252=EDGE_LOOP('',(#11273,#11274,#11275,#11276));
#3253=EDGE_LOOP('',(#11277,#11278,#11279,#11280));
#3254=EDGE_LOOP('',(#11281));
#3255=EDGE_LOOP('',(#11282));
#3256=EDGE_LOOP('',(#11283,#11284,#11285,#11286));
#3257=EDGE_LOOP('',(#11287,#11288,#11289,#11290));
#3258=EDGE_LOOP('',(#11291,#11292,#11293,#11294));
#3259=EDGE_LOOP('',(#11295,#11296,#11297,#11298));
#3260=EDGE_LOOP('',(#11299,#11300,#11301,#11302));
#3261=EDGE_LOOP('',(#11303,#11304,#11305,#11306));
#3262=EDGE_LOOP('',(#11307,#11308,#11309,#11310));
#3263=EDGE_LOOP('',(#11311));
#3264=EDGE_LOOP('',(#11312));
#3265=EDGE_LOOP('',(#11313,#11314,#11315,#11316));
#3266=EDGE_LOOP('',(#11317,#11318,#11319,#11320));
#3267=EDGE_LOOP('',(#11321));
#3268=EDGE_LOOP('',(#11322));
#3269=EDGE_LOOP('',(#11323));
#3270=EDGE_LOOP('',(#11324));
#3271=EDGE_LOOP('',(#11325));
#3272=EDGE_LOOP('',(#11326));
#3273=EDGE_LOOP('',(#11327));
#3274=EDGE_LOOP('',(#11328));
#3275=EDGE_LOOP('',(#11329));
#3276=EDGE_LOOP('',(#11330));
#3277=EDGE_LOOP('',(#11331));
#3278=EDGE_LOOP('',(#11332));
#3279=EDGE_LOOP('',(#11333,#11334,#11335,#11336));
#3280=EDGE_LOOP('',(#11337,#11338,#11339,#11340));
#3281=EDGE_LOOP('',(#11341,#11342,#11343,#11344));
#3282=EDGE_LOOP('',(#11345,#11346,#11347,#11348));
#3283=EDGE_LOOP('',(#11349,#11350,#11351,#11352));
#3284=EDGE_LOOP('',(#11353));
#3285=EDGE_LOOP('',(#11354));
#3286=EDGE_LOOP('',(#11355,#11356,#11357,#11358));
#3287=EDGE_LOOP('',(#11359,#11360,#11361,#11362));
#3288=EDGE_LOOP('',(#11363));
#3289=EDGE_LOOP('',(#11364));
#3290=EDGE_LOOP('',(#11365));
#3291=EDGE_LOOP('',(#11366));
#3292=EDGE_LOOP('',(#11367));
#3293=EDGE_LOOP('',(#11368));
#3294=EDGE_LOOP('',(#11369));
#3295=EDGE_LOOP('',(#11370));
#3296=EDGE_LOOP('',(#11371));
#3297=EDGE_LOOP('',(#11372));
#3298=EDGE_LOOP('',(#11373));
#3299=EDGE_LOOP('',(#11374));
#3300=EDGE_LOOP('',(#11375,#11376,#11377,#11378));
#3301=EDGE_LOOP('',(#11379,#11380,#11381,#11382));
#3302=EDGE_LOOP('',(#11383,#11384,#11385,#11386));
#3303=EDGE_LOOP('',(#11387,#11388,#11389,#11390));
#3304=EDGE_LOOP('',(#11391,#11392,#11393,#11394));
#3305=EDGE_LOOP('',(#11395));
#3306=EDGE_LOOP('',(#11396));
#3307=EDGE_LOOP('',(#11397,#11398,#11399,#11400));
#3308=EDGE_LOOP('',(#11401,#11402,#11403,#11404));
#3309=EDGE_LOOP('',(#11405));
#3310=EDGE_LOOP('',(#11406));
#3311=EDGE_LOOP('',(#11407));
#3312=EDGE_LOOP('',(#11408));
#3313=EDGE_LOOP('',(#11409));
#3314=EDGE_LOOP('',(#11410));
#3315=EDGE_LOOP('',(#11411));
#3316=EDGE_LOOP('',(#11412));
#3317=EDGE_LOOP('',(#11413));
#3318=EDGE_LOOP('',(#11414));
#3319=EDGE_LOOP('',(#11415));
#3320=EDGE_LOOP('',(#11416));
#3321=EDGE_LOOP('',(#11417,#11418,#11419,#11420));
#3322=EDGE_LOOP('',(#11421,#11422,#11423,#11424));
#3323=EDGE_LOOP('',(#11425,#11426,#11427,#11428));
#3324=EDGE_LOOP('',(#11429,#11430,#11431,#11432));
#3325=EDGE_LOOP('',(#11433,#11434,#11435,#11436));
#3326=EDGE_LOOP('',(#11437));
#3327=EDGE_LOOP('',(#11438));
#3328=EDGE_LOOP('',(#11439,#11440,#11441,#11442));
#3329=EDGE_LOOP('',(#11443,#11444,#11445,#11446));
#3330=EDGE_LOOP('',(#11447));
#3331=EDGE_LOOP('',(#11448));
#3332=EDGE_LOOP('',(#11449));
#3333=EDGE_LOOP('',(#11450));
#3334=EDGE_LOOP('',(#11451));
#3335=EDGE_LOOP('',(#11452));
#3336=EDGE_LOOP('',(#11453));
#3337=EDGE_LOOP('',(#11454));
#3338=EDGE_LOOP('',(#11455));
#3339=EDGE_LOOP('',(#11456));
#3340=EDGE_LOOP('',(#11457));
#3341=EDGE_LOOP('',(#11458));
#3342=EDGE_LOOP('',(#11459,#11460,#11461,#11462,#11463,#11464));
#3343=EDGE_LOOP('',(#11465,#11466,#11467,#11468,#11469));
#3344=EDGE_LOOP('',(#11470,#11471,#11472,#11473));
#3345=EDGE_LOOP('',(#11474,#11475,#11476,#11477));
#3346=EDGE_LOOP('',(#11478));
#3347=EDGE_LOOP('',(#11479));
#3348=EDGE_LOOP('',(#11480,#11481,#11482,#11483,#11484));
#3349=EDGE_LOOP('',(#11485));
#3350=EDGE_LOOP('',(#11486));
#3351=EDGE_LOOP('',(#11487,#11488,#11489,#11490));
#3352=EDGE_LOOP('',(#11491,#11492,#11493,#11494,#11495,#11496));
#3353=EDGE_LOOP('',(#11497,#11498,#11499,#11500,#11501));
#3354=EDGE_LOOP('',(#11502));
#3355=EDGE_LOOP('',(#11503));
#3356=EDGE_LOOP('',(#11504,#11505,#11506,#11507));
#3357=EDGE_LOOP('',(#11508,#11509,#11510,#11511));
#3358=EDGE_LOOP('',(#11512,#11513,#11514,#11515));
#3359=EDGE_LOOP('',(#11516));
#3360=EDGE_LOOP('',(#11517));
#3361=EDGE_LOOP('',(#11518,#11519,#11520,#11521,#11522));
#3362=EDGE_LOOP('',(#11523,#11524));
#3363=EDGE_LOOP('',(#11525,#11526));
#3364=EDGE_LOOP('',(#11527,#11528));
#3365=EDGE_LOOP('',(#11529,#11530));
#3366=EDGE_LOOP('',(#11531,#11532));
#3367=EDGE_LOOP('',(#11533,#11534));
#3368=EDGE_LOOP('',(#11535,#11536));
#3369=EDGE_LOOP('',(#11537,#11538,#11539,#11540));
#3370=EDGE_LOOP('',(#11541,#11542,#11543,#11544,#11545,#11546,#11547,#11548,
#11549,#11550,#11551,#11552,#11553,#11554,#11555,#11556,#11557,#11558));
#3371=EDGE_LOOP('',(#11559,#11560,#11561,#11562));
#3372=EDGE_LOOP('',(#11563,#11564,#11565,#11566));
#3373=EDGE_LOOP('',(#11567,#11568,#11569,#11570));
#3374=EDGE_LOOP('',(#11571,#11572,#11573,#11574));
#3375=EDGE_LOOP('',(#11575,#11576,#11577,#11578,#11579,#11580));
#3376=EDGE_LOOP('',(#11581,#11582,#11583,#11584));
#3377=EDGE_LOOP('',(#11585,#11586,#11587,#11588));
#3378=EDGE_LOOP('',(#11589,#11590,#11591,#11592));
#3379=EDGE_LOOP('',(#11593,#11594,#11595,#11596));
#3380=EDGE_LOOP('',(#11597,#11598,#11599,#11600));
#3381=EDGE_LOOP('',(#11601,#11602,#11603,#11604,#11605,#11606,#11607,#11608,
#11609,#11610,#11611,#11612,#11613,#11614,#11615,#11616,#11617,#11618));
#3382=EDGE_LOOP('',(#11619,#11620,#11621,#11622));
#3383=EDGE_LOOP('',(#11623,#11624,#11625,#11626));
#3384=EDGE_LOOP('',(#11627));
#3385=EDGE_LOOP('',(#11628));
#3386=EDGE_LOOP('',(#11629,#11630,#11631,#11632));
#3387=EDGE_LOOP('',(#11633));
#3388=EDGE_LOOP('',(#11634));
#3389=EDGE_LOOP('',(#11635,#11636,#11637,#11638));
#3390=EDGE_LOOP('',(#11639));
#3391=EDGE_LOOP('',(#11640));
#3392=EDGE_LOOP('',(#11641,#11642,#11643,#11644));
#3393=EDGE_LOOP('',(#11645));
#3394=EDGE_LOOP('',(#11646));
#3395=EDGE_LOOP('',(#11647,#11648,#11649,#11650));
#3396=EDGE_LOOP('',(#11651));
#3397=EDGE_LOOP('',(#11652));
#3398=EDGE_LOOP('',(#11653,#11654,#11655,#11656));
#3399=EDGE_LOOP('',(#11657,#11658,#11659,#11660,#11661,#11662));
#3400=EDGE_LOOP('',(#11663,#11664,#11665,#11666,#11667));
#3401=EDGE_LOOP('',(#11668,#11669,#11670,#11671));
#3402=EDGE_LOOP('',(#11672,#11673,#11674,#11675));
#3403=EDGE_LOOP('',(#11676));
#3404=EDGE_LOOP('',(#11677));
#3405=EDGE_LOOP('',(#11678,#11679,#11680,#11681,#11682));
#3406=EDGE_LOOP('',(#11683));
#3407=EDGE_LOOP('',(#11684));
#3408=EDGE_LOOP('',(#11685,#11686,#11687,#11688));
#3409=EDGE_LOOP('',(#11689,#11690,#11691,#11692,#11693,#11694));
#3410=EDGE_LOOP('',(#11695,#11696,#11697,#11698,#11699));
#3411=EDGE_LOOP('',(#11700));
#3412=EDGE_LOOP('',(#11701));
#3413=EDGE_LOOP('',(#11702,#11703,#11704,#11705));
#3414=EDGE_LOOP('',(#11706,#11707,#11708,#11709));
#3415=EDGE_LOOP('',(#11710,#11711,#11712,#11713));
#3416=EDGE_LOOP('',(#11714));
#3417=EDGE_LOOP('',(#11715));
#3418=EDGE_LOOP('',(#11716,#11717,#11718,#11719,#11720));
#3419=EDGE_LOOP('',(#11721,#11722));
#3420=EDGE_LOOP('',(#11723,#11724));
#3421=EDGE_LOOP('',(#11725,#11726));
#3422=EDGE_LOOP('',(#11727,#11728));
#3423=EDGE_LOOP('',(#11729,#11730));
#3424=EDGE_LOOP('',(#11731,#11732));
#3425=EDGE_LOOP('',(#11733,#11734));
#3426=EDGE_LOOP('',(#11735,#11736));
#3427=EDGE_LOOP('',(#11737,#11738,#11739,#11740));
#3428=EDGE_LOOP('',(#11741,#11742,#11743,#11744,#11745,#11746,#11747,#11748,
#11749,#11750,#11751,#11752,#11753,#11754,#11755,#11756,#11757,#11758,#11759,
#11760));
#3429=EDGE_LOOP('',(#11761,#11762,#11763,#11764));
#3430=EDGE_LOOP('',(#11765,#11766,#11767,#11768));
#3431=EDGE_LOOP('',(#11769,#11770,#11771,#11772));
#3432=EDGE_LOOP('',(#11773,#11774,#11775,#11776));
#3433=EDGE_LOOP('',(#11777,#11778,#11779,#11780));
#3434=EDGE_LOOP('',(#11781,#11782,#11783,#11784,#11785,#11786));
#3435=EDGE_LOOP('',(#11787,#11788,#11789,#11790));
#3436=EDGE_LOOP('',(#11791,#11792,#11793,#11794));
#3437=EDGE_LOOP('',(#11795,#11796,#11797,#11798));
#3438=EDGE_LOOP('',(#11799,#11800,#11801,#11802));
#3439=EDGE_LOOP('',(#11803,#11804,#11805,#11806));
#3440=EDGE_LOOP('',(#11807,#11808,#11809,#11810));
#3441=EDGE_LOOP('',(#11811,#11812,#11813,#11814,#11815,#11816,#11817,#11818,
#11819,#11820,#11821,#11822,#11823,#11824,#11825,#11826,#11827,#11828,#11829,
#11830));
#3442=EDGE_LOOP('',(#11831,#11832,#11833,#11834));
#3443=EDGE_LOOP('',(#11835,#11836,#11837,#11838));
#3444=EDGE_LOOP('',(#11839));
#3445=EDGE_LOOP('',(#11840));
#3446=EDGE_LOOP('',(#11841,#11842,#11843,#11844));
#3447=EDGE_LOOP('',(#11845));
#3448=EDGE_LOOP('',(#11846));
#3449=EDGE_LOOP('',(#11847,#11848,#11849,#11850));
#3450=EDGE_LOOP('',(#11851));
#3451=EDGE_LOOP('',(#11852));
#3452=EDGE_LOOP('',(#11853,#11854,#11855,#11856));
#3453=EDGE_LOOP('',(#11857));
#3454=EDGE_LOOP('',(#11858));
#3455=EDGE_LOOP('',(#11859,#11860,#11861,#11862));
#3456=EDGE_LOOP('',(#11863));
#3457=EDGE_LOOP('',(#11864));
#3458=EDGE_LOOP('',(#11865,#11866,#11867,#11868));
#3459=EDGE_LOOP('',(#11869,#11870,#11871,#11872));
#3460=EDGE_LOOP('',(#11873,#11874,#11875,#11876));
#3461=EDGE_LOOP('',(#11877,#11878,#11879,#11880));
#3462=EDGE_LOOP('',(#11881,#11882,#11883,#11884));
#3463=EDGE_LOOP('',(#11885,#11886,#11887,#11888));
#3464=EDGE_LOOP('',(#11889,#11890,#11891,#11892));
#3465=EDGE_LOOP('',(#11893,#11894,#11895,#11896,#11897,#11898));
#3466=EDGE_LOOP('',(#11899,#11900,#11901,#11902,#11903,#11904));
#3467=EDGE_LOOP('',(#11905));
#3468=EDGE_LOOP('',(#11906));
#3469=EDGE_LOOP('',(#11907,#11908,#11909,#11910));
#3470=EDGE_LOOP('',(#11911,#11912,#11913,#11914));
#3471=EDGE_LOOP('',(#11915,#11916,#11917,#11918));
#3472=EDGE_LOOP('',(#11919));
#3473=EDGE_LOOP('',(#11920));
#3474=EDGE_LOOP('',(#11921,#11922,#11923,#11924));
#3475=EDGE_LOOP('',(#11925,#11926,#11927,#11928));
#3476=EDGE_LOOP('',(#11929,#11930,#11931,#11932));
#3477=EDGE_LOOP('',(#11933,#11934,#11935,#11936));
#3478=EDGE_LOOP('',(#11937,#11938,#11939,#11940));
#3479=EDGE_LOOP('',(#11941,#11942,#11943,#11944));
#3480=EDGE_LOOP('',(#11945,#11946,#11947,#11948));
#3481=EDGE_LOOP('',(#11949,#11950,#11951,#11952));
#3482=EDGE_LOOP('',(#11953,#11954,#11955,#11956));
#3483=EDGE_LOOP('',(#11957,#11958,#11959,#11960));
#3484=EDGE_LOOP('',(#11961,#11962,#11963,#11964));
#3485=EDGE_LOOP('',(#11965,#11966,#11967,#11968));
#3486=EDGE_LOOP('',(#11969,#11970,#11971,#11972));
#3487=EDGE_LOOP('',(#11973,#11974,#11975,#11976));
#3488=EDGE_LOOP('',(#11977,#11978,#11979,#11980));
#3489=EDGE_LOOP('',(#11981,#11982,#11983,#11984));
#3490=EDGE_LOOP('',(#11985,#11986,#11987,#11988));
#3491=EDGE_LOOP('',(#11989,#11990,#11991,#11992));
#3492=EDGE_LOOP('',(#11993,#11994,#11995,#11996));
#3493=EDGE_LOOP('',(#11997,#11998,#11999,#12000));
#3494=EDGE_LOOP('',(#12001,#12002,#12003,#12004));
#3495=EDGE_LOOP('',(#12005,#12006,#12007,#12008));
#3496=EDGE_LOOP('',(#12009,#12010,#12011,#12012));
#3497=EDGE_LOOP('',(#12013,#12014,#12015,#12016));
#3498=EDGE_LOOP('',(#12017,#12018,#12019,#12020));
#3499=EDGE_LOOP('',(#12021,#12022,#12023,#12024));
#3500=EDGE_LOOP('',(#12025,#12026,#12027,#12028));
#3501=EDGE_LOOP('',(#12029,#12030,#12031,#12032));
#3502=EDGE_LOOP('',(#12033,#12034,#12035,#12036));
#3503=EDGE_LOOP('',(#12037,#12038,#12039,#12040));
#3504=EDGE_LOOP('',(#12041,#12042,#12043,#12044));
#3505=EDGE_LOOP('',(#12045,#12046,#12047,#12048));
#3506=EDGE_LOOP('',(#12049,#12050,#12051,#12052));
#3507=EDGE_LOOP('',(#12053,#12054,#12055,#12056));
#3508=EDGE_LOOP('',(#12057,#12058,#12059,#12060));
#3509=EDGE_LOOP('',(#12061,#12062,#12063,#12064));
#3510=EDGE_LOOP('',(#12065,#12066,#12067,#12068));
#3511=EDGE_LOOP('',(#12069,#12070,#12071,#12072));
#3512=EDGE_LOOP('',(#12073,#12074,#12075,#12076));
#3513=EDGE_LOOP('',(#12077,#12078,#12079,#12080));
#3514=EDGE_LOOP('',(#12081,#12082,#12083,#12084));
#3515=EDGE_LOOP('',(#12085,#12086,#12087,#12088));
#3516=EDGE_LOOP('',(#12089,#12090,#12091,#12092));
#3517=EDGE_LOOP('',(#12093,#12094,#12095,#12096));
#3518=EDGE_LOOP('',(#12097,#12098,#12099,#12100));
#3519=EDGE_LOOP('',(#12101,#12102,#12103,#12104));
#3520=EDGE_LOOP('',(#12105,#12106,#12107,#12108));
#3521=EDGE_LOOP('',(#12109,#12110,#12111,#12112));
#3522=EDGE_LOOP('',(#12113,#12114,#12115,#12116));
#3523=EDGE_LOOP('',(#12117,#12118,#12119,#12120));
#3524=EDGE_LOOP('',(#12121,#12122,#12123,#12124));
#3525=EDGE_LOOP('',(#12125,#12126,#12127,#12128));
#3526=EDGE_LOOP('',(#12129,#12130,#12131,#12132));
#3527=EDGE_LOOP('',(#12133,#12134,#12135,#12136));
#3528=EDGE_LOOP('',(#12137,#12138,#12139,#12140));
#3529=EDGE_LOOP('',(#12141,#12142,#12143,#12144));
#3530=EDGE_LOOP('',(#12145,#12146,#12147,#12148));
#3531=EDGE_LOOP('',(#12149,#12150,#12151,#12152));
#3532=EDGE_LOOP('',(#12153,#12154,#12155,#12156));
#3533=EDGE_LOOP('',(#12157,#12158,#12159,#12160));
#3534=EDGE_LOOP('',(#12161,#12162,#12163,#12164));
#3535=EDGE_LOOP('',(#12165,#12166,#12167,#12168));
#3536=EDGE_LOOP('',(#12169,#12170,#12171,#12172));
#3537=EDGE_LOOP('',(#12173,#12174,#12175,#12176));
#3538=EDGE_LOOP('',(#12177,#12178,#12179,#12180));
#3539=EDGE_LOOP('',(#12181,#12182,#12183,#12184));
#3540=EDGE_LOOP('',(#12185,#12186,#12187,#12188));
#3541=EDGE_LOOP('',(#12189,#12190,#12191,#12192));
#3542=EDGE_LOOP('',(#12193,#12194,#12195,#12196));
#3543=EDGE_LOOP('',(#12197,#12198,#12199,#12200));
#3544=EDGE_LOOP('',(#12201,#12202,#12203,#12204));
#3545=EDGE_LOOP('',(#12205,#12206,#12207,#12208));
#3546=EDGE_LOOP('',(#12209,#12210,#12211,#12212));
#3547=EDGE_LOOP('',(#12213,#12214,#12215,#12216));
#3548=EDGE_LOOP('',(#12217,#12218,#12219,#12220));
#3549=EDGE_LOOP('',(#12221,#12222,#12223,#12224));
#3550=EDGE_LOOP('',(#12225,#12226,#12227,#12228));
#3551=EDGE_LOOP('',(#12229,#12230,#12231,#12232));
#3552=EDGE_LOOP('',(#12233,#12234,#12235,#12236));
#3553=EDGE_LOOP('',(#12237,#12238,#12239,#12240));
#3554=EDGE_LOOP('',(#12241,#12242,#12243,#12244));
#3555=EDGE_LOOP('',(#12245,#12246,#12247,#12248));
#3556=EDGE_LOOP('',(#12249,#12250,#12251,#12252));
#3557=EDGE_LOOP('',(#12253,#12254,#12255,#12256));
#3558=EDGE_LOOP('',(#12257,#12258,#12259,#12260));
#3559=EDGE_LOOP('',(#12261,#12262,#12263,#12264));
#3560=EDGE_LOOP('',(#12265,#12266,#12267,#12268));
#3561=EDGE_LOOP('',(#12269,#12270,#12271,#12272));
#3562=EDGE_LOOP('',(#12273,#12274,#12275,#12276));
#3563=EDGE_LOOP('',(#12277,#12278,#12279,#12280));
#3564=EDGE_LOOP('',(#12281,#12282,#12283,#12284));
#3565=EDGE_LOOP('',(#12285,#12286,#12287,#12288));
#3566=EDGE_LOOP('',(#12289,#12290,#12291,#12292));
#3567=EDGE_LOOP('',(#12293,#12294,#12295,#12296));
#3568=EDGE_LOOP('',(#12297,#12298,#12299,#12300));
#3569=EDGE_LOOP('',(#12301,#12302,#12303,#12304));
#3570=EDGE_LOOP('',(#12305,#12306,#12307,#12308));
#3571=EDGE_LOOP('',(#12309,#12310,#12311,#12312));
#3572=EDGE_LOOP('',(#12313,#12314,#12315,#12316));
#3573=EDGE_LOOP('',(#12317,#12318,#12319,#12320));
#3574=EDGE_LOOP('',(#12321,#12322,#12323,#12324));
#3575=EDGE_LOOP('',(#12325,#12326,#12327,#12328));
#3576=EDGE_LOOP('',(#12329,#12330,#12331,#12332));
#3577=EDGE_LOOP('',(#12333,#12334,#12335,#12336));
#3578=EDGE_LOOP('',(#12337,#12338,#12339,#12340));
#3579=EDGE_LOOP('',(#12341,#12342,#12343,#12344));
#3580=EDGE_LOOP('',(#12345,#12346,#12347,#12348));
#3581=EDGE_LOOP('',(#12349,#12350,#12351,#12352));
#3582=EDGE_LOOP('',(#12353,#12354,#12355,#12356));
#3583=EDGE_LOOP('',(#12357,#12358,#12359,#12360));
#3584=EDGE_LOOP('',(#12361,#12362,#12363,#12364));
#3585=EDGE_LOOP('',(#12365,#12366,#12367,#12368));
#3586=EDGE_LOOP('',(#12369,#12370,#12371,#12372));
#3587=EDGE_LOOP('',(#12373,#12374,#12375,#12376));
#3588=EDGE_LOOP('',(#12377,#12378,#12379,#12380));
#3589=EDGE_LOOP('',(#12381,#12382,#12383,#12384));
#3590=EDGE_LOOP('',(#12385,#12386,#12387,#12388));
#3591=EDGE_LOOP('',(#12389,#12390,#12391,#12392));
#3592=EDGE_LOOP('',(#12393,#12394,#12395,#12396));
#3593=EDGE_LOOP('',(#12397,#12398,#12399,#12400));
#3594=EDGE_LOOP('',(#12401,#12402,#12403,#12404));
#3595=EDGE_LOOP('',(#12405,#12406,#12407,#12408));
#3596=EDGE_LOOP('',(#12409,#12410,#12411,#12412));
#3597=EDGE_LOOP('',(#12413,#12414,#12415,#12416));
#3598=EDGE_LOOP('',(#12417,#12418,#12419,#12420));
#3599=EDGE_LOOP('',(#12421,#12422,#12423,#12424));
#3600=EDGE_LOOP('',(#12425,#12426,#12427,#12428));
#3601=EDGE_LOOP('',(#12429,#12430,#12431,#12432));
#3602=EDGE_LOOP('',(#12433,#12434,#12435,#12436));
#3603=EDGE_LOOP('',(#12437,#12438,#12439,#12440));
#3604=EDGE_LOOP('',(#12441,#12442,#12443,#12444));
#3605=EDGE_LOOP('',(#12445,#12446,#12447,#12448,#12449,#12450,#12451,#12452));
#3606=EDGE_LOOP('',(#12453));
#3607=EDGE_LOOP('',(#12454));
#3608=EDGE_LOOP('',(#12455));
#3609=EDGE_LOOP('',(#12456,#12457,#12458,#12459));
#3610=EDGE_LOOP('',(#12460,#12461,#12462,#12463,#12464,#12465,#12466,#12467));
#3611=EDGE_LOOP('',(#12468,#12469,#12470,#12471));
#3612=EDGE_LOOP('',(#12472,#12473,#12474,#12475));
#3613=EDGE_LOOP('',(#12476,#12477,#12478,#12479));
#3614=EDGE_LOOP('',(#12480,#12481,#12482,#12483));
#3615=EDGE_LOOP('',(#12484,#12485,#12486,#12487));
#3616=EDGE_LOOP('',(#12488,#12489,#12490,#12491));
#3617=EDGE_LOOP('',(#12492,#12493,#12494,#12495));
#3618=EDGE_LOOP('',(#12496,#12497,#12498,#12499));
#3619=EDGE_LOOP('',(#12500,#12501,#12502,#12503));
#3620=EDGE_LOOP('',(#12504,#12505,#12506,#12507));
#3621=EDGE_LOOP('',(#12508,#12509,#12510,#12511));
#3622=EDGE_LOOP('',(#12512,#12513,#12514,#12515));
#3623=EDGE_LOOP('',(#12516,#12517,#12518,#12519));
#3624=EDGE_LOOP('',(#12520,#12521,#12522,#12523));
#3625=EDGE_LOOP('',(#12524));
#3626=EDGE_LOOP('',(#12525));
#3627=EDGE_LOOP('',(#12526));
#3628=EDGE_LOOP('',(#12527,#12528,#12529,#12530));
#3629=EDGE_LOOP('',(#12531,#12532,#12533,#12534));
#3630=EDGE_LOOP('',(#12535,#12536,#12537,#12538));
#3631=EDGE_LOOP('',(#12539,#12540,#12541,#12542));
#3632=EDGE_LOOP('',(#12543,#12544,#12545,#12546));
#3633=EDGE_LOOP('',(#12547,#12548,#12549,#12550));
#3634=EDGE_LOOP('',(#12551,#12552,#12553,#12554));
#3635=EDGE_LOOP('',(#12555,#12556,#12557,#12558));
#3636=EDGE_LOOP('',(#12559,#12560,#12561,#12562));
#3637=EDGE_LOOP('',(#12563,#12564,#12565,#12566));
#3638=EDGE_LOOP('',(#12567,#12568,#12569,#12570));
#3639=EDGE_LOOP('',(#12571,#12572,#12573,#12574));
#3640=EDGE_LOOP('',(#12575,#12576,#12577,#12578));
#3641=EDGE_LOOP('',(#12579));
#3642=EDGE_LOOP('',(#12580));
#3643=EDGE_LOOP('',(#12581));
#3644=EDGE_LOOP('',(#12582));
#3645=EDGE_LOOP('',(#12583,#12584,#12585,#12586));
#3646=EDGE_LOOP('',(#12587,#12588,#12589,#12590));
#3647=EDGE_LOOP('',(#12591));
#3648=EDGE_LOOP('',(#12592));
#3649=EDGE_LOOP('',(#12593));
#3650=EDGE_LOOP('',(#12594));
#3651=EDGE_LOOP('',(#12595,#12596,#12597,#12598));
#3652=EDGE_LOOP('',(#12599,#12600,#12601,#12602));
#3653=EDGE_LOOP('',(#12603,#12604,#12605,#12606));
#3654=EDGE_LOOP('',(#12607,#12608,#12609,#12610));
#3655=EDGE_LOOP('',(#12611,#12612,#12613,#12614));
#3656=EDGE_LOOP('',(#12615,#12616,#12617,#12618));
#3657=EDGE_LOOP('',(#12619,#12620,#12621,#12622));
#3658=EDGE_LOOP('',(#12623,#12624,#12625,#12626));
#3659=EDGE_LOOP('',(#12627,#12628,#12629,#12630));
#3660=EDGE_LOOP('',(#12631,#12632,#12633,#12634));
#3661=EDGE_LOOP('',(#12635,#12636,#12637,#12638));
#3662=EDGE_LOOP('',(#12639,#12640,#12641,#12642));
#3663=EDGE_LOOP('',(#12643,#12644,#12645,#12646));
#3664=EDGE_LOOP('',(#12647,#12648,#12649,#12650));
#3665=EDGE_LOOP('',(#12651,#12652,#12653,#12654));
#3666=EDGE_LOOP('',(#12655,#12656,#12657,#12658));
#3667=EDGE_LOOP('',(#12659,#12660,#12661,#12662));
#3668=EDGE_LOOP('',(#12663,#12664,#12665,#12666));
#3669=EDGE_LOOP('',(#12667,#12668,#12669,#12670,#12671,#12672));
#3670=EDGE_LOOP('',(#12673,#12674,#12675,#12676,#12677,#12678));
#3671=EDGE_LOOP('',(#12679));
#3672=EDGE_LOOP('',(#12680));
#3673=EDGE_LOOP('',(#12681,#12682,#12683,#12684));
#3674=EDGE_LOOP('',(#12685));
#3675=EDGE_LOOP('',(#12686));
#3676=EDGE_LOOP('',(#12687,#12688,#12689,#12690));
#3677=EDGE_LOOP('',(#12691,#12692,#12693,#12694));
#3678=EDGE_LOOP('',(#12695,#12696,#12697,#12698));
#3679=EDGE_LOOP('',(#12699));
#3680=EDGE_LOOP('',(#12700));
#3681=EDGE_LOOP('',(#12701,#12702,#12703,#12704));
#3682=EDGE_LOOP('',(#12705,#12706,#12707,#12708));
#3683=EDGE_LOOP('',(#12709,#12710,#12711,#12712));
#3684=EDGE_LOOP('',(#12713));
#3685=EDGE_LOOP('',(#12714,#12715,#12716,#12717));
#3686=EDGE_LOOP('',(#12718,#12719,#12720,#12721));
#3687=EDGE_LOOP('',(#12722,#12723,#12724,#12725));
#3688=EDGE_LOOP('',(#12726,#12727,#12728,#12729));
#3689=EDGE_LOOP('',(#12730,#12731,#12732,#12733));
#3690=EDGE_LOOP('',(#12734,#12735,#12736,#12737));
#3691=EDGE_LOOP('',(#12738,#12739,#12740,#12741));
#3692=EDGE_LOOP('',(#12742,#12743,#12744,#12745));
#3693=EDGE_LOOP('',(#12746,#12747,#12748,#12749));
#3694=EDGE_LOOP('',(#12750,#12751,#12752,#12753));
#3695=EDGE_LOOP('',(#12754));
#3696=EDGE_LOOP('',(#12755));
#3697=EDGE_LOOP('',(#12756));
#3698=EDGE_LOOP('',(#12757));
#3699=EDGE_LOOP('',(#12758,#12759,#12760,#12761));
#3700=EDGE_LOOP('',(#12762,#12763,#12764,#12765));
#3701=EDGE_LOOP('',(#12766,#12767,#12768,#12769));
#3702=EDGE_LOOP('',(#12770,#12771,#12772,#12773));
#3703=EDGE_LOOP('',(#12774,#12775,#12776,#12777));
#3704=EDGE_LOOP('',(#12778));
#3705=EDGE_LOOP('',(#12779));
#3706=EDGE_LOOP('',(#12780));
#3707=EDGE_LOOP('',(#12781,#12782,#12783,#12784));
#3708=EDGE_LOOP('',(#12785,#12786,#12787,#12788));
#3709=EDGE_LOOP('',(#12789));
#3710=EDGE_LOOP('',(#12790));
#3711=EDGE_LOOP('',(#12791));
#3712=EDGE_LOOP('',(#12792));
#3713=EDGE_LOOP('',(#12793,#12794,#12795,#12796));
#3714=EDGE_LOOP('',(#12797,#12798,#12799,#12800));
#3715=EDGE_LOOP('',(#12801));
#3716=EDGE_LOOP('',(#12802));
#3717=EDGE_LOOP('',(#12803));
#3718=EDGE_LOOP('',(#12804));
#3719=EDGE_LOOP('',(#12805,#12806));
#3720=EDGE_LOOP('',(#12807,#12808,#12809,#12810,#12811,#12812,#12813,#12814,
#12815));
#3721=EDGE_LOOP('',(#12816,#12817,#12818));
#3722=EDGE_LOOP('',(#12819,#12820,#12821,#12822));
#3723=EDGE_LOOP('',(#12823,#12824,#12825,#12826));
#3724=EDGE_LOOP('',(#12827,#12828,#12829,#12830));
#3725=EDGE_LOOP('',(#12831,#12832));
#3726=EDGE_LOOP('',(#12833));
#3727=EDGE_LOOP('',(#12834));
#3728=EDGE_LOOP('',(#12835));
#3729=EDGE_LOOP('',(#12836));
#3730=EDGE_LOOP('',(#12837,#12838,#12839,#12840));
#3731=EDGE_LOOP('',(#12841,#12842,#12843,#12844));
#3732=EDGE_LOOP('',(#12845,#12846,#12847,#12848));
#3733=EDGE_LOOP('',(#12849,#12850,#12851,#12852));
#3734=EDGE_LOOP('',(#12853));
#3735=EDGE_LOOP('',(#12854,#12855,#12856,#12857));
#3736=EDGE_LOOP('',(#12858,#12859,#12860,#12861));
#3737=EDGE_LOOP('',(#12862,#12863,#12864,#12865));
#3738=EDGE_LOOP('',(#12866,#12867,#12868,#12869));
#3739=EDGE_LOOP('',(#12870));
#3740=EDGE_LOOP('',(#12871,#12872,#12873,#12874));
#3741=EDGE_LOOP('',(#12875,#12876,#12877,#12878));
#3742=EDGE_LOOP('',(#12879));
#3743=EDGE_LOOP('',(#12880,#12881,#12882,#12883));
#3744=EDGE_LOOP('',(#12884,#12885,#12886,#12887));
#3745=EDGE_LOOP('',(#12888,#12889,#12890,#12891));
#3746=EDGE_LOOP('',(#12892));
#3747=EDGE_LOOP('',(#12893,#12894,#12895,#12896));
#3748=EDGE_LOOP('',(#12897,#12898,#12899,#12900));
#3749=EDGE_LOOP('',(#12901,#12902,#12903,#12904));
#3750=EDGE_LOOP('',(#12905));
#3751=EDGE_LOOP('',(#12906));
#3752=EDGE_LOOP('',(#12907));
#3753=EDGE_LOOP('',(#12908));
#3754=EDGE_LOOP('',(#12909,#12910,#12911,#12912));
#3755=EDGE_LOOP('',(#12913,#12914,#12915,#12916));
#3756=EDGE_LOOP('',(#12917));
#3757=EDGE_LOOP('',(#12918));
#3758=EDGE_LOOP('',(#12919));
#3759=EDGE_LOOP('',(#12920));
#3760=EDGE_LOOP('',(#12921,#12922,#12923,#12924));
#3761=EDGE_LOOP('',(#12925,#12926,#12927,#12928));
#3762=EDGE_LOOP('',(#12929));
#3763=EDGE_LOOP('',(#12930));
#3764=EDGE_LOOP('',(#12931));
#3765=EDGE_LOOP('',(#12932));
#3766=EDGE_LOOP('',(#12933,#12934,#12935,#12936));
#3767=EDGE_LOOP('',(#12937,#12938,#12939,#12940));
#3768=EDGE_LOOP('',(#12941));
#3769=EDGE_LOOP('',(#12942));
#3770=EDGE_LOOP('',(#12943));
#3771=EDGE_LOOP('',(#12944));
#3772=EDGE_LOOP('',(#12945,#12946,#12947,#12948));
#3773=EDGE_LOOP('',(#12949,#12950,#12951,#12952));
#3774=EDGE_LOOP('',(#12953));
#3775=EDGE_LOOP('',(#12954));
#3776=EDGE_LOOP('',(#12955));
#3777=EDGE_LOOP('',(#12956));
#3778=EDGE_LOOP('',(#12957,#12958,#12959,#12960));
#3779=EDGE_LOOP('',(#12961,#12962,#12963,#12964));
#3780=EDGE_LOOP('',(#12965,#12966,#12967,#12968));
#3781=EDGE_LOOP('',(#12969,#12970,#12971,#12972));
#3782=EDGE_LOOP('',(#12973,#12974,#12975,#12976));
#3783=EDGE_LOOP('',(#12977,#12978,#12979,#12980));
#3784=EDGE_LOOP('',(#12981,#12982,#12983,#12984,#12985,#12986));
#3785=EDGE_LOOP('',(#12987,#12988,#12989,#12990,#12991,#12992));
#3786=EDGE_LOOP('',(#12993));
#3787=EDGE_LOOP('',(#12994));
#3788=EDGE_LOOP('',(#12995,#12996,#12997,#12998));
#3789=EDGE_LOOP('',(#12999));
#3790=EDGE_LOOP('',(#13000));
#3791=EDGE_LOOP('',(#13001,#13002,#13003,#13004));
#3792=EDGE_LOOP('',(#13005,#13006,#13007,#13008));
#3793=EDGE_LOOP('',(#13009,#13010,#13011,#13012));
#3794=EDGE_LOOP('',(#13013));
#3795=EDGE_LOOP('',(#13014));
#3796=EDGE_LOOP('',(#13015,#13016,#13017,#13018));
#3797=EDGE_LOOP('',(#13019,#13020,#13021,#13022));
#3798=EDGE_LOOP('',(#13023,#13024,#13025,#13026));
#3799=EDGE_LOOP('',(#13027));
#3800=EDGE_LOOP('',(#13028,#13029,#13030,#13031));
#3801=EDGE_LOOP('',(#13032,#13033,#13034,#13035));
#3802=EDGE_LOOP('',(#13036,#13037,#13038,#13039));
#3803=EDGE_LOOP('',(#13040,#13041,#13042,#13043));
#3804=EDGE_LOOP('',(#13044,#13045,#13046,#13047));
#3805=EDGE_LOOP('',(#13048));
#3806=EDGE_LOOP('',(#13049));
#3807=EDGE_LOOP('',(#13050));
#3808=EDGE_LOOP('',(#13051));
#3809=EDGE_LOOP('',(#13052,#13053,#13054,#13055));
#3810=EDGE_LOOP('',(#13056,#13057,#13058,#13059));
#3811=EDGE_LOOP('',(#13060,#13061,#13062,#13063));
#3812=EDGE_LOOP('',(#13064,#13065,#13066,#13067));
#3813=EDGE_LOOP('',(#13068));
#3814=EDGE_LOOP('',(#13069));
#3815=EDGE_LOOP('',(#13070));
#3816=EDGE_LOOP('',(#13071,#13072,#13073,#13074));
#3817=EDGE_LOOP('',(#13075,#13076,#13077,#13078));
#3818=EDGE_LOOP('',(#13079));
#3819=EDGE_LOOP('',(#13080));
#3820=EDGE_LOOP('',(#13081));
#3821=EDGE_LOOP('',(#13082));
#3822=EDGE_LOOP('',(#13083,#13084,#13085,#13086));
#3823=EDGE_LOOP('',(#13087,#13088,#13089,#13090));
#3824=EDGE_LOOP('',(#13091));
#3825=EDGE_LOOP('',(#13092));
#3826=EDGE_LOOP('',(#13093));
#3827=EDGE_LOOP('',(#13094));
#3828=EDGE_LOOP('',(#13095,#13096));
#3829=EDGE_LOOP('',(#13097,#13098,#13099,#13100,#13101,#13102,#13103,#13104,
#13105));
#3830=EDGE_LOOP('',(#13106,#13107,#13108));
#3831=EDGE_LOOP('',(#13109,#13110,#13111,#13112));
#3832=EDGE_LOOP('',(#13113,#13114,#13115,#13116));
#3833=EDGE_LOOP('',(#13117,#13118,#13119,#13120));
#3834=EDGE_LOOP('',(#13121,#13122));
#3835=EDGE_LOOP('',(#13123));
#3836=EDGE_LOOP('',(#13124));
#3837=EDGE_LOOP('',(#13125));
#3838=EDGE_LOOP('',(#13126));
#3839=EDGE_LOOP('',(#13127,#13128,#13129,#13130));
#3840=EDGE_LOOP('',(#13131,#13132,#13133,#13134));
#3841=EDGE_LOOP('',(#13135));
#3842=EDGE_LOOP('',(#13136));
#3843=EDGE_LOOP('',(#13137));
#3844=EDGE_LOOP('',(#13138));
#3845=EDGE_LOOP('',(#13139,#13140,#13141,#13142));
#3846=EDGE_LOOP('',(#13143));
#3847=EDGE_LOOP('',(#13144,#13145,#13146,#13147));
#3848=EDGE_LOOP('',(#13148,#13149,#13150,#13151));
#3849=EDGE_LOOP('',(#13152,#13153,#13154,#13155));
#3850=EDGE_LOOP('',(#13156,#13157,#13158,#13159));
#3851=EDGE_LOOP('',(#13160,#13161,#13162,#13163));
#3852=EDGE_LOOP('',(#13164));
#3853=EDGE_LOOP('',(#13165));
#3854=EDGE_LOOP('',(#13166));
#3855=EDGE_LOOP('',(#13167));
#3856=EDGE_LOOP('',(#13168,#13169,#13170,#13171));
#3857=EDGE_LOOP('',(#13172,#13173,#13174,#13175));
#3858=EDGE_LOOP('',(#13176,#13177,#13178,#13179));
#3859=EDGE_LOOP('',(#13180,#13181,#13182,#13183));
#3860=EDGE_LOOP('',(#13184));
#3861=EDGE_LOOP('',(#13185));
#3862=EDGE_LOOP('',(#13186));
#3863=EDGE_LOOP('',(#13187,#13188,#13189,#13190));
#3864=EDGE_LOOP('',(#13191,#13192,#13193,#13194));
#3865=EDGE_LOOP('',(#13195));
#3866=EDGE_LOOP('',(#13196));
#3867=EDGE_LOOP('',(#13197));
#3868=EDGE_LOOP('',(#13198));
#3869=EDGE_LOOP('',(#13199,#13200,#13201,#13202));
#3870=EDGE_LOOP('',(#13203,#13204,#13205,#13206));
#3871=EDGE_LOOP('',(#13207));
#3872=EDGE_LOOP('',(#13208));
#3873=EDGE_LOOP('',(#13209));
#3874=EDGE_LOOP('',(#13210));
#3875=EDGE_LOOP('',(#13211,#13212));
#3876=EDGE_LOOP('',(#13213,#13214,#13215,#13216,#13217,#13218,#13219,#13220,
#13221));
#3877=EDGE_LOOP('',(#13222,#13223,#13224));
#3878=EDGE_LOOP('',(#13225,#13226,#13227,#13228));
#3879=EDGE_LOOP('',(#13229,#13230,#13231,#13232));
#3880=EDGE_LOOP('',(#13233,#13234,#13235,#13236));
#3881=EDGE_LOOP('',(#13237,#13238));
#3882=EDGE_LOOP('',(#13239));
#3883=EDGE_LOOP('',(#13240));
#3884=EDGE_LOOP('',(#13241));
#3885=EDGE_LOOP('',(#13242));
#3886=EDGE_LOOP('',(#13243,#13244,#13245,#13246));
#3887=EDGE_LOOP('',(#13247,#13248,#13249,#13250));
#3888=EDGE_LOOP('',(#13251));
#3889=EDGE_LOOP('',(#13252));
#3890=EDGE_LOOP('',(#13253));
#3891=EDGE_LOOP('',(#13254));
#3892=EDGE_LOOP('',(#13255,#13256,#13257,#13258));
#3893=EDGE_LOOP('',(#13259,#13260,#13261,#13262));
#3894=EDGE_LOOP('',(#13263,#13264,#13265,#13266));
#3895=EDGE_LOOP('',(#13267,#13268,#13269,#13270,#13271,#13272,#13273,#13274,
#13275,#13276,#13277,#13278,#13279,#13280,#13281,#13282,#13283,#13284,#13285,
#13286,#13287,#13288,#13289,#13290,#13291,#13292,#13293,#13294,#13295,#13296,
#13297,#13298,#13299,#13300,#13301,#13302,#13303,#13304,#13305,#13306,#13307,
#13308,#13309,#13310,#13311,#13312,#13313,#13314,#13315,#13316,#13317,#13318,
#13319,#13320,#13321,#13322,#13323,#13324,#13325,#13326,#13327,#13328,#13329,
#13330,#13331,#13332,#13333,#13334,#13335,#13336,#13337,#13338,#13339,#13340,
#13341,#13342,#13343,#13344,#13345,#13346));
#3896=EDGE_LOOP('',(#13347,#13348,#13349,#13350));
#3897=EDGE_LOOP('',(#13351,#13352,#13353,#13354));
#3898=EDGE_LOOP('',(#13355,#13356,#13357,#13358));
#3899=EDGE_LOOP('',(#13359));
#3900=EDGE_LOOP('',(#13360,#13361,#13362,#13363));
#3901=EDGE_LOOP('',(#13364,#13365,#13366,#13367));
#3902=EDGE_LOOP('',(#13368,#13369,#13370,#13371));
#3903=EDGE_LOOP('',(#13372,#13373,#13374,#13375));
#3904=EDGE_LOOP('',(#13376,#13377,#13378,#13379));
#3905=EDGE_LOOP('',(#13380,#13381,#13382,#13383));
#3906=EDGE_LOOP('',(#13384,#13385,#13386,#13387));
#3907=EDGE_LOOP('',(#13388,#13389,#13390,#13391));
#3908=EDGE_LOOP('',(#13392,#13393,#13394,#13395));
#3909=EDGE_LOOP('',(#13396,#13397,#13398,#13399));
#3910=EDGE_LOOP('',(#13400,#13401,#13402,#13403));
#3911=EDGE_LOOP('',(#13404,#13405,#13406,#13407));
#3912=EDGE_LOOP('',(#13408,#13409,#13410,#13411));
#3913=EDGE_LOOP('',(#13412,#13413,#13414,#13415));
#3914=EDGE_LOOP('',(#13416,#13417,#13418,#13419));
#3915=EDGE_LOOP('',(#13420,#13421,#13422,#13423));
#3916=EDGE_LOOP('',(#13424,#13425,#13426,#13427));
#3917=EDGE_LOOP('',(#13428,#13429,#13430,#13431));
#3918=EDGE_LOOP('',(#13432,#13433,#13434,#13435));
#3919=EDGE_LOOP('',(#13436,#13437,#13438,#13439));
#3920=EDGE_LOOP('',(#13440,#13441,#13442,#13443));
#3921=EDGE_LOOP('',(#13444,#13445,#13446,#13447));
#3922=EDGE_LOOP('',(#13448,#13449,#13450,#13451));
#3923=EDGE_LOOP('',(#13452,#13453,#13454,#13455));
#3924=EDGE_LOOP('',(#13456,#13457,#13458,#13459));
#3925=EDGE_LOOP('',(#13460,#13461,#13462,#13463));
#3926=EDGE_LOOP('',(#13464,#13465,#13466,#13467));
#3927=EDGE_LOOP('',(#13468,#13469,#13470,#13471));
#3928=EDGE_LOOP('',(#13472,#13473,#13474,#13475));
#3929=EDGE_LOOP('',(#13476,#13477,#13478,#13479));
#3930=EDGE_LOOP('',(#13480,#13481,#13482,#13483));
#3931=EDGE_LOOP('',(#13484,#13485,#13486,#13487));
#3932=EDGE_LOOP('',(#13488,#13489,#13490,#13491));
#3933=EDGE_LOOP('',(#13492,#13493,#13494,#13495));
#3934=EDGE_LOOP('',(#13496,#13497,#13498,#13499));
#3935=EDGE_LOOP('',(#13500,#13501,#13502,#13503));
#3936=EDGE_LOOP('',(#13504,#13505,#13506,#13507));
#3937=EDGE_LOOP('',(#13508,#13509,#13510,#13511));
#3938=EDGE_LOOP('',(#13512,#13513,#13514,#13515));
#3939=EDGE_LOOP('',(#13516,#13517,#13518,#13519));
#3940=EDGE_LOOP('',(#13520,#13521,#13522,#13523));
#3941=EDGE_LOOP('',(#13524,#13525,#13526,#13527));
#3942=EDGE_LOOP('',(#13528,#13529,#13530,#13531));
#3943=EDGE_LOOP('',(#13532,#13533,#13534,#13535));
#3944=EDGE_LOOP('',(#13536,#13537,#13538,#13539));
#3945=EDGE_LOOP('',(#13540,#13541,#13542,#13543));
#3946=EDGE_LOOP('',(#13544,#13545,#13546,#13547));
#3947=EDGE_LOOP('',(#13548,#13549,#13550,#13551));
#3948=EDGE_LOOP('',(#13552,#13553,#13554,#13555));
#3949=EDGE_LOOP('',(#13556,#13557,#13558,#13559));
#3950=EDGE_LOOP('',(#13560,#13561,#13562,#13563));
#3951=EDGE_LOOP('',(#13564,#13565,#13566,#13567));
#3952=EDGE_LOOP('',(#13568,#13569,#13570,#13571));
#3953=EDGE_LOOP('',(#13572,#13573,#13574,#13575));
#3954=EDGE_LOOP('',(#13576,#13577,#13578,#13579));
#3955=EDGE_LOOP('',(#13580,#13581,#13582,#13583));
#3956=EDGE_LOOP('',(#13584,#13585,#13586,#13587));
#3957=EDGE_LOOP('',(#13588,#13589,#13590,#13591));
#3958=EDGE_LOOP('',(#13592,#13593,#13594,#13595));
#3959=EDGE_LOOP('',(#13596,#13597,#13598,#13599));
#3960=EDGE_LOOP('',(#13600,#13601,#13602,#13603));
#3961=EDGE_LOOP('',(#13604,#13605,#13606,#13607));
#3962=EDGE_LOOP('',(#13608,#13609,#13610,#13611));
#3963=EDGE_LOOP('',(#13612,#13613,#13614,#13615));
#3964=EDGE_LOOP('',(#13616,#13617,#13618,#13619));
#3965=EDGE_LOOP('',(#13620,#13621,#13622,#13623));
#3966=EDGE_LOOP('',(#13624,#13625,#13626,#13627));
#3967=EDGE_LOOP('',(#13628,#13629,#13630,#13631));
#3968=EDGE_LOOP('',(#13632,#13633,#13634,#13635));
#3969=EDGE_LOOP('',(#13636,#13637,#13638,#13639));
#3970=EDGE_LOOP('',(#13640,#13641,#13642,#13643));
#3971=EDGE_LOOP('',(#13644,#13645,#13646,#13647));
#3972=EDGE_LOOP('',(#13648,#13649,#13650,#13651));
#3973=EDGE_LOOP('',(#13652,#13653,#13654,#13655));
#3974=EDGE_LOOP('',(#13656,#13657,#13658,#13659));
#3975=EDGE_LOOP('',(#13660,#13661,#13662,#13663));
#3976=EDGE_LOOP('',(#13664,#13665,#13666,#13667));
#3977=EDGE_LOOP('',(#13668,#13669,#13670,#13671));
#3978=EDGE_LOOP('',(#13672,#13673,#13674,#13675));
#3979=EDGE_LOOP('',(#13676,#13677,#13678,#13679));
#3980=EDGE_LOOP('',(#13680,#13681,#13682,#13683,#13684,#13685,#13686,#13687,
#13688,#13689,#13690,#13691,#13692,#13693,#13694,#13695,#13696,#13697,#13698,
#13699,#13700,#13701,#13702,#13703,#13704,#13705,#13706,#13707,#13708,#13709,
#13710,#13711,#13712,#13713,#13714,#13715,#13716,#13717,#13718,#13719,#13720,
#13721,#13722,#13723,#13724,#13725,#13726,#13727,#13728,#13729,#13730,#13731,
#13732,#13733,#13734,#13735,#13736,#13737,#13738,#13739,#13740,#13741,#13742,
#13743,#13744,#13745,#13746,#13747,#13748,#13749,#13750,#13751,#13752,#13753,
#13754,#13755,#13756,#13757,#13758,#13759));
#3981=EDGE_LOOP('',(#13760));
#3982=EDGE_LOOP('',(#13761,#13762,#13763,#13764));
#3983=EDGE_LOOP('',(#13765,#13766,#13767,#13768,#13769,#13770,#13771,#13772));
#3984=EDGE_LOOP('',(#13773,#13774,#13775,#13776));
#3985=EDGE_LOOP('',(#13777,#13778,#13779,#13780));
#3986=EDGE_LOOP('',(#13781,#13782,#13783,#13784));
#3987=EDGE_LOOP('',(#13785,#13786,#13787,#13788));
#3988=EDGE_LOOP('',(#13789,#13790,#13791,#13792,#13793,#13794,#13795,#13796));
#3989=EDGE_LOOP('',(#13797,#13798,#13799,#13800));
#3990=EDGE_LOOP('',(#13801,#13802,#13803,#13804));
#3991=EDGE_LOOP('',(#13805,#13806,#13807,#13808));
#3992=EDGE_LOOP('',(#13809,#13810,#13811,#13812));
#3993=EDGE_LOOP('',(#13813,#13814,#13815,#13816));
#3994=EDGE_LOOP('',(#13817));
#3995=EDGE_LOOP('',(#13818,#13819,#13820,#13821));
#3996=EDGE_LOOP('',(#13822,#13823,#13824,#13825));
#3997=EDGE_LOOP('',(#13826,#13827,#13828,#13829));
#3998=EDGE_LOOP('',(#13830,#13831,#13832,#13833));
#3999=EDGE_LOOP('',(#13834,#13835,#13836,#13837));
#4000=EDGE_LOOP('',(#13838));
#4001=EDGE_LOOP('',(#13839));
#4002=EDGE_LOOP('',(#13840));
#4003=EDGE_LOOP('',(#13841));
#4004=EDGE_LOOP('',(#13842,#13843,#13844,#13845));
#4005=EDGE_LOOP('',(#13846,#13847,#13848,#13849));
#4006=EDGE_LOOP('',(#13850,#13851,#13852,#13853));
#4007=EDGE_LOOP('',(#13854,#13855,#13856,#13857));
#4008=EDGE_LOOP('',(#13858));
#4009=EDGE_LOOP('',(#13859));
#4010=EDGE_LOOP('',(#13860));
#4011=EDGE_LOOP('',(#13861,#13862,#13863,#13864));
#4012=EDGE_LOOP('',(#13865,#13866,#13867,#13868));
#4013=EDGE_LOOP('',(#13869));
#4014=EDGE_LOOP('',(#13870));
#4015=EDGE_LOOP('',(#13871));
#4016=EDGE_LOOP('',(#13872));
#4017=EDGE_LOOP('',(#13873,#13874,#13875,#13876));
#4018=EDGE_LOOP('',(#13877,#13878,#13879,#13880));
#4019=EDGE_LOOP('',(#13881));
#4020=EDGE_LOOP('',(#13882));
#4021=EDGE_LOOP('',(#13883));
#4022=EDGE_LOOP('',(#13884));
#4023=EDGE_LOOP('',(#13885,#13886));
#4024=EDGE_LOOP('',(#13887,#13888,#13889,#13890,#13891,#13892,#13893,#13894,
#13895));
#4025=EDGE_LOOP('',(#13896,#13897,#13898));
#4026=EDGE_LOOP('',(#13899,#13900,#13901,#13902));
#4027=EDGE_LOOP('',(#13903,#13904,#13905,#13906));
#4028=EDGE_LOOP('',(#13907,#13908,#13909,#13910));
#4029=EDGE_LOOP('',(#13911,#13912));
#4030=EDGE_LOOP('',(#13913));
#4031=EDGE_LOOP('',(#13914));
#4032=EDGE_LOOP('',(#13915));
#4033=EDGE_LOOP('',(#13916));
#4034=EDGE_LOOP('',(#13917,#13918,#13919,#13920));
#4035=EDGE_LOOP('',(#13921,#13922,#13923,#13924));
#4036=EDGE_LOOP('',(#13925));
#4037=EDGE_LOOP('',(#13926));
#4038=EDGE_LOOP('',(#13927));
#4039=EDGE_LOOP('',(#13928));
#4040=EDGE_LOOP('',(#13929,#13930,#13931,#13932));
#4041=EDGE_LOOP('',(#13933,#13934,#13935,#13936));
#4042=EDGE_LOOP('',(#13937));
#4043=EDGE_LOOP('',(#13938));
#4044=EDGE_LOOP('',(#13939));
#4045=EDGE_LOOP('',(#13940));
#4046=EDGE_LOOP('',(#13941,#13942));
#4047=EDGE_LOOP('',(#13943,#13944,#13945,#13946,#13947,#13948,#13949,#13950,
#13951));
#4048=EDGE_LOOP('',(#13952,#13953,#13954));
#4049=EDGE_LOOP('',(#13955,#13956,#13957,#13958));
#4050=EDGE_LOOP('',(#13959,#13960,#13961));
#4051=EDGE_LOOP('',(#13962,#13963,#13964));
#4052=EDGE_LOOP('',(#13965,#13966,#13967,#13968));
#4053=EDGE_LOOP('',(#13969,#13970,#13971,#13972));
#4054=EDGE_LOOP('',(#13973,#13974,#13975,#13976));
#4055=EDGE_LOOP('',(#13977,#13978,#13979,#13980));
#4056=EDGE_LOOP('',(#13981,#13982));
#4057=EDGE_LOOP('',(#13983,#13984,#13985,#13986));
#4058=EDGE_LOOP('',(#13987));
#4059=EDGE_LOOP('',(#13988));
#4060=EDGE_LOOP('',(#13989));
#4061=EDGE_LOOP('',(#13990));
#4062=EDGE_LOOP('',(#13991,#13992,#13993,#13994));
#4063=EDGE_LOOP('',(#13995,#13996,#13997,#13998));
#4064=EDGE_LOOP('',(#13999));
#4065=EDGE_LOOP('',(#14000));
#4066=EDGE_LOOP('',(#14001));
#4067=EDGE_LOOP('',(#14002));
#4068=EDGE_LOOP('',(#14003,#14004,#14005,#14006));
#4069=EDGE_LOOP('',(#14007,#14008,#14009,#14010));
#4070=EDGE_LOOP('',(#14011,#14012,#14013,#14014));
#4071=EDGE_LOOP('',(#14015,#14016,#14017,#14018,#14019,#14020,#14021,#14022,
#14023,#14024,#14025,#14026,#14027,#14028,#14029,#14030,#14031,#14032,#14033,
#14034,#14035,#14036,#14037,#14038,#14039,#14040,#14041,#14042,#14043,#14044,
#14045,#14046,#14047,#14048,#14049,#14050,#14051,#14052,#14053,#14054,#14055,
#14056,#14057,#14058,#14059,#14060,#14061,#14062,#14063,#14064,#14065,#14066,
#14067,#14068,#14069,#14070,#14071,#14072,#14073,#14074,#14075,#14076,#14077,
#14078,#14079,#14080,#14081,#14082,#14083,#14084,#14085,#14086,#14087,#14088,
#14089,#14090,#14091,#14092,#14093,#14094,#14095,#14096,#14097,#14098,#14099,
#14100,#14101,#14102,#14103,#14104,#14105,#14106,#14107,#14108,#14109,#14110,
#14111,#14112,#14113,#14114,#14115,#14116,#14117,#14118,#14119,#14120,#14121,
#14122,#14123,#14124,#14125,#14126,#14127,#14128,#14129,#14130,#14131,#14132,
#14133,#14134,#14135,#14136,#14137,#14138,#14139,#14140,#14141,#14142,#14143,
#14144,#14145,#14146,#14147,#14148,#14149,#14150,#14151,#14152,#14153,#14154,
#14155,#14156,#14157,#14158,#14159,#14160,#14161,#14162,#14163,#14164,#14165,
#14166,#14167,#14168,#14169,#14170,#14171,#14172,#14173,#14174));
#4072=EDGE_LOOP('',(#14175,#14176,#14177,#14178));
#4073=EDGE_LOOP('',(#14179,#14180,#14181,#14182));
#4074=EDGE_LOOP('',(#14183,#14184,#14185,#14186));
#4075=EDGE_LOOP('',(#14187));
#4076=EDGE_LOOP('',(#14188,#14189,#14190,#14191));
#4077=EDGE_LOOP('',(#14192,#14193,#14194,#14195));
#4078=EDGE_LOOP('',(#14196,#14197,#14198,#14199));
#4079=EDGE_LOOP('',(#14200,#14201,#14202,#14203));
#4080=EDGE_LOOP('',(#14204,#14205,#14206,#14207));
#4081=EDGE_LOOP('',(#14208,#14209,#14210,#14211));
#4082=EDGE_LOOP('',(#14212,#14213,#14214,#14215));
#4083=EDGE_LOOP('',(#14216,#14217,#14218,#14219));
#4084=EDGE_LOOP('',(#14220,#14221,#14222,#14223));
#4085=EDGE_LOOP('',(#14224,#14225,#14226,#14227));
#4086=EDGE_LOOP('',(#14228,#14229,#14230,#14231));
#4087=EDGE_LOOP('',(#14232,#14233,#14234,#14235));
#4088=EDGE_LOOP('',(#14236,#14237,#14238,#14239));
#4089=EDGE_LOOP('',(#14240,#14241,#14242,#14243));
#4090=EDGE_LOOP('',(#14244,#14245,#14246,#14247));
#4091=EDGE_LOOP('',(#14248,#14249,#14250,#14251));
#4092=EDGE_LOOP('',(#14252,#14253,#14254,#14255));
#4093=EDGE_LOOP('',(#14256,#14257,#14258,#14259));
#4094=EDGE_LOOP('',(#14260,#14261,#14262,#14263));
#4095=EDGE_LOOP('',(#14264,#14265,#14266,#14267));
#4096=EDGE_LOOP('',(#14268,#14269,#14270,#14271));
#4097=EDGE_LOOP('',(#14272,#14273,#14274,#14275));
#4098=EDGE_LOOP('',(#14276,#14277,#14278,#14279));
#4099=EDGE_LOOP('',(#14280,#14281,#14282,#14283));
#4100=EDGE_LOOP('',(#14284,#14285,#14286,#14287));
#4101=EDGE_LOOP('',(#14288,#14289,#14290,#14291));
#4102=EDGE_LOOP('',(#14292,#14293,#14294,#14295));
#4103=EDGE_LOOP('',(#14296,#14297,#14298,#14299));
#4104=EDGE_LOOP('',(#14300,#14301,#14302,#14303));
#4105=EDGE_LOOP('',(#14304,#14305,#14306,#14307));
#4106=EDGE_LOOP('',(#14308,#14309,#14310,#14311));
#4107=EDGE_LOOP('',(#14312,#14313,#14314,#14315));
#4108=EDGE_LOOP('',(#14316,#14317,#14318,#14319));
#4109=EDGE_LOOP('',(#14320,#14321,#14322,#14323));
#4110=EDGE_LOOP('',(#14324,#14325,#14326,#14327));
#4111=EDGE_LOOP('',(#14328,#14329,#14330,#14331));
#4112=EDGE_LOOP('',(#14332,#14333,#14334,#14335));
#4113=EDGE_LOOP('',(#14336,#14337,#14338,#14339));
#4114=EDGE_LOOP('',(#14340,#14341,#14342,#14343));
#4115=EDGE_LOOP('',(#14344,#14345,#14346,#14347));
#4116=EDGE_LOOP('',(#14348,#14349,#14350,#14351));
#4117=EDGE_LOOP('',(#14352,#14353,#14354,#14355));
#4118=EDGE_LOOP('',(#14356,#14357,#14358,#14359));
#4119=EDGE_LOOP('',(#14360,#14361,#14362,#14363));
#4120=EDGE_LOOP('',(#14364,#14365,#14366,#14367));
#4121=EDGE_LOOP('',(#14368,#14369,#14370,#14371));
#4122=EDGE_LOOP('',(#14372,#14373,#14374,#14375));
#4123=EDGE_LOOP('',(#14376,#14377,#14378,#14379));
#4124=EDGE_LOOP('',(#14380,#14381,#14382,#14383));
#4125=EDGE_LOOP('',(#14384,#14385,#14386,#14387));
#4126=EDGE_LOOP('',(#14388,#14389,#14390,#14391));
#4127=EDGE_LOOP('',(#14392,#14393,#14394,#14395));
#4128=EDGE_LOOP('',(#14396,#14397,#14398,#14399));
#4129=EDGE_LOOP('',(#14400,#14401,#14402,#14403));
#4130=EDGE_LOOP('',(#14404,#14405,#14406,#14407));
#4131=EDGE_LOOP('',(#14408,#14409,#14410,#14411));
#4132=EDGE_LOOP('',(#14412,#14413,#14414,#14415));
#4133=EDGE_LOOP('',(#14416,#14417,#14418,#14419));
#4134=EDGE_LOOP('',(#14420,#14421,#14422,#14423));
#4135=EDGE_LOOP('',(#14424,#14425,#14426,#14427));
#4136=EDGE_LOOP('',(#14428,#14429,#14430,#14431));
#4137=EDGE_LOOP('',(#14432,#14433,#14434,#14435));
#4138=EDGE_LOOP('',(#14436,#14437,#14438,#14439));
#4139=EDGE_LOOP('',(#14440,#14441,#14442,#14443));
#4140=EDGE_LOOP('',(#14444,#14445,#14446,#14447));
#4141=EDGE_LOOP('',(#14448,#14449,#14450,#14451));
#4142=EDGE_LOOP('',(#14452,#14453,#14454,#14455));
#4143=EDGE_LOOP('',(#14456,#14457,#14458,#14459));
#4144=EDGE_LOOP('',(#14460,#14461,#14462,#14463));
#4145=EDGE_LOOP('',(#14464,#14465,#14466,#14467));
#4146=EDGE_LOOP('',(#14468,#14469,#14470,#14471));
#4147=EDGE_LOOP('',(#14472,#14473,#14474,#14475));
#4148=EDGE_LOOP('',(#14476,#14477,#14478,#14479));
#4149=EDGE_LOOP('',(#14480,#14481,#14482,#14483));
#4150=EDGE_LOOP('',(#14484,#14485,#14486,#14487));
#4151=EDGE_LOOP('',(#14488,#14489,#14490,#14491));
#4152=EDGE_LOOP('',(#14492,#14493,#14494,#14495));
#4153=EDGE_LOOP('',(#14496,#14497,#14498,#14499));
#4154=EDGE_LOOP('',(#14500,#14501,#14502,#14503));
#4155=EDGE_LOOP('',(#14504,#14505,#14506,#14507));
#4156=EDGE_LOOP('',(#14508,#14509,#14510,#14511));
#4157=EDGE_LOOP('',(#14512,#14513,#14514,#14515));
#4158=EDGE_LOOP('',(#14516,#14517,#14518,#14519));
#4159=EDGE_LOOP('',(#14520,#14521,#14522,#14523));
#4160=EDGE_LOOP('',(#14524,#14525,#14526,#14527));
#4161=EDGE_LOOP('',(#14528,#14529,#14530,#14531));
#4162=EDGE_LOOP('',(#14532,#14533,#14534,#14535));
#4163=EDGE_LOOP('',(#14536,#14537,#14538,#14539));
#4164=EDGE_LOOP('',(#14540,#14541,#14542,#14543));
#4165=EDGE_LOOP('',(#14544,#14545,#14546,#14547));
#4166=EDGE_LOOP('',(#14548,#14549,#14550,#14551));
#4167=EDGE_LOOP('',(#14552,#14553,#14554,#14555));
#4168=EDGE_LOOP('',(#14556,#14557,#14558,#14559));
#4169=EDGE_LOOP('',(#14560,#14561,#14562,#14563));
#4170=EDGE_LOOP('',(#14564,#14565,#14566,#14567));
#4171=EDGE_LOOP('',(#14568,#14569,#14570,#14571));
#4172=EDGE_LOOP('',(#14572,#14573,#14574,#14575));
#4173=EDGE_LOOP('',(#14576,#14577,#14578,#14579));
#4174=EDGE_LOOP('',(#14580,#14581,#14582,#14583));
#4175=EDGE_LOOP('',(#14584,#14585,#14586,#14587));
#4176=EDGE_LOOP('',(#14588,#14589,#14590,#14591));
#4177=EDGE_LOOP('',(#14592,#14593,#14594,#14595));
#4178=EDGE_LOOP('',(#14596,#14597,#14598,#14599));
#4179=EDGE_LOOP('',(#14600,#14601,#14602,#14603));
#4180=EDGE_LOOP('',(#14604,#14605,#14606,#14607));
#4181=EDGE_LOOP('',(#14608,#14609,#14610,#14611));
#4182=EDGE_LOOP('',(#14612,#14613,#14614,#14615));
#4183=EDGE_LOOP('',(#14616,#14617,#14618,#14619));
#4184=EDGE_LOOP('',(#14620,#14621,#14622,#14623));
#4185=EDGE_LOOP('',(#14624,#14625,#14626,#14627));
#4186=EDGE_LOOP('',(#14628,#14629,#14630,#14631));
#4187=EDGE_LOOP('',(#14632,#14633,#14634,#14635));
#4188=EDGE_LOOP('',(#14636,#14637,#14638,#14639));
#4189=EDGE_LOOP('',(#14640,#14641,#14642,#14643));
#4190=EDGE_LOOP('',(#14644,#14645,#14646,#14647));
#4191=EDGE_LOOP('',(#14648,#14649,#14650,#14651));
#4192=EDGE_LOOP('',(#14652,#14653,#14654,#14655));
#4193=EDGE_LOOP('',(#14656,#14657,#14658,#14659));
#4194=EDGE_LOOP('',(#14660,#14661,#14662,#14663));
#4195=EDGE_LOOP('',(#14664,#14665,#14666,#14667));
#4196=EDGE_LOOP('',(#14668,#14669,#14670,#14671));
#4197=EDGE_LOOP('',(#14672,#14673,#14674,#14675));
#4198=EDGE_LOOP('',(#14676,#14677,#14678,#14679));
#4199=EDGE_LOOP('',(#14680,#14681,#14682,#14683));
#4200=EDGE_LOOP('',(#14684,#14685,#14686,#14687));
#4201=EDGE_LOOP('',(#14688,#14689,#14690,#14691));
#4202=EDGE_LOOP('',(#14692,#14693,#14694,#14695));
#4203=EDGE_LOOP('',(#14696,#14697,#14698,#14699));
#4204=EDGE_LOOP('',(#14700,#14701,#14702,#14703));
#4205=EDGE_LOOP('',(#14704,#14705,#14706,#14707));
#4206=EDGE_LOOP('',(#14708,#14709,#14710,#14711));
#4207=EDGE_LOOP('',(#14712,#14713,#14714,#14715));
#4208=EDGE_LOOP('',(#14716,#14717,#14718,#14719));
#4209=EDGE_LOOP('',(#14720,#14721,#14722,#14723));
#4210=EDGE_LOOP('',(#14724,#14725,#14726,#14727));
#4211=EDGE_LOOP('',(#14728,#14729,#14730,#14731));
#4212=EDGE_LOOP('',(#14732,#14733,#14734,#14735));
#4213=EDGE_LOOP('',(#14736,#14737,#14738,#14739));
#4214=EDGE_LOOP('',(#14740,#14741,#14742,#14743));
#4215=EDGE_LOOP('',(#14744,#14745,#14746,#14747));
#4216=EDGE_LOOP('',(#14748,#14749,#14750,#14751));
#4217=EDGE_LOOP('',(#14752,#14753,#14754,#14755));
#4218=EDGE_LOOP('',(#14756,#14757,#14758,#14759));
#4219=EDGE_LOOP('',(#14760,#14761,#14762,#14763));
#4220=EDGE_LOOP('',(#14764,#14765,#14766,#14767));
#4221=EDGE_LOOP('',(#14768,#14769,#14770,#14771));
#4222=EDGE_LOOP('',(#14772,#14773,#14774,#14775));
#4223=EDGE_LOOP('',(#14776,#14777,#14778,#14779));
#4224=EDGE_LOOP('',(#14780,#14781,#14782,#14783));
#4225=EDGE_LOOP('',(#14784,#14785,#14786,#14787));
#4226=EDGE_LOOP('',(#14788,#14789,#14790,#14791));
#4227=EDGE_LOOP('',(#14792,#14793,#14794,#14795));
#4228=EDGE_LOOP('',(#14796,#14797,#14798,#14799));
#4229=EDGE_LOOP('',(#14800,#14801,#14802,#14803));
#4230=EDGE_LOOP('',(#14804,#14805,#14806,#14807));
#4231=EDGE_LOOP('',(#14808,#14809,#14810,#14811));
#4232=EDGE_LOOP('',(#14812,#14813,#14814,#14815));
#4233=EDGE_LOOP('',(#14816,#14817,#14818,#14819));
#4234=EDGE_LOOP('',(#14820,#14821,#14822,#14823));
#4235=EDGE_LOOP('',(#14824,#14825,#14826,#14827));
#4236=EDGE_LOOP('',(#14828,#14829,#14830,#14831,#14832,#14833,#14834,#14835,
#14836,#14837,#14838,#14839,#14840,#14841,#14842,#14843,#14844,#14845,#14846,
#14847,#14848,#14849,#14850,#14851,#14852,#14853,#14854,#14855,#14856,#14857,
#14858,#14859,#14860,#14861,#14862,#14863,#14864,#14865,#14866,#14867,#14868,
#14869,#14870,#14871,#14872,#14873,#14874,#14875,#14876,#14877,#14878,#14879,
#14880,#14881,#14882,#14883,#14884,#14885,#14886,#14887,#14888,#14889,#14890,
#14891,#14892,#14893,#14894,#14895,#14896,#14897,#14898,#14899,#14900,#14901,
#14902,#14903,#14904,#14905,#14906,#14907,#14908,#14909,#14910,#14911,#14912,
#14913,#14914,#14915,#14916,#14917,#14918,#14919,#14920,#14921,#14922,#14923,
#14924,#14925,#14926,#14927,#14928,#14929,#14930,#14931,#14932,#14933,#14934,
#14935,#14936,#14937,#14938,#14939,#14940,#14941,#14942,#14943,#14944,#14945,
#14946,#14947,#14948,#14949,#14950,#14951,#14952,#14953,#14954,#14955,#14956,
#14957,#14958,#14959,#14960,#14961,#14962,#14963,#14964,#14965,#14966,#14967,
#14968,#14969,#14970,#14971,#14972,#14973,#14974,#14975,#14976,#14977,#14978,
#14979,#14980,#14981,#14982,#14983,#14984,#14985,#14986,#14987));
#4237=EDGE_LOOP('',(#14988));
#4238=EDGE_LOOP('',(#14989,#14990,#14991,#14992));
#4239=EDGE_LOOP('',(#14993,#14994,#14995,#14996,#14997,#14998,#14999,#15000));
#4240=EDGE_LOOP('',(#15001,#15002,#15003,#15004));
#4241=EDGE_LOOP('',(#15005,#15006,#15007,#15008));
#4242=EDGE_LOOP('',(#15009,#15010,#15011,#15012));
#4243=EDGE_LOOP('',(#15013,#15014,#15015,#15016));
#4244=EDGE_LOOP('',(#15017,#15018,#15019,#15020,#15021,#15022,#15023,#15024));
#4245=EDGE_LOOP('',(#15025,#15026,#15027,#15028));
#4246=EDGE_LOOP('',(#15029,#15030,#15031,#15032));
#4247=EDGE_LOOP('',(#15033,#15034,#15035,#15036));
#4248=EDGE_LOOP('',(#15037,#15038,#15039,#15040));
#4249=EDGE_LOOP('',(#15041,#15042,#15043,#15044));
#4250=EDGE_LOOP('',(#15045,#15046,#15047,#15048));
#4251=EDGE_LOOP('',(#15049,#15050,#15051,#15052));
#4252=EDGE_LOOP('',(#15053,#15054,#15055,#15056));
#4253=EDGE_LOOP('',(#15057,#15058,#15059,#15060));
#4254=EDGE_LOOP('',(#15061,#15062,#15063,#15064));
#4255=EDGE_LOOP('',(#15065,#15066,#15067,#15068,#15069,#15070));
#4256=EDGE_LOOP('',(#15071));
#4257=EDGE_LOOP('',(#15072,#15073,#15074,#15075,#15076,#15077));
#4258=EDGE_LOOP('',(#15078,#15079,#15080,#15081));
#4259=EDGE_LOOP('',(#15082,#15083,#15084,#15085));
#4260=EDGE_LOOP('',(#15086,#15087,#15088,#15089));
#4261=EDGE_LOOP('',(#15090));
#4262=EDGE_LOOP('',(#15091));
#4263=EDGE_LOOP('',(#15092,#15093,#15094,#15095));
#4264=EDGE_LOOP('',(#15096,#15097,#15098,#15099));
#4265=EDGE_LOOP('',(#15100,#15101,#15102,#15103));
#4266=EDGE_LOOP('',(#15104));
#4267=EDGE_LOOP('',(#15105));
#4268=EDGE_LOOP('',(#15106,#15107,#15108,#15109));
#4269=EDGE_LOOP('',(#15110,#15111,#15112,#15113));
#4270=EDGE_LOOP('',(#15114,#15115,#15116,#15117));
#4271=EDGE_LOOP('',(#15118));
#4272=EDGE_LOOP('',(#15119,#15120,#15121,#15122));
#4273=EDGE_LOOP('',(#15123,#15124,#15125,#15126));
#4274=EDGE_LOOP('',(#15127,#15128,#15129,#15130));
#4275=EDGE_LOOP('',(#15131,#15132,#15133,#15134));
#4276=EDGE_LOOP('',(#15135,#15136,#15137,#15138));
#4277=EDGE_LOOP('',(#15139,#15140,#15141,#15142));
#4278=EDGE_LOOP('',(#15143,#15144,#15145,#15146,#15147,#15148));
#4279=EDGE_LOOP('',(#15149,#15150,#15151,#15152,#15153,#15154));
#4280=EDGE_LOOP('',(#15155,#15156,#15157,#15158));
#4281=EDGE_LOOP('',(#15159,#15160,#15161,#15162));
#4282=EDGE_LOOP('',(#15163));
#4283=EDGE_LOOP('',(#15164));
#4284=EDGE_LOOP('',(#15165));
#4285=EDGE_LOOP('',(#15166));
#4286=LINE('',#23316,#5418);
#4287=LINE('',#23322,#5419);
#4288=LINE('',#23328,#5420);
#4289=LINE('',#23333,#5421);
#4290=LINE('',#23335,#5422);
#4291=LINE('',#23337,#5423);
#4292=LINE('',#23338,#5424);
#4293=LINE('',#23341,#5425);
#4294=LINE('',#23343,#5426);
#4295=LINE('',#23344,#5427);
#4296=LINE('',#23347,#5428);
#4297=LINE('',#23349,#5429);
#4298=LINE('',#23350,#5430);
#4299=LINE('',#23352,#5431);
#4300=LINE('',#23353,#5432);
#4301=LINE('',#23361,#5433);
#4302=LINE('',#23367,#5434);
#4303=LINE('',#23373,#5435);
#4304=LINE('',#23379,#5436);
#4305=LINE('',#23385,#5437);
#4306=LINE('',#23391,#5438);
#4307=LINE('',#23397,#5439);
#4308=LINE('',#23403,#5440);
#4309=LINE('',#23409,#5441);
#4310=LINE('',#23415,#5442);
#4311=LINE('',#23421,#5443);
#4312=LINE('',#23427,#5444);
#4313=LINE('',#23433,#5445);
#4314=LINE('',#23439,#5446);
#4315=LINE('',#23445,#5447);
#4316=LINE('',#23451,#5448);
#4317=LINE('',#23457,#5449);
#4318=LINE('',#23463,#5450);
#4319=LINE('',#23469,#5451);
#4320=LINE('',#23475,#5452);
#4321=LINE('',#23481,#5453);
#4322=LINE('',#23487,#5454);
#4323=LINE('',#23493,#5455);
#4324=LINE('',#23499,#5456);
#4325=LINE('',#23505,#5457);
#4326=LINE('',#23510,#5458);
#4327=LINE('',#23512,#5459);
#4328=LINE('',#23514,#5460);
#4329=LINE('',#23515,#5461);
#4330=LINE('',#23518,#5462);
#4331=LINE('',#23520,#5463);
#4332=LINE('',#23521,#5464);
#4333=LINE('',#23525,#5465);
#4334=LINE('',#23527,#5466);
#4335=LINE('',#23529,#5467);
#4336=LINE('',#23530,#5468);
#4337=LINE('',#23532,#5469);
#4338=LINE('',#23534,#5470);
#4339=LINE('',#23535,#5471);
#4340=LINE('',#23538,#5472);
#4341=LINE('',#23539,#5473);
#4342=LINE('',#23541,#5474);
#4343=LINE('',#23542,#5475);
#4344=LINE('',#23550,#5476);
#4345=LINE('',#23556,#5477);
#4346=LINE('',#23562,#5478);
#4347=LINE('',#23568,#5479);
#4348=LINE('',#23574,#5480);
#4349=LINE('',#23581,#5481);
#4350=LINE('',#23587,#5482);
#4351=LINE('',#23596,#5483);
#4352=LINE('',#23602,#5484);
#4353=LINE('',#23608,#5485);
#4354=LINE('',#23614,#5486);
#4355=LINE('',#23620,#5487);
#4356=LINE('',#23628,#5488);
#4357=LINE('',#23633,#5489);
#4358=LINE('',#23642,#5490);
#4359=LINE('',#23648,#5491);
#4360=LINE('',#23654,#5492);
#4361=LINE('',#23660,#5493);
#4362=LINE('',#23666,#5494);
#4363=LINE('',#23673,#5495);
#4364=LINE('',#23679,#5496);
#4365=LINE('',#23688,#5497);
#4366=LINE('',#23694,#5498);
#4367=LINE('',#23700,#5499);
#4368=LINE('',#23706,#5500);
#4369=LINE('',#23712,#5501);
#4370=LINE('',#23720,#5502);
#4371=LINE('',#23725,#5503);
#4372=LINE('',#23733,#5504);
#4373=LINE('',#23735,#5505);
#4374=LINE('',#23737,#5506);
#4375=LINE('',#23738,#5507);
#4376=LINE('',#23741,#5508);
#4377=LINE('',#23743,#5509);
#4378=LINE('',#23744,#5510);
#4379=LINE('',#23747,#5511);
#4380=LINE('',#23749,#5512);
#4381=LINE('',#23750,#5513);
#4382=LINE('',#23753,#5514);
#4383=LINE('',#23755,#5515);
#4384=LINE('',#23756,#5516);
#4385=LINE('',#23759,#5517);
#4386=LINE('',#23761,#5518);
#4387=LINE('',#23762,#5519);
#4388=LINE('',#23764,#5520);
#4389=LINE('',#23765,#5521);
#4390=LINE('',#23777,#5522);
#4391=LINE('',#23781,#5523);
#4392=LINE('',#23785,#5524);
#4393=LINE('',#23792,#5525);
#4394=LINE('',#23794,#5526);
#4395=LINE('',#23800,#5527);
#4396=LINE('',#23806,#5528);
#4397=LINE('',#23812,#5529);
#4398=LINE('',#23818,#5530);
#4399=LINE('',#23824,#5531);
#4400=LINE('',#23831,#5532);
#4401=LINE('',#23837,#5533);
#4402=LINE('',#23846,#5534);
#4403=LINE('',#23852,#5535);
#4404=LINE('',#23858,#5536);
#4405=LINE('',#23864,#5537);
#4406=LINE('',#23870,#5538);
#4407=LINE('',#23878,#5539);
#4408=LINE('',#23883,#5540);
#4409=LINE('',#23892,#5541);
#4410=LINE('',#23898,#5542);
#4411=LINE('',#23904,#5543);
#4412=LINE('',#23910,#5544);
#4413=LINE('',#23916,#5545);
#4414=LINE('',#23923,#5546);
#4415=LINE('',#23929,#5547);
#4416=LINE('',#23938,#5548);
#4417=LINE('',#23944,#5549);
#4418=LINE('',#23950,#5550);
#4419=LINE('',#23956,#5551);
#4420=LINE('',#23962,#5552);
#4421=LINE('',#23970,#5553);
#4422=LINE('',#23975,#5554);
#4423=LINE('',#23993,#5555);
#4424=LINE('',#23999,#5556);
#4425=LINE('',#24003,#5557);
#4426=LINE('',#24009,#5558);
#4427=LINE('',#24014,#5559);
#4428=LINE('',#24029,#5560);
#4429=LINE('',#24038,#5561);
#4430=LINE('',#24042,#5562);
#4431=LINE('',#24046,#5563);
#4432=LINE('',#24049,#5564);
#4433=LINE('',#24185,#5565);
#4434=LINE('',#24438,#5566);
#4435=LINE('',#24480,#5567);
#4436=LINE('',#24485,#5568);
#4437=LINE('',#24494,#5569);
#4438=LINE('',#24499,#5570);
#4439=LINE('',#24519,#5571);
#4440=LINE('',#24525,#5572);
#4441=LINE('',#24529,#5573);
#4442=LINE('',#24535,#5574);
#4443=LINE('',#24540,#5575);
#4444=LINE('',#24555,#5576);
#4445=LINE('',#24564,#5577);
#4446=LINE('',#24568,#5578);
#4447=LINE('',#24572,#5579);
#4448=LINE('',#24575,#5580);
#4449=LINE('',#24728,#5581);
#4450=LINE('',#25024,#5582);
#4451=LINE('',#25066,#5583);
#4452=LINE('',#25071,#5584);
#4453=LINE('',#25080,#5585);
#4454=LINE('',#25085,#5586);
#4455=LINE('',#25095,#5587);
#4456=LINE('',#25097,#5588);
#4457=LINE('',#25099,#5589);
#4458=LINE('',#25100,#5590);
#4459=LINE('',#25103,#5591);
#4460=LINE('',#25105,#5592);
#4461=LINE('',#25106,#5593);
#4462=LINE('',#25109,#5594);
#4463=LINE('',#25111,#5595);
#4464=LINE('',#25112,#5596);
#4465=LINE('',#25115,#5597);
#4466=LINE('',#25117,#5598);
#4467=LINE('',#25118,#5599);
#4468=LINE('',#25121,#5600);
#4469=LINE('',#25123,#5601);
#4470=LINE('',#25124,#5602);
#4471=LINE('',#25126,#5603);
#4472=LINE('',#25127,#5604);
#4473=LINE('',#25139,#5605);
#4474=LINE('',#25143,#5606);
#4475=LINE('',#25147,#5607);
#4476=LINE('',#25154,#5608);
#4477=LINE('',#25156,#5609);
#4478=LINE('',#25161,#5610);
#4479=LINE('',#25163,#5611);
#4480=LINE('',#25165,#5612);
#4481=LINE('',#25166,#5613);
#4482=LINE('',#25169,#5614);
#4483=LINE('',#25171,#5615);
#4484=LINE('',#25172,#5616);
#4485=LINE('',#25175,#5617);
#4486=LINE('',#25177,#5618);
#4487=LINE('',#25178,#5619);
#4488=LINE('',#25180,#5620);
#4489=LINE('',#25181,#5621);
#4490=LINE('',#25186,#5622);
#4491=LINE('',#25188,#5623);
#4492=LINE('',#25190,#5624);
#4493=LINE('',#25191,#5625);
#4494=LINE('',#25194,#5626);
#4495=LINE('',#25196,#5627);
#4496=LINE('',#25197,#5628);
#4497=LINE('',#25200,#5629);
#4498=LINE('',#25202,#5630);
#4499=LINE('',#25203,#5631);
#4500=LINE('',#25205,#5632);
#4501=LINE('',#25206,#5633);
#4502=LINE('',#25211,#5634);
#4503=LINE('',#25213,#5635);
#4504=LINE('',#25215,#5636);
#4505=LINE('',#25216,#5637);
#4506=LINE('',#25219,#5638);
#4507=LINE('',#25221,#5639);
#4508=LINE('',#25222,#5640);
#4509=LINE('',#25225,#5641);
#4510=LINE('',#25227,#5642);
#4511=LINE('',#25228,#5643);
#4512=LINE('',#25230,#5644);
#4513=LINE('',#25231,#5645);
#4514=LINE('',#25236,#5646);
#4515=LINE('',#25238,#5647);
#4516=LINE('',#25240,#5648);
#4517=LINE('',#25241,#5649);
#4518=LINE('',#25244,#5650);
#4519=LINE('',#25246,#5651);
#4520=LINE('',#25247,#5652);
#4521=LINE('',#25250,#5653);
#4522=LINE('',#25252,#5654);
#4523=LINE('',#25253,#5655);
#4524=LINE('',#25255,#5656);
#4525=LINE('',#25256,#5657);
#4526=LINE('',#25261,#5658);
#4527=LINE('',#25263,#5659);
#4528=LINE('',#25265,#5660);
#4529=LINE('',#25266,#5661);
#4530=LINE('',#25269,#5662);
#4531=LINE('',#25271,#5663);
#4532=LINE('',#25272,#5664);
#4533=LINE('',#25275,#5665);
#4534=LINE('',#25277,#5666);
#4535=LINE('',#25278,#5667);
#4536=LINE('',#25280,#5668);
#4537=LINE('',#25281,#5669);
#4538=LINE('',#25286,#5670);
#4539=LINE('',#25288,#5671);
#4540=LINE('',#25290,#5672);
#4541=LINE('',#25291,#5673);
#4542=LINE('',#25294,#5674);
#4543=LINE('',#25296,#5675);
#4544=LINE('',#25297,#5676);
#4545=LINE('',#25300,#5677);
#4546=LINE('',#25302,#5678);
#4547=LINE('',#25303,#5679);
#4548=LINE('',#25305,#5680);
#4549=LINE('',#25306,#5681);
#4550=LINE('',#25311,#5682);
#4551=LINE('',#25313,#5683);
#4552=LINE('',#25315,#5684);
#4553=LINE('',#25316,#5685);
#4554=LINE('',#25319,#5686);
#4555=LINE('',#25321,#5687);
#4556=LINE('',#25322,#5688);
#4557=LINE('',#25325,#5689);
#4558=LINE('',#25327,#5690);
#4559=LINE('',#25328,#5691);
#4560=LINE('',#25330,#5692);
#4561=LINE('',#25331,#5693);
#4562=LINE('',#25336,#5694);
#4563=LINE('',#25338,#5695);
#4564=LINE('',#25340,#5696);
#4565=LINE('',#25341,#5697);
#4566=LINE('',#25344,#5698);
#4567=LINE('',#25346,#5699);
#4568=LINE('',#25347,#5700);
#4569=LINE('',#25350,#5701);
#4570=LINE('',#25352,#5702);
#4571=LINE('',#25353,#5703);
#4572=LINE('',#25355,#5704);
#4573=LINE('',#25356,#5705);
#4574=LINE('',#25361,#5706);
#4575=LINE('',#25363,#5707);
#4576=LINE('',#25365,#5708);
#4577=LINE('',#25366,#5709);
#4578=LINE('',#25369,#5710);
#4579=LINE('',#25371,#5711);
#4580=LINE('',#25372,#5712);
#4581=LINE('',#25375,#5713);
#4582=LINE('',#25377,#5714);
#4583=LINE('',#25378,#5715);
#4584=LINE('',#25380,#5716);
#4585=LINE('',#25381,#5717);
#4586=LINE('',#25386,#5718);
#4587=LINE('',#25388,#5719);
#4588=LINE('',#25390,#5720);
#4589=LINE('',#25391,#5721);
#4590=LINE('',#25394,#5722);
#4591=LINE('',#25396,#5723);
#4592=LINE('',#25397,#5724);
#4593=LINE('',#25400,#5725);
#4594=LINE('',#25402,#5726);
#4595=LINE('',#25403,#5727);
#4596=LINE('',#25405,#5728);
#4597=LINE('',#25406,#5729);
#4598=LINE('',#25411,#5730);
#4599=LINE('',#25413,#5731);
#4600=LINE('',#25415,#5732);
#4601=LINE('',#25416,#5733);
#4602=LINE('',#25419,#5734);
#4603=LINE('',#25421,#5735);
#4604=LINE('',#25422,#5736);
#4605=LINE('',#25425,#5737);
#4606=LINE('',#25427,#5738);
#4607=LINE('',#25428,#5739);
#4608=LINE('',#25430,#5740);
#4609=LINE('',#25431,#5741);
#4610=LINE('',#25436,#5742);
#4611=LINE('',#25438,#5743);
#4612=LINE('',#25440,#5744);
#4613=LINE('',#25441,#5745);
#4614=LINE('',#25444,#5746);
#4615=LINE('',#25446,#5747);
#4616=LINE('',#25447,#5748);
#4617=LINE('',#25450,#5749);
#4618=LINE('',#25452,#5750);
#4619=LINE('',#25453,#5751);
#4620=LINE('',#25455,#5752);
#4621=LINE('',#25456,#5753);
#4622=LINE('',#25461,#5754);
#4623=LINE('',#25463,#5755);
#4624=LINE('',#25465,#5756);
#4625=LINE('',#25466,#5757);
#4626=LINE('',#25469,#5758);
#4627=LINE('',#25471,#5759);
#4628=LINE('',#25472,#5760);
#4629=LINE('',#25475,#5761);
#4630=LINE('',#25477,#5762);
#4631=LINE('',#25478,#5763);
#4632=LINE('',#25480,#5764);
#4633=LINE('',#25481,#5765);
#4634=LINE('',#25486,#5766);
#4635=LINE('',#25488,#5767);
#4636=LINE('',#25490,#5768);
#4637=LINE('',#25491,#5769);
#4638=LINE('',#25494,#5770);
#4639=LINE('',#25496,#5771);
#4640=LINE('',#25497,#5772);
#4641=LINE('',#25500,#5773);
#4642=LINE('',#25502,#5774);
#4643=LINE('',#25503,#5775);
#4644=LINE('',#25505,#5776);
#4645=LINE('',#25506,#5777);
#4646=LINE('',#25511,#5778);
#4647=LINE('',#25513,#5779);
#4648=LINE('',#25515,#5780);
#4649=LINE('',#25516,#5781);
#4650=LINE('',#25519,#5782);
#4651=LINE('',#25521,#5783);
#4652=LINE('',#25522,#5784);
#4653=LINE('',#25525,#5785);
#4654=LINE('',#25527,#5786);
#4655=LINE('',#25528,#5787);
#4656=LINE('',#25530,#5788);
#4657=LINE('',#25531,#5789);
#4658=LINE('',#25536,#5790);
#4659=LINE('',#25538,#5791);
#4660=LINE('',#25540,#5792);
#4661=LINE('',#25541,#5793);
#4662=LINE('',#25544,#5794);
#4663=LINE('',#25546,#5795);
#4664=LINE('',#25547,#5796);
#4665=LINE('',#25550,#5797);
#4666=LINE('',#25552,#5798);
#4667=LINE('',#25553,#5799);
#4668=LINE('',#25555,#5800);
#4669=LINE('',#25556,#5801);
#4670=LINE('',#25561,#5802);
#4671=LINE('',#25563,#5803);
#4672=LINE('',#25565,#5804);
#4673=LINE('',#25566,#5805);
#4674=LINE('',#25569,#5806);
#4675=LINE('',#25571,#5807);
#4676=LINE('',#25572,#5808);
#4677=LINE('',#25575,#5809);
#4678=LINE('',#25577,#5810);
#4679=LINE('',#25578,#5811);
#4680=LINE('',#25580,#5812);
#4681=LINE('',#25581,#5813);
#4682=LINE('',#25586,#5814);
#4683=LINE('',#25588,#5815);
#4684=LINE('',#25590,#5816);
#4685=LINE('',#25591,#5817);
#4686=LINE('',#25594,#5818);
#4687=LINE('',#25596,#5819);
#4688=LINE('',#25597,#5820);
#4689=LINE('',#25600,#5821);
#4690=LINE('',#25602,#5822);
#4691=LINE('',#25603,#5823);
#4692=LINE('',#25605,#5824);
#4693=LINE('',#25606,#5825);
#4694=LINE('',#25611,#5826);
#4695=LINE('',#25613,#5827);
#4696=LINE('',#25615,#5828);
#4697=LINE('',#25616,#5829);
#4698=LINE('',#25619,#5830);
#4699=LINE('',#25621,#5831);
#4700=LINE('',#25622,#5832);
#4701=LINE('',#25625,#5833);
#4702=LINE('',#25627,#5834);
#4703=LINE('',#25628,#5835);
#4704=LINE('',#25630,#5836);
#4705=LINE('',#25631,#5837);
#4706=LINE('',#25636,#5838);
#4707=LINE('',#25638,#5839);
#4708=LINE('',#25640,#5840);
#4709=LINE('',#25641,#5841);
#4710=LINE('',#25644,#5842);
#4711=LINE('',#25646,#5843);
#4712=LINE('',#25647,#5844);
#4713=LINE('',#25650,#5845);
#4714=LINE('',#25652,#5846);
#4715=LINE('',#25653,#5847);
#4716=LINE('',#25655,#5848);
#4717=LINE('',#25656,#5849);
#4718=LINE('',#25661,#5850);
#4719=LINE('',#25663,#5851);
#4720=LINE('',#25665,#5852);
#4721=LINE('',#25666,#5853);
#4722=LINE('',#25669,#5854);
#4723=LINE('',#25671,#5855);
#4724=LINE('',#25672,#5856);
#4725=LINE('',#25675,#5857);
#4726=LINE('',#25677,#5858);
#4727=LINE('',#25678,#5859);
#4728=LINE('',#25680,#5860);
#4729=LINE('',#25681,#5861);
#4730=LINE('',#25686,#5862);
#4731=LINE('',#25688,#5863);
#4732=LINE('',#25690,#5864);
#4733=LINE('',#25691,#5865);
#4734=LINE('',#25694,#5866);
#4735=LINE('',#25696,#5867);
#4736=LINE('',#25697,#5868);
#4737=LINE('',#25700,#5869);
#4738=LINE('',#25702,#5870);
#4739=LINE('',#25703,#5871);
#4740=LINE('',#25705,#5872);
#4741=LINE('',#25706,#5873);
#4742=LINE('',#25711,#5874);
#4743=LINE('',#25713,#5875);
#4744=LINE('',#25715,#5876);
#4745=LINE('',#25716,#5877);
#4746=LINE('',#25719,#5878);
#4747=LINE('',#25721,#5879);
#4748=LINE('',#25722,#5880);
#4749=LINE('',#25725,#5881);
#4750=LINE('',#25727,#5882);
#4751=LINE('',#25728,#5883);
#4752=LINE('',#25730,#5884);
#4753=LINE('',#25731,#5885);
#4754=LINE('',#25736,#5886);
#4755=LINE('',#25738,#5887);
#4756=LINE('',#25740,#5888);
#4757=LINE('',#25741,#5889);
#4758=LINE('',#25744,#5890);
#4759=LINE('',#25746,#5891);
#4760=LINE('',#25747,#5892);
#4761=LINE('',#25750,#5893);
#4762=LINE('',#25752,#5894);
#4763=LINE('',#25753,#5895);
#4764=LINE('',#25755,#5896);
#4765=LINE('',#25756,#5897);
#4766=LINE('',#25762,#5898);
#4767=LINE('',#25768,#5899);
#4768=LINE('',#25774,#5900);
#4769=LINE('',#25779,#5901);
#4770=LINE('',#25781,#5902);
#4771=LINE('',#25783,#5903);
#4772=LINE('',#25784,#5904);
#4773=LINE('',#25788,#5905);
#4774=LINE('',#25790,#5906);
#4775=LINE('',#25792,#5907);
#4776=LINE('',#25793,#5908);
#4777=LINE('',#25796,#5909);
#4778=LINE('',#25798,#5910);
#4779=LINE('',#25799,#5911);
#4780=LINE('',#25802,#5912);
#4781=LINE('',#25804,#5913);
#4782=LINE('',#25805,#5914);
#4783=LINE('',#25807,#5915);
#4784=LINE('',#25808,#5916);
#4785=LINE('',#25811,#5917);
#4786=LINE('',#25813,#5918);
#4787=LINE('',#25814,#5919);
#4788=LINE('',#25817,#5920);
#4789=LINE('',#25821,#5921);
#4790=LINE('',#25822,#5922);
#4791=LINE('',#25831,#5923);
#4792=LINE('',#25837,#5924);
#4793=LINE('',#25846,#5925);
#4794=LINE('',#25852,#5926);
#4795=LINE('',#25860,#5927);
#4796=LINE('',#25862,#5928);
#4797=LINE('',#25864,#5929);
#4798=LINE('',#25865,#5930);
#4799=LINE('',#25868,#5931);
#4800=LINE('',#25870,#5932);
#4801=LINE('',#25871,#5933);
#4802=LINE('',#25874,#5934);
#4803=LINE('',#25876,#5935);
#4804=LINE('',#25877,#5936);
#4805=LINE('',#25879,#5937);
#4806=LINE('',#25880,#5938);
#4807=LINE('',#25887,#5939);
#4808=LINE('',#25889,#5940);
#4809=LINE('',#25891,#5941);
#4810=LINE('',#25892,#5942);
#4811=LINE('',#25895,#5943);
#4812=LINE('',#25897,#5944);
#4813=LINE('',#25898,#5945);
#4814=LINE('',#25901,#5946);
#4815=LINE('',#25903,#5947);
#4816=LINE('',#25904,#5948);
#4817=LINE('',#25906,#5949);
#4818=LINE('',#25907,#5950);
#4819=LINE('',#25914,#5951);
#4820=LINE('',#25916,#5952);
#4821=LINE('',#25918,#5953);
#4822=LINE('',#25919,#5954);
#4823=LINE('',#25922,#5955);
#4824=LINE('',#25924,#5956);
#4825=LINE('',#25925,#5957);
#4826=LINE('',#25928,#5958);
#4827=LINE('',#25930,#5959);
#4828=LINE('',#25931,#5960);
#4829=LINE('',#25934,#5961);
#4830=LINE('',#25936,#5962);
#4831=LINE('',#25937,#5963);
#4832=LINE('',#25940,#5964);
#4833=LINE('',#25942,#5965);
#4834=LINE('',#25943,#5966);
#4835=LINE('',#25945,#5967);
#4836=LINE('',#25946,#5968);
#4837=LINE('',#25956,#5969);
#4838=LINE('',#25965,#5970);
#4839=LINE('',#25969,#5971);
#4840=LINE('',#25973,#5972);
#4841=LINE('',#25980,#5973);
#4842=LINE('',#25982,#5974);
#4843=LINE('',#25989,#5975);
#4844=LINE('',#25995,#5976);
#4845=LINE('',#25997,#5977);
#4846=LINE('',#25999,#5978);
#4847=LINE('',#26000,#5979);
#4848=LINE('',#26005,#5980);
#4849=LINE('',#26006,#5981);
#4850=LINE('',#26009,#5982);
#4851=LINE('',#26011,#5983);
#4852=LINE('',#26012,#5984);
#4853=LINE('',#26014,#5985);
#4854=LINE('',#26020,#5986);
#4855=LINE('',#26022,#5987);
#4856=LINE('',#26024,#5988);
#4857=LINE('',#26025,#5989);
#4858=LINE('',#26030,#5990);
#4859=LINE('',#26031,#5991);
#4860=LINE('',#26034,#5992);
#4861=LINE('',#26036,#5993);
#4862=LINE('',#26037,#5994);
#4863=LINE('',#26039,#5995);
#4864=LINE('',#26053,#5996);
#4865=LINE('',#26056,#5997);
#4866=LINE('',#26061,#5998);
#4867=LINE('',#26069,#5999);
#4868=LINE('',#26075,#6000);
#4869=LINE('',#26084,#6001);
#4870=LINE('',#26090,#6002);
#4871=LINE('',#26098,#6003);
#4872=LINE('',#26115,#6004);
#4873=LINE('',#26166,#6005);
#4874=LINE('',#26171,#6006);
#4875=LINE('',#26177,#6007);
#4876=LINE('',#26186,#6008);
#4877=LINE('',#26191,#6009);
#4878=LINE('',#26193,#6010);
#4879=LINE('',#26195,#6011);
#4880=LINE('',#26196,#6012);
#4881=LINE('',#26199,#6013);
#4882=LINE('',#26201,#6014);
#4883=LINE('',#26202,#6015);
#4884=LINE('',#26205,#6016);
#4885=LINE('',#26207,#6017);
#4886=LINE('',#26208,#6018);
#4887=LINE('',#26218,#6019);
#4888=LINE('',#26222,#6020);
#4889=LINE('',#26226,#6021);
#4890=LINE('',#26229,#6022);
#4891=LINE('',#26232,#6023);
#4892=LINE('',#26233,#6024);
#4893=LINE('',#26236,#6025);
#4894=LINE('',#26239,#6026);
#4895=LINE('',#26242,#6027);
#4896=LINE('',#26250,#6028);
#4897=LINE('',#26256,#6029);
#4898=LINE('',#26265,#6030);
#4899=LINE('',#26271,#6031);
#4900=LINE('',#26280,#6032);
#4901=LINE('',#26286,#6033);
#4902=LINE('',#26295,#6034);
#4903=LINE('',#26301,#6035);
#4904=LINE('',#26310,#6036);
#4905=LINE('',#26316,#6037);
#4906=LINE('',#26324,#6038);
#4907=LINE('',#26326,#6039);
#4908=LINE('',#26328,#6040);
#4909=LINE('',#26329,#6041);
#4910=LINE('',#26332,#6042);
#4911=LINE('',#26334,#6043);
#4912=LINE('',#26335,#6044);
#4913=LINE('',#26338,#6045);
#4914=LINE('',#26340,#6046);
#4915=LINE('',#26341,#6047);
#4916=LINE('',#26344,#6048);
#4917=LINE('',#26346,#6049);
#4918=LINE('',#26347,#6050);
#4919=LINE('',#26350,#6051);
#4920=LINE('',#26352,#6052);
#4921=LINE('',#26353,#6053);
#4922=LINE('',#26355,#6054);
#4923=LINE('',#26356,#6055);
#4924=LINE('',#26366,#6056);
#4925=LINE('',#26375,#6057);
#4926=LINE('',#26379,#6058);
#4927=LINE('',#26383,#6059);
#4928=LINE('',#26390,#6060);
#4929=LINE('',#26392,#6061);
#4930=LINE('',#26399,#6062);
#4931=LINE('',#26405,#6063);
#4932=LINE('',#26407,#6064);
#4933=LINE('',#26409,#6065);
#4934=LINE('',#26410,#6066);
#4935=LINE('',#26415,#6067);
#4936=LINE('',#26416,#6068);
#4937=LINE('',#26419,#6069);
#4938=LINE('',#26421,#6070);
#4939=LINE('',#26422,#6071);
#4940=LINE('',#26424,#6072);
#4941=LINE('',#26438,#6073);
#4942=LINE('',#26441,#6074);
#4943=LINE('',#26446,#6075);
#4944=LINE('',#26454,#6076);
#4945=LINE('',#26460,#6077);
#4946=LINE('',#26469,#6078);
#4947=LINE('',#26475,#6079);
#4948=LINE('',#26483,#6080);
#4949=LINE('',#26504,#6081);
#4950=LINE('',#26559,#6082);
#4951=LINE('',#26564,#6083);
#4952=LINE('',#26570,#6084);
#4953=LINE('',#26579,#6085);
#4954=LINE('',#26585,#6086);
#4955=LINE('',#26595,#6087);
#4956=LINE('',#26601,#6088);
#4957=LINE('',#26603,#6089);
#4958=LINE('',#26605,#6090);
#4959=LINE('',#26606,#6091);
#4960=LINE('',#26611,#6092);
#4961=LINE('',#26612,#6093);
#4962=LINE('',#26615,#6094);
#4963=LINE('',#26617,#6095);
#4964=LINE('',#26618,#6096);
#4965=LINE('',#26620,#6097);
#4966=LINE('',#26634,#6098);
#4967=LINE('',#26637,#6099);
#4968=LINE('',#26642,#6100);
#4969=LINE('',#26650,#6101);
#4970=LINE('',#26656,#6102);
#4971=LINE('',#26665,#6103);
#4972=LINE('',#26671,#6104);
#4973=LINE('',#26679,#6105);
#4974=LINE('',#26696,#6106);
#4975=LINE('',#26747,#6107);
#4976=LINE('',#26752,#6108);
#4977=LINE('',#26758,#6109);
#4978=LINE('',#26767,#6110);
#4979=LINE('',#26773,#6111);
#4980=LINE('',#26781,#6112);
#4981=LINE('',#26783,#6113);
#4982=LINE('',#26785,#6114);
#4983=LINE('',#26786,#6115);
#4984=LINE('',#26789,#6116);
#4985=LINE('',#26791,#6117);
#4986=LINE('',#26792,#6118);
#4987=LINE('',#26795,#6119);
#4988=LINE('',#26797,#6120);
#4989=LINE('',#26798,#6121);
#4990=LINE('',#26875,#6122);
#4991=LINE('',#27021,#6123);
#4992=LINE('',#27167,#6124);
#4993=LINE('',#27313,#6125);
#4994=LINE('',#27459,#6126);
#4995=LINE('',#27605,#6127);
#4996=LINE('',#27751,#6128);
#4997=LINE('',#27897,#6129);
#4998=LINE('',#28043,#6130);
#4999=LINE('',#28189,#6131);
#5000=LINE('',#28335,#6132);
#5001=LINE('',#28481,#6133);
#5002=LINE('',#28627,#6134);
#5003=LINE('',#28773,#6135);
#5004=LINE('',#28919,#6136);
#5005=LINE('',#29065,#6137);
#5006=LINE('',#29211,#6138);
#5007=LINE('',#29357,#6139);
#5008=LINE('',#29503,#6140);
#5009=LINE('',#29649,#6141);
#5010=LINE('',#29727,#6142);
#5011=LINE('',#29871,#6143);
#5012=LINE('',#29943,#6144);
#5013=LINE('',#29946,#6145);
#5014=LINE('',#29947,#6146);
#5015=LINE('',#30159,#6147);
#5016=LINE('',#30163,#6148);
#5017=LINE('',#30375,#6149);
#5018=LINE('',#30378,#6150);
#5019=LINE('',#30379,#6151);
#5020=LINE('',#30591,#6152);
#5021=LINE('',#30595,#6153);
#5022=LINE('',#30807,#6154);
#5023=LINE('',#30810,#6155);
#5024=LINE('',#30811,#6156);
#5025=LINE('',#31023,#6157);
#5026=LINE('',#31027,#6158);
#5027=LINE('',#31239,#6159);
#5028=LINE('',#31242,#6160);
#5029=LINE('',#31243,#6161);
#5030=LINE('',#31455,#6162);
#5031=LINE('',#31459,#6163);
#5032=LINE('',#31671,#6164);
#5033=LINE('',#31674,#6165);
#5034=LINE('',#31675,#6166);
#5035=LINE('',#31887,#6167);
#5036=LINE('',#31891,#6168);
#5037=LINE('',#32103,#6169);
#5038=LINE('',#32106,#6170);
#5039=LINE('',#32107,#6171);
#5040=LINE('',#32319,#6172);
#5041=LINE('',#32323,#6173);
#5042=LINE('',#32535,#6174);
#5043=LINE('',#32538,#6175);
#5044=LINE('',#32539,#6176);
#5045=LINE('',#32751,#6177);
#5046=LINE('',#32755,#6178);
#5047=LINE('',#32967,#6179);
#5048=LINE('',#32970,#6180);
#5049=LINE('',#32971,#6181);
#5050=LINE('',#33183,#6182);
#5051=LINE('',#33187,#6183);
#5052=LINE('',#33399,#6184);
#5053=LINE('',#33402,#6185);
#5054=LINE('',#33403,#6186);
#5055=LINE('',#33615,#6187);
#5056=LINE('',#33619,#6188);
#5057=LINE('',#33831,#6189);
#5058=LINE('',#33834,#6190);
#5059=LINE('',#33835,#6191);
#5060=LINE('',#34047,#6192);
#5061=LINE('',#34051,#6193);
#5062=LINE('',#34263,#6194);
#5063=LINE('',#34266,#6195);
#5064=LINE('',#34267,#6196);
#5065=LINE('',#34479,#6197);
#5066=LINE('',#34483,#6198);
#5067=LINE('',#34695,#6199);
#5068=LINE('',#34698,#6200);
#5069=LINE('',#34699,#6201);
#5070=LINE('',#34911,#6202);
#5071=LINE('',#34915,#6203);
#5072=LINE('',#35127,#6204);
#5073=LINE('',#35130,#6205);
#5074=LINE('',#35131,#6206);
#5075=LINE('',#35343,#6207);
#5076=LINE('',#35347,#6208);
#5077=LINE('',#35559,#6209);
#5078=LINE('',#35562,#6210);
#5079=LINE('',#35563,#6211);
#5080=LINE('',#35775,#6212);
#5081=LINE('',#35779,#6213);
#5082=LINE('',#35991,#6214);
#5083=LINE('',#35994,#6215);
#5084=LINE('',#35995,#6216);
#5085=LINE('',#36207,#6217);
#5086=LINE('',#36211,#6218);
#5087=LINE('',#36423,#6219);
#5088=LINE('',#36426,#6220);
#5089=LINE('',#36427,#6221);
#5090=LINE('',#36639,#6222);
#5091=LINE('',#36643,#6223);
#5092=LINE('',#36855,#6224);
#5093=LINE('',#36858,#6225);
#5094=LINE('',#36859,#6226);
#5095=LINE('',#37071,#6227);
#5096=LINE('',#37075,#6228);
#5097=LINE('',#37287,#6229);
#5098=LINE('',#37290,#6230);
#5099=LINE('',#37291,#6231);
#5100=LINE('',#37503,#6232);
#5101=LINE('',#37507,#6233);
#5102=LINE('',#37719,#6234);
#5103=LINE('',#37722,#6235);
#5104=LINE('',#37723,#6236);
#5105=LINE('',#37935,#6237);
#5106=LINE('',#37939,#6238);
#5107=LINE('',#38151,#6239);
#5108=LINE('',#38154,#6240);
#5109=LINE('',#38155,#6241);
#5110=LINE('',#38367,#6242);
#5111=LINE('',#38375,#6243);
#5112=LINE('',#38377,#6244);
#5113=LINE('',#38379,#6245);
#5114=LINE('',#38381,#6246);
#5115=LINE('',#38383,#6247);
#5116=LINE('',#38385,#6248);
#5117=LINE('',#38387,#6249);
#5118=LINE('',#38388,#6250);
#5119=LINE('',#38391,#6251);
#5120=LINE('',#38393,#6252);
#5121=LINE('',#38394,#6253);
#5122=LINE('',#38397,#6254);
#5123=LINE('',#38398,#6255);
#5124=LINE('',#38401,#6256);
#5125=LINE('',#38402,#6257);
#5126=LINE('',#38405,#6258);
#5127=LINE('',#38406,#6259);
#5128=LINE('',#38409,#6260);
#5129=LINE('',#38411,#6261);
#5130=LINE('',#38413,#6262);
#5131=LINE('',#38414,#6263);
#5132=LINE('',#38416,#6264);
#5133=LINE('',#38418,#6265);
#5134=LINE('',#38420,#6266);
#5135=LINE('',#38428,#6267);
#5136=LINE('',#38434,#6268);
#5137=LINE('',#38436,#6269);
#5138=LINE('',#38438,#6270);
#5139=LINE('',#38439,#6271);
#5140=LINE('',#38444,#6272);
#5141=LINE('',#38445,#6273);
#5142=LINE('',#38448,#6274);
#5143=LINE('',#38450,#6275);
#5144=LINE('',#38451,#6276);
#5145=LINE('',#38453,#6277);
#5146=LINE('',#38467,#6278);
#5147=LINE('',#38470,#6279);
#5148=LINE('',#38475,#6280);
#5149=LINE('',#38483,#6281);
#5150=LINE('',#38489,#6282);
#5151=LINE('',#38498,#6283);
#5152=LINE('',#38504,#6284);
#5153=LINE('',#38512,#6285);
#5154=LINE('',#38533,#6286);
#5155=LINE('',#38588,#6287);
#5156=LINE('',#38593,#6288);
#5157=LINE('',#38599,#6289);
#5158=LINE('',#38608,#6290);
#5159=LINE('',#38614,#6291);
#5160=LINE('',#38623,#6292);
#5161=LINE('',#38629,#6293);
#5162=LINE('',#38637,#6294);
#5163=LINE('',#38654,#6295);
#5164=LINE('',#38705,#6296);
#5165=LINE('',#38709,#6297);
#5166=LINE('',#38711,#6298);
#5167=LINE('',#38713,#6299);
#5168=LINE('',#38714,#6300);
#5169=LINE('',#38718,#6301);
#5170=LINE('',#38722,#6302);
#5171=LINE('',#38724,#6303);
#5172=LINE('',#38729,#6304);
#5173=LINE('',#38735,#6305);
#5174=LINE('',#38744,#6306);
#5175=LINE('',#38750,#6307);
#5176=LINE('',#38758,#6308);
#5177=LINE('',#38760,#6309);
#5178=LINE('',#38762,#6310);
#5179=LINE('',#38763,#6311);
#5180=LINE('',#38766,#6312);
#5181=LINE('',#38768,#6313);
#5182=LINE('',#38769,#6314);
#5183=LINE('',#38772,#6315);
#5184=LINE('',#38774,#6316);
#5185=LINE('',#38775,#6317);
#5186=LINE('',#38852,#6318);
#5187=LINE('',#38998,#6319);
#5188=LINE('',#39144,#6320);
#5189=LINE('',#39290,#6321);
#5190=LINE('',#39436,#6322);
#5191=LINE('',#39582,#6323);
#5192=LINE('',#39728,#6324);
#5193=LINE('',#39874,#6325);
#5194=LINE('',#40020,#6326);
#5195=LINE('',#40166,#6327);
#5196=LINE('',#40312,#6328);
#5197=LINE('',#40458,#6329);
#5198=LINE('',#40604,#6330);
#5199=LINE('',#40750,#6331);
#5200=LINE('',#40896,#6332);
#5201=LINE('',#41042,#6333);
#5202=LINE('',#41188,#6334);
#5203=LINE('',#41334,#6335);
#5204=LINE('',#41480,#6336);
#5205=LINE('',#41626,#6337);
#5206=LINE('',#41772,#6338);
#5207=LINE('',#41918,#6339);
#5208=LINE('',#42064,#6340);
#5209=LINE('',#42210,#6341);
#5210=LINE('',#42356,#6342);
#5211=LINE('',#42502,#6343);
#5212=LINE('',#42648,#6344);
#5213=LINE('',#42794,#6345);
#5214=LINE('',#42940,#6346);
#5215=LINE('',#43086,#6347);
#5216=LINE('',#43232,#6348);
#5217=LINE('',#43378,#6349);
#5218=LINE('',#43524,#6350);
#5219=LINE('',#43670,#6351);
#5220=LINE('',#43816,#6352);
#5221=LINE('',#43962,#6353);
#5222=LINE('',#44108,#6354);
#5223=LINE('',#44254,#6355);
#5224=LINE('',#44400,#6356);
#5225=LINE('',#44546,#6357);
#5226=LINE('',#44624,#6358);
#5227=LINE('',#44845,#6359);
#5228=LINE('',#44994,#6360);
#5229=LINE('',#45066,#6361);
#5230=LINE('',#45287,#6362);
#5231=LINE('',#45436,#6363);
#5232=LINE('',#45508,#6364);
#5233=LINE('',#45729,#6365);
#5234=LINE('',#45878,#6366);
#5235=LINE('',#45950,#6367);
#5236=LINE('',#46171,#6368);
#5237=LINE('',#46320,#6369);
#5238=LINE('',#46392,#6370);
#5239=LINE('',#46613,#6371);
#5240=LINE('',#46762,#6372);
#5241=LINE('',#46834,#6373);
#5242=LINE('',#47055,#6374);
#5243=LINE('',#47204,#6375);
#5244=LINE('',#47276,#6376);
#5245=LINE('',#47497,#6377);
#5246=LINE('',#47646,#6378);
#5247=LINE('',#47718,#6379);
#5248=LINE('',#47939,#6380);
#5249=LINE('',#48088,#6381);
#5250=LINE('',#48160,#6382);
#5251=LINE('',#48381,#6383);
#5252=LINE('',#48530,#6384);
#5253=LINE('',#48602,#6385);
#5254=LINE('',#48823,#6386);
#5255=LINE('',#48972,#6387);
#5256=LINE('',#49044,#6388);
#5257=LINE('',#49265,#6389);
#5258=LINE('',#49414,#6390);
#5259=LINE('',#49486,#6391);
#5260=LINE('',#49707,#6392);
#5261=LINE('',#49856,#6393);
#5262=LINE('',#49928,#6394);
#5263=LINE('',#50149,#6395);
#5264=LINE('',#50298,#6396);
#5265=LINE('',#50370,#6397);
#5266=LINE('',#50591,#6398);
#5267=LINE('',#50740,#6399);
#5268=LINE('',#50812,#6400);
#5269=LINE('',#51033,#6401);
#5270=LINE('',#51182,#6402);
#5271=LINE('',#51254,#6403);
#5272=LINE('',#51475,#6404);
#5273=LINE('',#51624,#6405);
#5274=LINE('',#51696,#6406);
#5275=LINE('',#51917,#6407);
#5276=LINE('',#52066,#6408);
#5277=LINE('',#52138,#6409);
#5278=LINE('',#52359,#6410);
#5279=LINE('',#52508,#6411);
#5280=LINE('',#52580,#6412);
#5281=LINE('',#52801,#6413);
#5282=LINE('',#52950,#6414);
#5283=LINE('',#53022,#6415);
#5284=LINE('',#53243,#6416);
#5285=LINE('',#53392,#6417);
#5286=LINE('',#53464,#6418);
#5287=LINE('',#53685,#6419);
#5288=LINE('',#53834,#6420);
#5289=LINE('',#53906,#6421);
#5290=LINE('',#54127,#6422);
#5291=LINE('',#54276,#6423);
#5292=LINE('',#54348,#6424);
#5293=LINE('',#54569,#6425);
#5294=LINE('',#54718,#6426);
#5295=LINE('',#54790,#6427);
#5296=LINE('',#55011,#6428);
#5297=LINE('',#55160,#6429);
#5298=LINE('',#55232,#6430);
#5299=LINE('',#55453,#6431);
#5300=LINE('',#55602,#6432);
#5301=LINE('',#55674,#6433);
#5302=LINE('',#55895,#6434);
#5303=LINE('',#56044,#6435);
#5304=LINE('',#56116,#6436);
#5305=LINE('',#56337,#6437);
#5306=LINE('',#56486,#6438);
#5307=LINE('',#56558,#6439);
#5308=LINE('',#56779,#6440);
#5309=LINE('',#56928,#6441);
#5310=LINE('',#57000,#6442);
#5311=LINE('',#57221,#6443);
#5312=LINE('',#57370,#6444);
#5313=LINE('',#57442,#6445);
#5314=LINE('',#57663,#6446);
#5315=LINE('',#57812,#6447);
#5316=LINE('',#57884,#6448);
#5317=LINE('',#58105,#6449);
#5318=LINE('',#58254,#6450);
#5319=LINE('',#58326,#6451);
#5320=LINE('',#58547,#6452);
#5321=LINE('',#58696,#6453);
#5322=LINE('',#58768,#6454);
#5323=LINE('',#58989,#6455);
#5324=LINE('',#59138,#6456);
#5325=LINE('',#59210,#6457);
#5326=LINE('',#59431,#6458);
#5327=LINE('',#59580,#6459);
#5328=LINE('',#59652,#6460);
#5329=LINE('',#59873,#6461);
#5330=LINE('',#60022,#6462);
#5331=LINE('',#60094,#6463);
#5332=LINE('',#60315,#6464);
#5333=LINE('',#60464,#6465);
#5334=LINE('',#60536,#6466);
#5335=LINE('',#60757,#6467);
#5336=LINE('',#60906,#6468);
#5337=LINE('',#60978,#6469);
#5338=LINE('',#61199,#6470);
#5339=LINE('',#61348,#6471);
#5340=LINE('',#61420,#6472);
#5341=LINE('',#61641,#6473);
#5342=LINE('',#61644,#6474);
#5343=LINE('',#61645,#6475);
#5344=LINE('',#62020,#6476);
#5345=LINE('',#62302,#6477);
#5346=LINE('',#62304,#6478);
#5347=LINE('',#62312,#6479);
#5348=LINE('',#62314,#6480);
#5349=LINE('',#62316,#6481);
#5350=LINE('',#62318,#6482);
#5351=LINE('',#62320,#6483);
#5352=LINE('',#62322,#6484);
#5353=LINE('',#62324,#6485);
#5354=LINE('',#62325,#6486);
#5355=LINE('',#62328,#6487);
#5356=LINE('',#62330,#6488);
#5357=LINE('',#62331,#6489);
#5358=LINE('',#62334,#6490);
#5359=LINE('',#62335,#6491);
#5360=LINE('',#62338,#6492);
#5361=LINE('',#62339,#6493);
#5362=LINE('',#62342,#6494);
#5363=LINE('',#62343,#6495);
#5364=LINE('',#62347,#6496);
#5365=LINE('',#62348,#6497);
#5366=LINE('',#62350,#6498);
#5367=LINE('',#62351,#6499);
#5368=LINE('',#62353,#6500);
#5369=LINE('',#62355,#6501);
#5370=LINE('',#62357,#6502);
#5371=LINE('',#62363,#6503);
#5372=LINE('',#62365,#6504);
#5373=LINE('',#62367,#6505);
#5374=LINE('',#62368,#6506);
#5375=LINE('',#62371,#6507);
#5376=LINE('',#62373,#6508);
#5377=LINE('',#62374,#6509);
#5378=LINE('',#62377,#6510);
#5379=LINE('',#62379,#6511);
#5380=LINE('',#62380,#6512);
#5381=LINE('',#62383,#6513);
#5382=LINE('',#62385,#6514);
#5383=LINE('',#62386,#6515);
#5384=LINE('',#62389,#6516);
#5385=LINE('',#62391,#6517);
#5386=LINE('',#62392,#6518);
#5387=LINE('',#62394,#6519);
#5388=LINE('',#62395,#6520);
#5389=LINE('',#62403,#6521);
#5390=LINE('',#62407,#6522);
#5391=LINE('',#62411,#6523);
#5392=LINE('',#62420,#6524);
#5393=LINE('',#62424,#6525);
#5394=LINE('',#62428,#6526);
#5395=LINE('',#62435,#6527);
#5396=LINE('',#62439,#6528);
#5397=LINE('',#62443,#6529);
#5398=LINE('',#62448,#6530);
#5399=LINE('',#62450,#6531);
#5400=LINE('',#62452,#6532);
#5401=LINE('',#62453,#6533);
#5402=LINE('',#62456,#6534);
#5403=LINE('',#62458,#6535);
#5404=LINE('',#62459,#6536);
#5405=LINE('',#62462,#6537);
#5406=LINE('',#62464,#6538);
#5407=LINE('',#62465,#6539);
#5408=LINE('',#62468,#6540);
#5409=LINE('',#62470,#6541);
#5410=LINE('',#62471,#6542);
#5411=LINE('',#62474,#6543);
#5412=LINE('',#62476,#6544);
#5413=LINE('',#62477,#6545);
#5414=LINE('',#62479,#6546);
#5415=LINE('',#62480,#6547);
#5416=LINE('',#62594,#6548);
#5417=LINE('',#62600,#6549);
#5418=VECTOR('',#18841,0.25);
#5419=VECTOR('',#18848,0.25);
#5420=VECTOR('',#18855,0.25);
#5421=VECTOR('',#18860,1.);
#5422=VECTOR('',#18861,1.);
#5423=VECTOR('',#18862,1.);
#5424=VECTOR('',#18863,1.);
#5425=VECTOR('',#18866,1.);
#5426=VECTOR('',#18867,1.);
#5427=VECTOR('',#18868,1.);
#5428=VECTOR('',#18871,1.);
#5429=VECTOR('',#18872,1.);
#5430=VECTOR('',#18873,1.);
#5431=VECTOR('',#18876,1.);
#5432=VECTOR('',#18877,1.);
#5433=VECTOR('',#18888,0.225000000000001);
#5434=VECTOR('',#18895,0.225000000000001);
#5435=VECTOR('',#18902,0.164999999999999);
#5436=VECTOR('',#18909,0.164999999999999);
#5437=VECTOR('',#18916,0.164999999999999);
#5438=VECTOR('',#18923,0.164999999999999);
#5439=VECTOR('',#18930,2.35);
#5440=VECTOR('',#18937,0.164999999999999);
#5441=VECTOR('',#18944,0.164999999999999);
#5442=VECTOR('',#18951,0.164999999999999);
#5443=VECTOR('',#18958,0.164999999999999);
#5444=VECTOR('',#18965,1.6);
#5445=VECTOR('',#18972,0.165);
#5446=VECTOR('',#18979,0.165);
#5447=VECTOR('',#18986,0.165);
#5448=VECTOR('',#18993,0.165);
#5449=VECTOR('',#19000,2.35);
#5450=VECTOR('',#19007,0.165);
#5451=VECTOR('',#19014,0.165);
#5452=VECTOR('',#19021,0.165);
#5453=VECTOR('',#19028,0.165);
#5454=VECTOR('',#19035,1.6);
#5455=VECTOR('',#19042,0.33);
#5456=VECTOR('',#19049,0.33);
#5457=VECTOR('',#19056,0.329999999999998);
#5458=VECTOR('',#19061,1.);
#5459=VECTOR('',#19062,1.);
#5460=VECTOR('',#19063,1.);
#5461=VECTOR('',#19064,1.);
#5462=VECTOR('',#19067,1.);
#5463=VECTOR('',#19068,1.);
#5464=VECTOR('',#19069,1.);
#5465=VECTOR('',#19072,1.);
#5466=VECTOR('',#19073,1.);
#5467=VECTOR('',#19074,1.);
#5468=VECTOR('',#19075,1.);
#5469=VECTOR('',#19078,1.);
#5470=VECTOR('',#19079,1.);
#5471=VECTOR('',#19080,1.);
#5472=VECTOR('',#19083,1.);
#5473=VECTOR('',#19084,1.);
#5474=VECTOR('',#19087,1.);
#5475=VECTOR('',#19088,1.);
#5476=VECTOR('',#19099,0.225);
#5477=VECTOR('',#19106,0.225);
#5478=VECTOR('',#19113,0.225);
#5479=VECTOR('',#19120,0.225);
#5480=VECTOR('',#19127,1.59);
#5481=VECTOR('',#19136,1.2);
#5482=VECTOR('',#19143,2.5);
#5483=VECTOR('',#19156,0.225);
#5484=VECTOR('',#19163,0.225);
#5485=VECTOR('',#19170,0.225);
#5486=VECTOR('',#19177,0.225);
#5487=VECTOR('',#19184,1.59);
#5488=VECTOR('',#19195,1.2);
#5489=VECTOR('',#19200,2.5);
#5490=VECTOR('',#19213,0.225);
#5491=VECTOR('',#19220,0.225);
#5492=VECTOR('',#19227,0.225000000000001);
#5493=VECTOR('',#19234,0.225000000000001);
#5494=VECTOR('',#19241,2.34);
#5495=VECTOR('',#19250,1.9);
#5496=VECTOR('',#19257,3.);
#5497=VECTOR('',#19270,0.225);
#5498=VECTOR('',#19277,0.225);
#5499=VECTOR('',#19284,0.225000000000001);
#5500=VECTOR('',#19291,0.225000000000001);
#5501=VECTOR('',#19298,2.34);
#5502=VECTOR('',#19309,1.9);
#5503=VECTOR('',#19314,3.);
#5504=VECTOR('',#19325,1.);
#5505=VECTOR('',#19326,1.);
#5506=VECTOR('',#19327,1.);
#5507=VECTOR('',#19328,1.);
#5508=VECTOR('',#19331,1.);
#5509=VECTOR('',#19332,1.);
#5510=VECTOR('',#19333,1.);
#5511=VECTOR('',#19336,1.);
#5512=VECTOR('',#19337,1.);
#5513=VECTOR('',#19338,1.);
#5514=VECTOR('',#19341,1.);
#5515=VECTOR('',#19342,1.);
#5516=VECTOR('',#19343,1.);
#5517=VECTOR('',#19346,1.);
#5518=VECTOR('',#19347,1.);
#5519=VECTOR('',#19348,1.);
#5520=VECTOR('',#19351,1.);
#5521=VECTOR('',#19352,1.);
#5522=VECTOR('',#19369,0.475);
#5523=VECTOR('',#19374,0.5);
#5524=VECTOR('',#19379,0.485);
#5525=VECTOR('',#19388,0.31);
#5526=VECTOR('',#19391,0.3);
#5527=VECTOR('',#19398,0.225);
#5528=VECTOR('',#19405,0.225);
#5529=VECTOR('',#19412,0.225);
#5530=VECTOR('',#19419,0.225);
#5531=VECTOR('',#19426,1.59);
#5532=VECTOR('',#19435,1.2);
#5533=VECTOR('',#19442,2.5);
#5534=VECTOR('',#19455,0.225);
#5535=VECTOR('',#19462,0.225);
#5536=VECTOR('',#19469,0.225);
#5537=VECTOR('',#19476,0.225);
#5538=VECTOR('',#19483,1.59);
#5539=VECTOR('',#19494,1.2);
#5540=VECTOR('',#19499,2.5);
#5541=VECTOR('',#19512,0.225000000000001);
#5542=VECTOR('',#19519,0.225000000000001);
#5543=VECTOR('',#19526,0.225000000000001);
#5544=VECTOR('',#19533,0.225000000000001);
#5545=VECTOR('',#19540,2.34);
#5546=VECTOR('',#19549,1.9);
#5547=VECTOR('',#19556,3.);
#5548=VECTOR('',#19569,0.225000000000001);
#5549=VECTOR('',#19576,0.225000000000001);
#5550=VECTOR('',#19583,0.225000000000001);
#5551=VECTOR('',#19590,0.225000000000001);
#5552=VECTOR('',#19597,2.34);
#5553=VECTOR('',#19608,1.9);
#5554=VECTOR('',#19613,3.);
#5555=VECTOR('',#19638,1.070235);
#5556=VECTOR('',#19645,0.6);
#5557=VECTOR('',#19650,0.63);
#5558=VECTOR('',#19659,1.070235);
#5559=VECTOR('',#19666,0.63);
#5560=VECTOR('',#19685,1.129765);
#5561=VECTOR('',#19696,1.57);
#5562=VECTOR('',#19701,1.6);
#5563=VECTOR('',#19706,1.57);
#5564=VECTOR('',#19711,1.129765);
#5565=VECTOR('',#19758,1.123812);
#5566=VECTOR('',#19827,1.076188);
#5567=VECTOR('',#19856,1.119765);
#5568=VECTOR('',#19863,1.085235);
#5569=VECTOR('',#19874,1.119765);
#5570=VECTOR('',#19881,1.085235);
#5571=VECTOR('',#19910,1.63531);
#5572=VECTOR('',#19917,1.);
#5573=VECTOR('',#19922,1.05);
#5574=VECTOR('',#19931,1.63531);
#5575=VECTOR('',#19938,1.05);
#5576=VECTOR('',#19957,1.71469);
#5577=VECTOR('',#19968,2.3);
#5578=VECTOR('',#19973,2.35);
#5579=VECTOR('',#19978,2.3);
#5580=VECTOR('',#19983,1.71469);
#5581=VECTOR('',#20034,1.706752);
#5582=VECTOR('',#20111,1.643248);
#5583=VECTOR('',#20140,1.70469);
#5584=VECTOR('',#20147,1.65031);
#5585=VECTOR('',#20158,1.70469);
#5586=VECTOR('',#20165,1.65031);
#5587=VECTOR('',#20180,1.);
#5588=VECTOR('',#20181,1.);
#5589=VECTOR('',#20182,1.);
#5590=VECTOR('',#20183,1.);
#5591=VECTOR('',#20186,1.);
#5592=VECTOR('',#20187,1.);
#5593=VECTOR('',#20188,1.);
#5594=VECTOR('',#20191,1.);
#5595=VECTOR('',#20192,1.);
#5596=VECTOR('',#20193,1.);
#5597=VECTOR('',#20196,1.);
#5598=VECTOR('',#20197,1.);
#5599=VECTOR('',#20198,1.);
#5600=VECTOR('',#20201,1.);
#5601=VECTOR('',#20202,1.);
#5602=VECTOR('',#20203,1.);
#5603=VECTOR('',#20206,1.);
#5604=VECTOR('',#20207,1.);
#5605=VECTOR('',#20224,0.325);
#5606=VECTOR('',#20229,0.35);
#5607=VECTOR('',#20234,0.335);
#5608=VECTOR('',#20243,0.21);
#5609=VECTOR('',#20246,0.2);
#5610=VECTOR('',#20251,1.);
#5611=VECTOR('',#20252,1.);
#5612=VECTOR('',#20253,1.);
#5613=VECTOR('',#20254,1.);
#5614=VECTOR('',#20257,1.);
#5615=VECTOR('',#20258,1.);
#5616=VECTOR('',#20259,1.);
#5617=VECTOR('',#20262,1.);
#5618=VECTOR('',#20263,1.);
#5619=VECTOR('',#20264,1.);
#5620=VECTOR('',#20267,1.);
#5621=VECTOR('',#20268,1.);
#5622=VECTOR('',#20273,1.);
#5623=VECTOR('',#20274,1.);
#5624=VECTOR('',#20275,1.);
#5625=VECTOR('',#20276,1.);
#5626=VECTOR('',#20279,1.);
#5627=VECTOR('',#20280,1.);
#5628=VECTOR('',#20281,1.);
#5629=VECTOR('',#20284,1.);
#5630=VECTOR('',#20285,1.);
#5631=VECTOR('',#20286,1.);
#5632=VECTOR('',#20289,1.);
#5633=VECTOR('',#20290,1.);
#5634=VECTOR('',#20295,1.);
#5635=VECTOR('',#20296,1.);
#5636=VECTOR('',#20297,1.);
#5637=VECTOR('',#20298,1.);
#5638=VECTOR('',#20301,1.);
#5639=VECTOR('',#20302,1.);
#5640=VECTOR('',#20303,1.);
#5641=VECTOR('',#20306,1.);
#5642=VECTOR('',#20307,1.);
#5643=VECTOR('',#20308,1.);
#5644=VECTOR('',#20311,1.);
#5645=VECTOR('',#20312,1.);
#5646=VECTOR('',#20317,1.);
#5647=VECTOR('',#20318,1.);
#5648=VECTOR('',#20319,1.);
#5649=VECTOR('',#20320,1.);
#5650=VECTOR('',#20323,1.);
#5651=VECTOR('',#20324,1.);
#5652=VECTOR('',#20325,1.);
#5653=VECTOR('',#20328,1.);
#5654=VECTOR('',#20329,1.);
#5655=VECTOR('',#20330,1.);
#5656=VECTOR('',#20333,1.);
#5657=VECTOR('',#20334,1.);
#5658=VECTOR('',#20339,1.);
#5659=VECTOR('',#20340,1.);
#5660=VECTOR('',#20341,1.);
#5661=VECTOR('',#20342,1.);
#5662=VECTOR('',#20345,1.);
#5663=VECTOR('',#20346,1.);
#5664=VECTOR('',#20347,1.);
#5665=VECTOR('',#20350,1.);
#5666=VECTOR('',#20351,1.);
#5667=VECTOR('',#20352,1.);
#5668=VECTOR('',#20355,1.);
#5669=VECTOR('',#20356,1.);
#5670=VECTOR('',#20361,1.);
#5671=VECTOR('',#20362,1.);
#5672=VECTOR('',#20363,1.);
#5673=VECTOR('',#20364,1.);
#5674=VECTOR('',#20367,1.);
#5675=VECTOR('',#20368,1.);
#5676=VECTOR('',#20369,1.);
#5677=VECTOR('',#20372,1.);
#5678=VECTOR('',#20373,1.);
#5679=VECTOR('',#20374,1.);
#5680=VECTOR('',#20377,1.);
#5681=VECTOR('',#20378,1.);
#5682=VECTOR('',#20383,1.);
#5683=VECTOR('',#20384,1.);
#5684=VECTOR('',#20385,1.);
#5685=VECTOR('',#20386,1.);
#5686=VECTOR('',#20389,1.);
#5687=VECTOR('',#20390,1.);
#5688=VECTOR('',#20391,1.);
#5689=VECTOR('',#20394,1.);
#5690=VECTOR('',#20395,1.);
#5691=VECTOR('',#20396,1.);
#5692=VECTOR('',#20399,1.);
#5693=VECTOR('',#20400,1.);
#5694=VECTOR('',#20405,1.);
#5695=VECTOR('',#20406,1.);
#5696=VECTOR('',#20407,1.);
#5697=VECTOR('',#20408,1.);
#5698=VECTOR('',#20411,1.);
#5699=VECTOR('',#20412,1.);
#5700=VECTOR('',#20413,1.);
#5701=VECTOR('',#20416,1.);
#5702=VECTOR('',#20417,1.);
#5703=VECTOR('',#20418,1.);
#5704=VECTOR('',#20421,1.);
#5705=VECTOR('',#20422,1.);
#5706=VECTOR('',#20427,1.);
#5707=VECTOR('',#20428,1.);
#5708=VECTOR('',#20429,1.);
#5709=VECTOR('',#20430,1.);
#5710=VECTOR('',#20433,1.);
#5711=VECTOR('',#20434,1.);
#5712=VECTOR('',#20435,1.);
#5713=VECTOR('',#20438,1.);
#5714=VECTOR('',#20439,1.);
#5715=VECTOR('',#20440,1.);
#5716=VECTOR('',#20443,1.);
#5717=VECTOR('',#20444,1.);
#5718=VECTOR('',#20449,1.);
#5719=VECTOR('',#20450,1.);
#5720=VECTOR('',#20451,1.);
#5721=VECTOR('',#20452,1.);
#5722=VECTOR('',#20455,1.);
#5723=VECTOR('',#20456,1.);
#5724=VECTOR('',#20457,1.);
#5725=VECTOR('',#20460,1.);
#5726=VECTOR('',#20461,1.);
#5727=VECTOR('',#20462,1.);
#5728=VECTOR('',#20465,1.);
#5729=VECTOR('',#20466,1.);
#5730=VECTOR('',#20471,1.);
#5731=VECTOR('',#20472,1.);
#5732=VECTOR('',#20473,1.);
#5733=VECTOR('',#20474,1.);
#5734=VECTOR('',#20477,1.);
#5735=VECTOR('',#20478,1.);
#5736=VECTOR('',#20479,1.);
#5737=VECTOR('',#20482,1.);
#5738=VECTOR('',#20483,1.);
#5739=VECTOR('',#20484,1.);
#5740=VECTOR('',#20487,1.);
#5741=VECTOR('',#20488,1.);
#5742=VECTOR('',#20493,1.);
#5743=VECTOR('',#20494,1.);
#5744=VECTOR('',#20495,1.);
#5745=VECTOR('',#20496,1.);
#5746=VECTOR('',#20499,1.);
#5747=VECTOR('',#20500,1.);
#5748=VECTOR('',#20501,1.);
#5749=VECTOR('',#20504,1.);
#5750=VECTOR('',#20505,1.);
#5751=VECTOR('',#20506,1.);
#5752=VECTOR('',#20509,1.);
#5753=VECTOR('',#20510,1.);
#5754=VECTOR('',#20515,1.);
#5755=VECTOR('',#20516,1.);
#5756=VECTOR('',#20517,1.);
#5757=VECTOR('',#20518,1.);
#5758=VECTOR('',#20521,1.);
#5759=VECTOR('',#20522,1.);
#5760=VECTOR('',#20523,1.);
#5761=VECTOR('',#20526,1.);
#5762=VECTOR('',#20527,1.);
#5763=VECTOR('',#20528,1.);
#5764=VECTOR('',#20531,1.);
#5765=VECTOR('',#20532,1.);
#5766=VECTOR('',#20537,1.);
#5767=VECTOR('',#20538,1.);
#5768=VECTOR('',#20539,1.);
#5769=VECTOR('',#20540,1.);
#5770=VECTOR('',#20543,1.);
#5771=VECTOR('',#20544,1.);
#5772=VECTOR('',#20545,1.);
#5773=VECTOR('',#20548,1.);
#5774=VECTOR('',#20549,1.);
#5775=VECTOR('',#20550,1.);
#5776=VECTOR('',#20553,1.);
#5777=VECTOR('',#20554,1.);
#5778=VECTOR('',#20559,1.);
#5779=VECTOR('',#20560,1.);
#5780=VECTOR('',#20561,1.);
#5781=VECTOR('',#20562,1.);
#5782=VECTOR('',#20565,1.);
#5783=VECTOR('',#20566,1.);
#5784=VECTOR('',#20567,1.);
#5785=VECTOR('',#20570,1.);
#5786=VECTOR('',#20571,1.);
#5787=VECTOR('',#20572,1.);
#5788=VECTOR('',#20575,1.);
#5789=VECTOR('',#20576,1.);
#5790=VECTOR('',#20581,1.);
#5791=VECTOR('',#20582,1.);
#5792=VECTOR('',#20583,1.);
#5793=VECTOR('',#20584,1.);
#5794=VECTOR('',#20587,1.);
#5795=VECTOR('',#20588,1.);
#5796=VECTOR('',#20589,1.);
#5797=VECTOR('',#20592,1.);
#5798=VECTOR('',#20593,1.);
#5799=VECTOR('',#20594,1.);
#5800=VECTOR('',#20597,1.);
#5801=VECTOR('',#20598,1.);
#5802=VECTOR('',#20603,1.);
#5803=VECTOR('',#20604,1.);
#5804=VECTOR('',#20605,1.);
#5805=VECTOR('',#20606,1.);
#5806=VECTOR('',#20609,1.);
#5807=VECTOR('',#20610,1.);
#5808=VECTOR('',#20611,1.);
#5809=VECTOR('',#20614,1.);
#5810=VECTOR('',#20615,1.);
#5811=VECTOR('',#20616,1.);
#5812=VECTOR('',#20619,1.);
#5813=VECTOR('',#20620,1.);
#5814=VECTOR('',#20625,1.);
#5815=VECTOR('',#20626,1.);
#5816=VECTOR('',#20627,1.);
#5817=VECTOR('',#20628,1.);
#5818=VECTOR('',#20631,1.);
#5819=VECTOR('',#20632,1.);
#5820=VECTOR('',#20633,1.);
#5821=VECTOR('',#20636,1.);
#5822=VECTOR('',#20637,1.);
#5823=VECTOR('',#20638,1.);
#5824=VECTOR('',#20641,1.);
#5825=VECTOR('',#20642,1.);
#5826=VECTOR('',#20647,1.);
#5827=VECTOR('',#20648,1.);
#5828=VECTOR('',#20649,1.);
#5829=VECTOR('',#20650,1.);
#5830=VECTOR('',#20653,1.);
#5831=VECTOR('',#20654,1.);
#5832=VECTOR('',#20655,1.);
#5833=VECTOR('',#20658,1.);
#5834=VECTOR('',#20659,1.);
#5835=VECTOR('',#20660,1.);
#5836=VECTOR('',#20663,1.);
#5837=VECTOR('',#20664,1.);
#5838=VECTOR('',#20669,1.);
#5839=VECTOR('',#20670,1.);
#5840=VECTOR('',#20671,1.);
#5841=VECTOR('',#20672,1.);
#5842=VECTOR('',#20675,1.);
#5843=VECTOR('',#20676,1.);
#5844=VECTOR('',#20677,1.);
#5845=VECTOR('',#20680,1.);
#5846=VECTOR('',#20681,1.);
#5847=VECTOR('',#20682,1.);
#5848=VECTOR('',#20685,1.);
#5849=VECTOR('',#20686,1.);
#5850=VECTOR('',#20691,1.);
#5851=VECTOR('',#20692,1.);
#5852=VECTOR('',#20693,1.);
#5853=VECTOR('',#20694,1.);
#5854=VECTOR('',#20697,1.);
#5855=VECTOR('',#20698,1.);
#5856=VECTOR('',#20699,1.);
#5857=VECTOR('',#20702,1.);
#5858=VECTOR('',#20703,1.);
#5859=VECTOR('',#20704,1.);
#5860=VECTOR('',#20707,1.);
#5861=VECTOR('',#20708,1.);
#5862=VECTOR('',#20713,1.);
#5863=VECTOR('',#20714,1.);
#5864=VECTOR('',#20715,1.);
#5865=VECTOR('',#20716,1.);
#5866=VECTOR('',#20719,1.);
#5867=VECTOR('',#20720,1.);
#5868=VECTOR('',#20721,1.);
#5869=VECTOR('',#20724,1.);
#5870=VECTOR('',#20725,1.);
#5871=VECTOR('',#20726,1.);
#5872=VECTOR('',#20729,1.);
#5873=VECTOR('',#20730,1.);
#5874=VECTOR('',#20735,1.);
#5875=VECTOR('',#20736,1.);
#5876=VECTOR('',#20737,1.);
#5877=VECTOR('',#20738,1.);
#5878=VECTOR('',#20741,1.);
#5879=VECTOR('',#20742,1.);
#5880=VECTOR('',#20743,1.);
#5881=VECTOR('',#20746,1.);
#5882=VECTOR('',#20747,1.);
#5883=VECTOR('',#20748,1.);
#5884=VECTOR('',#20751,1.);
#5885=VECTOR('',#20752,1.);
#5886=VECTOR('',#20757,1.);
#5887=VECTOR('',#20758,1.);
#5888=VECTOR('',#20759,1.);
#5889=VECTOR('',#20760,1.);
#5890=VECTOR('',#20763,1.);
#5891=VECTOR('',#20764,1.);
#5892=VECTOR('',#20765,1.);
#5893=VECTOR('',#20768,1.);
#5894=VECTOR('',#20769,1.);
#5895=VECTOR('',#20770,1.);
#5896=VECTOR('',#20773,1.);
#5897=VECTOR('',#20774,1.);
#5898=VECTOR('',#20781,0.225000000000001);
#5899=VECTOR('',#20788,0.225000000000001);
#5900=VECTOR('',#20795,1.525);
#5901=VECTOR('',#20800,1.);
#5902=VECTOR('',#20801,1.);
#5903=VECTOR('',#20802,1.);
#5904=VECTOR('',#20803,1.);
#5905=VECTOR('',#20806,1.);
#5906=VECTOR('',#20807,1.);
#5907=VECTOR('',#20808,1.);
#5908=VECTOR('',#20809,1.);
#5909=VECTOR('',#20812,1.);
#5910=VECTOR('',#20813,1.);
#5911=VECTOR('',#20814,1.);
#5912=VECTOR('',#20817,1.);
#5913=VECTOR('',#20818,1.);
#5914=VECTOR('',#20819,1.);
#5915=VECTOR('',#20822,1.);
#5916=VECTOR('',#20823,1.);
#5917=VECTOR('',#20826,1.);
#5918=VECTOR('',#20827,1.);
#5919=VECTOR('',#20828,1.);
#5920=VECTOR('',#20831,1.);
#5921=VECTOR('',#20836,1.);
#5922=VECTOR('',#20837,1.);
#5923=VECTOR('',#20850,0.164999999999999);
#5924=VECTOR('',#20857,0.5);
#5925=VECTOR('',#20870,0.164999999999999);
#5926=VECTOR('',#20877,0.5);
#5927=VECTOR('',#20888,1.);
#5928=VECTOR('',#20889,1.);
#5929=VECTOR('',#20890,1.);
#5930=VECTOR('',#20891,1.);
#5931=VECTOR('',#20894,1.);
#5932=VECTOR('',#20895,1.);
#5933=VECTOR('',#20896,1.);
#5934=VECTOR('',#20899,1.);
#5935=VECTOR('',#20900,1.);
#5936=VECTOR('',#20901,1.);
#5937=VECTOR('',#20904,1.);
#5938=VECTOR('',#20905,1.);
#5939=VECTOR('',#20914,1.);
#5940=VECTOR('',#20915,1.);
#5941=VECTOR('',#20916,1.);
#5942=VECTOR('',#20917,1.);
#5943=VECTOR('',#20920,1.);
#5944=VECTOR('',#20921,1.);
#5945=VECTOR('',#20922,1.);
#5946=VECTOR('',#20925,1.);
#5947=VECTOR('',#20926,1.);
#5948=VECTOR('',#20927,1.);
#5949=VECTOR('',#20930,1.);
#5950=VECTOR('',#20931,1.);
#5951=VECTOR('',#20940,1.);
#5952=VECTOR('',#20941,1.);
#5953=VECTOR('',#20942,1.);
#5954=VECTOR('',#20943,1.);
#5955=VECTOR('',#20946,1.);
#5956=VECTOR('',#20947,1.);
#5957=VECTOR('',#20948,1.);
#5958=VECTOR('',#20951,1.);
#5959=VECTOR('',#20952,1.);
#5960=VECTOR('',#20953,1.);
#5961=VECTOR('',#20956,1.);
#5962=VECTOR('',#20957,1.);
#5963=VECTOR('',#20958,1.);
#5964=VECTOR('',#20961,1.);
#5965=VECTOR('',#20962,1.);
#5966=VECTOR('',#20963,1.);
#5967=VECTOR('',#20966,1.);
#5968=VECTOR('',#20967,1.);
#5969=VECTOR('',#20980,0.2);
#5970=VECTOR('',#20993,0.325);
#5971=VECTOR('',#20998,0.35);
#5972=VECTOR('',#21003,0.335);
#5973=VECTOR('',#21012,0.21);
#5974=VECTOR('',#21015,0.2);
#5975=VECTOR('',#21024,0.165);
#5976=VECTOR('',#21031,1.);
#5977=VECTOR('',#21032,1.);
#5978=VECTOR('',#21033,1.);
#5979=VECTOR('',#21034,1.);
#5980=VECTOR('',#21039,1.);
#5981=VECTOR('',#21040,1.);
#5982=VECTOR('',#21043,1.);
#5983=VECTOR('',#21044,1.);
#5984=VECTOR('',#21045,1.);
#5985=VECTOR('',#21048,1.);
#5986=VECTOR('',#21055,1.);
#5987=VECTOR('',#21056,1.);
#5988=VECTOR('',#21057,1.);
#5989=VECTOR('',#21058,1.);
#5990=VECTOR('',#21063,1.);
#5991=VECTOR('',#21064,1.);
#5992=VECTOR('',#21067,1.);
#5993=VECTOR('',#21068,1.);
#5994=VECTOR('',#21069,1.);
#5995=VECTOR('',#21072,1.);
#5996=VECTOR('',#21091,0.9);
#5997=VECTOR('',#21094,0.6);
#5998=VECTOR('',#21101,0.6);
#5999=VECTOR('',#21112,0.605);
#6000=VECTOR('',#21119,0.9);
#6001=VECTOR('',#21132,0.605);
#6002=VECTOR('',#21139,0.9);
#6003=VECTOR('',#21150,1.);
#6004=VECTOR('',#21157,0.21);
#6005=VECTOR('',#21162,1.);
#6006=VECTOR('',#21167,0.605);
#6007=VECTOR('',#21174,1.);
#6008=VECTOR('',#21187,0.25);
#6009=VECTOR('',#21192,1.);
#6010=VECTOR('',#21193,1.);
#6011=VECTOR('',#21194,1.);
#6012=VECTOR('',#21195,1.);
#6013=VECTOR('',#21198,1.);
#6014=VECTOR('',#21199,1.);
#6015=VECTOR('',#21200,1.);
#6016=VECTOR('',#21203,1.);
#6017=VECTOR('',#21204,1.);
#6018=VECTOR('',#21205,1.);
#6019=VECTOR('',#21218,1.);
#6020=VECTOR('',#21221,1.);
#6021=VECTOR('',#21226,1.);
#6022=VECTOR('',#21229,1.);
#6023=VECTOR('',#21232,1.);
#6024=VECTOR('',#21233,1.);
#6025=VECTOR('',#21236,1.);
#6026=VECTOR('',#21241,1.);
#6027=VECTOR('',#21244,1.25);
#6028=VECTOR('',#21255,0.605);
#6029=VECTOR('',#21262,0.9);
#6030=VECTOR('',#21275,0.605);
#6031=VECTOR('',#21282,0.9);
#6032=VECTOR('',#21295,0.225);
#6033=VECTOR('',#21302,1.);
#6034=VECTOR('',#21315,0.33);
#6035=VECTOR('',#21322,0.4);
#6036=VECTOR('',#21335,0.32);
#6037=VECTOR('',#21342,0.6);
#6038=VECTOR('',#21353,1.);
#6039=VECTOR('',#21354,1.);
#6040=VECTOR('',#21355,1.);
#6041=VECTOR('',#21356,1.);
#6042=VECTOR('',#21359,1.);
#6043=VECTOR('',#21360,1.);
#6044=VECTOR('',#21361,1.);
#6045=VECTOR('',#21364,1.);
#6046=VECTOR('',#21365,1.);
#6047=VECTOR('',#21366,1.);
#6048=VECTOR('',#21369,1.);
#6049=VECTOR('',#21370,1.);
#6050=VECTOR('',#21371,1.);
#6051=VECTOR('',#21374,1.);
#6052=VECTOR('',#21375,1.);
#6053=VECTOR('',#21376,1.);
#6054=VECTOR('',#21379,1.);
#6055=VECTOR('',#21380,1.);
#6056=VECTOR('',#21393,0.3);
#6057=VECTOR('',#21406,0.475);
#6058=VECTOR('',#21411,0.5);
#6059=VECTOR('',#21416,0.485);
#6060=VECTOR('',#21425,0.31);
#6061=VECTOR('',#21428,0.3);
#6062=VECTOR('',#21437,0.165);
#6063=VECTOR('',#21444,1.);
#6064=VECTOR('',#21445,1.);
#6065=VECTOR('',#21446,1.);
#6066=VECTOR('',#21447,1.);
#6067=VECTOR('',#21452,1.);
#6068=VECTOR('',#21453,1.);
#6069=VECTOR('',#21456,1.);
#6070=VECTOR('',#21457,1.);
#6071=VECTOR('',#21458,1.);
#6072=VECTOR('',#21461,1.);
#6073=VECTOR('',#21480,1.3);
#6074=VECTOR('',#21483,1.);
#6075=VECTOR('',#21490,1.);
#6076=VECTOR('',#21501,1.005);
#6077=VECTOR('',#21508,1.3);
#6078=VECTOR('',#21521,1.005);
#6079=VECTOR('',#21528,1.3);
#6080=VECTOR('',#21539,1.);
#6081=VECTOR('',#21546,0.21);
#6082=VECTOR('',#21551,1.);
#6083=VECTOR('',#21556,1.005);
#6084=VECTOR('',#21563,1.4);
#6085=VECTOR('',#21576,0.225);
#6086=VECTOR('',#21583,1.4);
#6087=VECTOR('',#21598,0.164999999999999);
#6088=VECTOR('',#21605,1.);
#6089=VECTOR('',#21606,1.);
#6090=VECTOR('',#21607,1.);
#6091=VECTOR('',#21608,1.);
#6092=VECTOR('',#21613,1.);
#6093=VECTOR('',#21614,1.);
#6094=VECTOR('',#21617,1.);
#6095=VECTOR('',#21618,1.);
#6096=VECTOR('',#21619,1.);
#6097=VECTOR('',#21622,1.);
#6098=VECTOR('',#21641,0.9);
#6099=VECTOR('',#21644,0.6);
#6100=VECTOR('',#21651,0.6);
#6101=VECTOR('',#21662,0.605);
#6102=VECTOR('',#21669,0.9);
#6103=VECTOR('',#21682,0.605);
#6104=VECTOR('',#21689,0.9);
#6105=VECTOR('',#21700,1.);
#6106=VECTOR('',#21707,0.210000000000001);
#6107=VECTOR('',#21712,1.);
#6108=VECTOR('',#21717,0.605);
#6109=VECTOR('',#21724,1.);
#6110=VECTOR('',#21737,0.225);
#6111=VECTOR('',#21744,1.);
#6112=VECTOR('',#21755,1.);
#6113=VECTOR('',#21756,1.);
#6114=VECTOR('',#21757,1.);
#6115=VECTOR('',#21758,1.);
#6116=VECTOR('',#21761,1.);
#6117=VECTOR('',#21762,1.);
#6118=VECTOR('',#21763,1.);
#6119=VECTOR('',#21766,1.);
#6120=VECTOR('',#21767,1.);
#6121=VECTOR('',#21768,1.);
#6122=VECTOR('',#21773,1.);
#6123=VECTOR('',#21776,1.);
#6124=VECTOR('',#21779,1.);
#6125=VECTOR('',#21782,1.);
#6126=VECTOR('',#21785,1.);
#6127=VECTOR('',#21788,1.);
#6128=VECTOR('',#21791,1.);
#6129=VECTOR('',#21794,1.);
#6130=VECTOR('',#21797,1.);
#6131=VECTOR('',#21800,1.);
#6132=VECTOR('',#21803,1.);
#6133=VECTOR('',#21806,1.);
#6134=VECTOR('',#21809,1.);
#6135=VECTOR('',#21812,1.);
#6136=VECTOR('',#21815,1.);
#6137=VECTOR('',#21818,1.);
#6138=VECTOR('',#21821,1.);
#6139=VECTOR('',#21824,1.);
#6140=VECTOR('',#21827,1.);
#6141=VECTOR('',#21830,1.);
#6142=VECTOR('',#21841,1.4);
#6143=VECTOR('',#21846,1.);
#6144=VECTOR('',#21847,1.);
#6145=VECTOR('',#21850,1.);
#6146=VECTOR('',#21851,1.);
#6147=VECTOR('',#21852,1.);
#6148=VECTOR('',#21857,1.);
#6149=VECTOR('',#21858,1.);
#6150=VECTOR('',#21861,1.);
#6151=VECTOR('',#21862,1.);
#6152=VECTOR('',#21863,1.);
#6153=VECTOR('',#21868,1.);
#6154=VECTOR('',#21869,1.);
#6155=VECTOR('',#21872,1.);
#6156=VECTOR('',#21873,1.);
#6157=VECTOR('',#21874,1.);
#6158=VECTOR('',#21879,1.);
#6159=VECTOR('',#21880,1.);
#6160=VECTOR('',#21883,1.);
#6161=VECTOR('',#21884,1.);
#6162=VECTOR('',#21885,1.);
#6163=VECTOR('',#21890,1.);
#6164=VECTOR('',#21891,1.);
#6165=VECTOR('',#21894,1.);
#6166=VECTOR('',#21895,1.);
#6167=VECTOR('',#21896,1.);
#6168=VECTOR('',#21901,1.);
#6169=VECTOR('',#21902,1.);
#6170=VECTOR('',#21905,1.);
#6171=VECTOR('',#21906,1.);
#6172=VECTOR('',#21907,1.);
#6173=VECTOR('',#21912,1.);
#6174=VECTOR('',#21913,1.);
#6175=VECTOR('',#21916,1.);
#6176=VECTOR('',#21917,1.);
#6177=VECTOR('',#21918,1.);
#6178=VECTOR('',#21923,1.);
#6179=VECTOR('',#21924,1.);
#6180=VECTOR('',#21927,1.);
#6181=VECTOR('',#21928,1.);
#6182=VECTOR('',#21929,1.);
#6183=VECTOR('',#21934,1.);
#6184=VECTOR('',#21935,1.);
#6185=VECTOR('',#21938,1.);
#6186=VECTOR('',#21939,1.);
#6187=VECTOR('',#21940,1.);
#6188=VECTOR('',#21945,1.);
#6189=VECTOR('',#21946,1.);
#6190=VECTOR('',#21949,1.);
#6191=VECTOR('',#21950,1.);
#6192=VECTOR('',#21951,1.);
#6193=VECTOR('',#21956,1.);
#6194=VECTOR('',#21957,1.);
#6195=VECTOR('',#21960,1.);
#6196=VECTOR('',#21961,1.);
#6197=VECTOR('',#21962,1.);
#6198=VECTOR('',#21967,1.);
#6199=VECTOR('',#21968,1.);
#6200=VECTOR('',#21971,1.);
#6201=VECTOR('',#21972,1.);
#6202=VECTOR('',#21973,1.);
#6203=VECTOR('',#21978,1.);
#6204=VECTOR('',#21979,1.);
#6205=VECTOR('',#21982,1.);
#6206=VECTOR('',#21983,1.);
#6207=VECTOR('',#21984,1.);
#6208=VECTOR('',#21989,1.);
#6209=VECTOR('',#21990,1.);
#6210=VECTOR('',#21993,1.);
#6211=VECTOR('',#21994,1.);
#6212=VECTOR('',#21995,1.);
#6213=VECTOR('',#22000,1.);
#6214=VECTOR('',#22001,1.);
#6215=VECTOR('',#22004,1.);
#6216=VECTOR('',#22005,1.);
#6217=VECTOR('',#22006,1.);
#6218=VECTOR('',#22011,1.);
#6219=VECTOR('',#22012,1.);
#6220=VECTOR('',#22015,1.);
#6221=VECTOR('',#22016,1.);
#6222=VECTOR('',#22017,1.);
#6223=VECTOR('',#22022,1.);
#6224=VECTOR('',#22023,1.);
#6225=VECTOR('',#22026,1.);
#6226=VECTOR('',#22027,1.);
#6227=VECTOR('',#22028,1.);
#6228=VECTOR('',#22033,1.);
#6229=VECTOR('',#22034,1.);
#6230=VECTOR('',#22037,1.);
#6231=VECTOR('',#22038,1.);
#6232=VECTOR('',#22039,1.);
#6233=VECTOR('',#22044,1.);
#6234=VECTOR('',#22045,1.);
#6235=VECTOR('',#22048,1.);
#6236=VECTOR('',#22049,1.);
#6237=VECTOR('',#22050,1.);
#6238=VECTOR('',#22055,1.);
#6239=VECTOR('',#22056,1.);
#6240=VECTOR('',#22059,1.);
#6241=VECTOR('',#22060,1.);
#6242=VECTOR('',#22061,1.);
#6243=VECTOR('',#22072,1.);
#6244=VECTOR('',#22073,1.);
#6245=VECTOR('',#22074,1.);
#6246=VECTOR('',#22075,1.);
#6247=VECTOR('',#22076,1.);
#6248=VECTOR('',#22077,1.);
#6249=VECTOR('',#22078,1.);
#6250=VECTOR('',#22079,1.);
#6251=VECTOR('',#22082,1.);
#6252=VECTOR('',#22083,1.);
#6253=VECTOR('',#22084,1.);
#6254=VECTOR('',#22087,1.);
#6255=VECTOR('',#22088,1.);
#6256=VECTOR('',#22091,1.);
#6257=VECTOR('',#22092,1.);
#6258=VECTOR('',#22095,1.);
#6259=VECTOR('',#22096,1.);
#6260=VECTOR('',#22099,1.);
#6261=VECTOR('',#22100,1.);
#6262=VECTOR('',#22101,1.);
#6263=VECTOR('',#22102,1.);
#6264=VECTOR('',#22105,1.);
#6265=VECTOR('',#22108,1.);
#6266=VECTOR('',#22111,1.);
#6267=VECTOR('',#22122,0.164999999999999);
#6268=VECTOR('',#22129,1.);
#6269=VECTOR('',#22130,1.);
#6270=VECTOR('',#22131,1.);
#6271=VECTOR('',#22132,1.);
#6272=VECTOR('',#22137,1.);
#6273=VECTOR('',#22138,1.);
#6274=VECTOR('',#22141,1.);
#6275=VECTOR('',#22142,1.);
#6276=VECTOR('',#22143,1.);
#6277=VECTOR('',#22146,1.);
#6278=VECTOR('',#22165,1.3);
#6279=VECTOR('',#22168,1.);
#6280=VECTOR('',#22175,1.);
#6281=VECTOR('',#22186,1.005);
#6282=VECTOR('',#22193,1.3);
#6283=VECTOR('',#22206,1.005);
#6284=VECTOR('',#22213,1.3);
#6285=VECTOR('',#22224,1.);
#6286=VECTOR('',#22231,0.210000000000001);
#6287=VECTOR('',#22236,1.);
#6288=VECTOR('',#22241,1.005);
#6289=VECTOR('',#22248,1.4);
#6290=VECTOR('',#22261,1.005);
#6291=VECTOR('',#22268,1.4);
#6292=VECTOR('',#22281,1.005);
#6293=VECTOR('',#22288,1.4);
#6294=VECTOR('',#22299,1.);
#6295=VECTOR('',#22306,0.210000000000001);
#6296=VECTOR('',#22311,1.);
#6297=VECTOR('',#22314,1.);
#6298=VECTOR('',#22315,1.);
#6299=VECTOR('',#22316,1.);
#6300=VECTOR('',#22317,1.);
#6301=VECTOR('',#22322,1.);
#6302=VECTOR('',#22327,1.);
#6303=VECTOR('',#22330,1.);
#6304=VECTOR('',#22335,1.);
#6305=VECTOR('',#22342,1.5);
#6306=VECTOR('',#22355,0.225000000000001);
#6307=VECTOR('',#22362,1.4);
#6308=VECTOR('',#22373,1.);
#6309=VECTOR('',#22374,1.);
#6310=VECTOR('',#22375,1.);
#6311=VECTOR('',#22376,1.);
#6312=VECTOR('',#22379,1.);
#6313=VECTOR('',#22380,1.);
#6314=VECTOR('',#22381,1.);
#6315=VECTOR('',#22384,1.);
#6316=VECTOR('',#22385,1.);
#6317=VECTOR('',#22386,1.);
#6318=VECTOR('',#22391,1.);
#6319=VECTOR('',#22394,1.);
#6320=VECTOR('',#22397,1.);
#6321=VECTOR('',#22400,1.);
#6322=VECTOR('',#22403,1.);
#6323=VECTOR('',#22406,1.);
#6324=VECTOR('',#22409,1.);
#6325=VECTOR('',#22412,1.);
#6326=VECTOR('',#22415,1.);
#6327=VECTOR('',#22418,1.);
#6328=VECTOR('',#22421,1.);
#6329=VECTOR('',#22424,1.);
#6330=VECTOR('',#22427,1.);
#6331=VECTOR('',#22430,1.);
#6332=VECTOR('',#22433,1.);
#6333=VECTOR('',#22436,1.);
#6334=VECTOR('',#22439,1.);
#6335=VECTOR('',#22442,1.);
#6336=VECTOR('',#22445,1.);
#6337=VECTOR('',#22448,1.);
#6338=VECTOR('',#22451,1.);
#6339=VECTOR('',#22454,1.);
#6340=VECTOR('',#22457,1.);
#6341=VECTOR('',#22460,1.);
#6342=VECTOR('',#22463,1.);
#6343=VECTOR('',#22466,1.);
#6344=VECTOR('',#22469,1.);
#6345=VECTOR('',#22472,1.);
#6346=VECTOR('',#22475,1.);
#6347=VECTOR('',#22478,1.);
#6348=VECTOR('',#22481,1.);
#6349=VECTOR('',#22484,1.);
#6350=VECTOR('',#22487,1.);
#6351=VECTOR('',#22490,1.);
#6352=VECTOR('',#22493,1.);
#6353=VECTOR('',#22496,1.);
#6354=VECTOR('',#22499,1.);
#6355=VECTOR('',#22502,1.);
#6356=VECTOR('',#22505,1.);
#6357=VECTOR('',#22508,1.);
#6358=VECTOR('',#22519,2.);
#6359=VECTOR('',#22524,1.);
#6360=VECTOR('',#22525,1.);
#6361=VECTOR('',#22528,1.);
#6362=VECTOR('',#22533,1.);
#6363=VECTOR('',#22534,1.);
#6364=VECTOR('',#22537,1.);
#6365=VECTOR('',#22542,1.);
#6366=VECTOR('',#22543,1.);
#6367=VECTOR('',#22546,1.);
#6368=VECTOR('',#22551,1.);
#6369=VECTOR('',#22552,1.);
#6370=VECTOR('',#22555,1.);
#6371=VECTOR('',#22560,1.);
#6372=VECTOR('',#22561,1.);
#6373=VECTOR('',#22564,1.);
#6374=VECTOR('',#22569,1.);
#6375=VECTOR('',#22570,1.);
#6376=VECTOR('',#22573,1.);
#6377=VECTOR('',#22578,1.);
#6378=VECTOR('',#22579,1.);
#6379=VECTOR('',#22582,1.);
#6380=VECTOR('',#22587,1.);
#6381=VECTOR('',#22588,1.);
#6382=VECTOR('',#22591,1.);
#6383=VECTOR('',#22596,1.);
#6384=VECTOR('',#22597,1.);
#6385=VECTOR('',#22600,1.);
#6386=VECTOR('',#22605,1.);
#6387=VECTOR('',#22606,1.);
#6388=VECTOR('',#22609,1.);
#6389=VECTOR('',#22614,1.);
#6390=VECTOR('',#22615,1.);
#6391=VECTOR('',#22618,1.);
#6392=VECTOR('',#22623,1.);
#6393=VECTOR('',#22624,1.);
#6394=VECTOR('',#22627,1.);
#6395=VECTOR('',#22632,1.);
#6396=VECTOR('',#22633,1.);
#6397=VECTOR('',#22636,1.);
#6398=VECTOR('',#22641,1.);
#6399=VECTOR('',#22642,1.);
#6400=VECTOR('',#22645,1.);
#6401=VECTOR('',#22650,1.);
#6402=VECTOR('',#22651,1.);
#6403=VECTOR('',#22654,1.);
#6404=VECTOR('',#22659,1.);
#6405=VECTOR('',#22660,1.);
#6406=VECTOR('',#22663,1.);
#6407=VECTOR('',#22668,1.);
#6408=VECTOR('',#22669,1.);
#6409=VECTOR('',#22672,1.);
#6410=VECTOR('',#22677,1.);
#6411=VECTOR('',#22678,1.);
#6412=VECTOR('',#22681,1.);
#6413=VECTOR('',#22686,1.);
#6414=VECTOR('',#22687,1.);
#6415=VECTOR('',#22690,1.);
#6416=VECTOR('',#22695,1.);
#6417=VECTOR('',#22696,1.);
#6418=VECTOR('',#22699,1.);
#6419=VECTOR('',#22704,1.);
#6420=VECTOR('',#22705,1.);
#6421=VECTOR('',#22708,1.);
#6422=VECTOR('',#22713,1.);
#6423=VECTOR('',#22714,1.);
#6424=VECTOR('',#22717,1.);
#6425=VECTOR('',#22722,1.);
#6426=VECTOR('',#22723,1.);
#6427=VECTOR('',#22726,1.);
#6428=VECTOR('',#22731,1.);
#6429=VECTOR('',#22732,1.);
#6430=VECTOR('',#22735,1.);
#6431=VECTOR('',#22740,1.);
#6432=VECTOR('',#22741,1.);
#6433=VECTOR('',#22744,1.);
#6434=VECTOR('',#22749,1.);
#6435=VECTOR('',#22750,1.);
#6436=VECTOR('',#22753,1.);
#6437=VECTOR('',#22758,1.);
#6438=VECTOR('',#22759,1.);
#6439=VECTOR('',#22762,1.);
#6440=VECTOR('',#22767,1.);
#6441=VECTOR('',#22768,1.);
#6442=VECTOR('',#22771,1.);
#6443=VECTOR('',#22776,1.);
#6444=VECTOR('',#22777,1.);
#6445=VECTOR('',#22780,1.);
#6446=VECTOR('',#22785,1.);
#6447=VECTOR('',#22786,1.);
#6448=VECTOR('',#22789,1.);
#6449=VECTOR('',#22794,1.);
#6450=VECTOR('',#22795,1.);
#6451=VECTOR('',#22798,1.);
#6452=VECTOR('',#22803,1.);
#6453=VECTOR('',#22804,1.);
#6454=VECTOR('',#22807,1.);
#6455=VECTOR('',#22812,1.);
#6456=VECTOR('',#22813,1.);
#6457=VECTOR('',#22816,1.);
#6458=VECTOR('',#22821,1.);
#6459=VECTOR('',#22822,1.);
#6460=VECTOR('',#22825,1.);
#6461=VECTOR('',#22830,1.);
#6462=VECTOR('',#22831,1.);
#6463=VECTOR('',#22834,1.);
#6464=VECTOR('',#22839,1.);
#6465=VECTOR('',#22840,1.);
#6466=VECTOR('',#22843,1.);
#6467=VECTOR('',#22848,1.);
#6468=VECTOR('',#22849,1.);
#6469=VECTOR('',#22852,1.);
#6470=VECTOR('',#22857,1.);
#6471=VECTOR('',#22858,1.);
#6472=VECTOR('',#22861,1.);
#6473=VECTOR('',#22866,1.);
#6474=VECTOR('',#22869,1.);
#6475=VECTOR('',#22870,1.);
#6476=VECTOR('',#22875,1.);
#6477=VECTOR('',#22876,1.);
#6478=VECTOR('',#22879,1.);
#6479=VECTOR('',#22890,1.);
#6480=VECTOR('',#22891,1.);
#6481=VECTOR('',#22892,1.);
#6482=VECTOR('',#22893,1.);
#6483=VECTOR('',#22894,1.);
#6484=VECTOR('',#22895,1.);
#6485=VECTOR('',#22896,1.);
#6486=VECTOR('',#22897,1.);
#6487=VECTOR('',#22900,1.);
#6488=VECTOR('',#22901,1.);
#6489=VECTOR('',#22902,1.);
#6490=VECTOR('',#22905,1.);
#6491=VECTOR('',#22906,1.);
#6492=VECTOR('',#22909,1.);
#6493=VECTOR('',#22910,1.);
#6494=VECTOR('',#22913,1.);
#6495=VECTOR('',#22914,1.);
#6496=VECTOR('',#22917,1.);
#6497=VECTOR('',#22918,1.);
#6498=VECTOR('',#22919,1.);
#6499=VECTOR('',#22920,1.);
#6500=VECTOR('',#22923,1.);
#6501=VECTOR('',#22926,1.);
#6502=VECTOR('',#22929,1.);
#6503=VECTOR('',#22936,1.);
#6504=VECTOR('',#22937,1.);
#6505=VECTOR('',#22938,1.);
#6506=VECTOR('',#22939,1.);
#6507=VECTOR('',#22942,1.);
#6508=VECTOR('',#22943,1.);
#6509=VECTOR('',#22944,1.);
#6510=VECTOR('',#22947,1.);
#6511=VECTOR('',#22948,1.);
#6512=VECTOR('',#22949,1.);
#6513=VECTOR('',#22952,1.);
#6514=VECTOR('',#22953,1.);
#6515=VECTOR('',#22954,1.);
#6516=VECTOR('',#22957,1.);
#6517=VECTOR('',#22958,1.);
#6518=VECTOR('',#22959,1.);
#6519=VECTOR('',#22962,1.);
#6520=VECTOR('',#22963,1.);
#6521=VECTOR('',#22974,0.235);
#6522=VECTOR('',#22979,0.25);
#6523=VECTOR('',#22984,0.2125);
#6524=VECTOR('',#22997,0.325);
#6525=VECTOR('',#23002,0.35);
#6526=VECTOR('',#23007,0.335);
#6527=VECTOR('',#23016,0.21);
#6528=VECTOR('',#23021,0.2);
#6529=VECTOR('',#23026,0.18);
#6530=VECTOR('',#23031,1.);
#6531=VECTOR('',#23032,1.);
#6532=VECTOR('',#23033,1.);
#6533=VECTOR('',#23034,1.);
#6534=VECTOR('',#23037,1.);
#6535=VECTOR('',#23038,1.);
#6536=VECTOR('',#23039,1.);
#6537=VECTOR('',#23042,1.);
#6538=VECTOR('',#23043,1.);
#6539=VECTOR('',#23044,1.);
#6540=VECTOR('',#23047,1.);
#6541=VECTOR('',#23048,1.);
#6542=VECTOR('',#23049,1.);
#6543=VECTOR('',#23052,1.);
#6544=VECTOR('',#23053,1.);
#6545=VECTOR('',#23054,1.);
#6546=VECTOR('',#23057,1.);
#6547=VECTOR('',#23058,1.);
#6548=VECTOR('',#23281,0.405);
#6549=VECTOR('',#23288,0.9);
#6550=CIRCLE('',#17162,0.25);
#6551=CIRCLE('',#17163,0.25);
#6552=CIRCLE('',#17165,0.25);
#6553=CIRCLE('',#17166,0.25);
#6554=CIRCLE('',#17168,0.25);
#6555=CIRCLE('',#17169,0.25);
#6556=CIRCLE('',#17178,0.225000000000001);
#6557=CIRCLE('',#17179,0.225000000000001);
#6558=CIRCLE('',#17181,0.225000000000001);
#6559=CIRCLE('',#17182,0.225000000000001);
#6560=CIRCLE('',#17184,0.164999999999999);
#6561=CIRCLE('',#17185,0.164999999999999);
#6562=CIRCLE('',#17187,0.164999999999999);
#6563=CIRCLE('',#17188,0.164999999999999);
#6564=CIRCLE('',#17190,0.164999999999999);
#6565=CIRCLE('',#17191,0.164999999999999);
#6566=CIRCLE('',#17193,0.164999999999999);
#6567=CIRCLE('',#17194,0.164999999999999);
#6568=CIRCLE('',#17196,2.35);
#6569=CIRCLE('',#17197,2.35);
#6570=CIRCLE('',#17199,0.164999999999999);
#6571=CIRCLE('',#17200,0.164999999999999);
#6572=CIRCLE('',#17202,0.164999999999999);
#6573=CIRCLE('',#17203,0.164999999999999);
#6574=CIRCLE('',#17205,0.164999999999999);
#6575=CIRCLE('',#17206,0.164999999999999);
#6576=CIRCLE('',#17208,0.164999999999999);
#6577=CIRCLE('',#17209,0.164999999999999);
#6578=CIRCLE('',#17211,1.6);
#6579=CIRCLE('',#17212,1.6);
#6580=CIRCLE('',#17214,0.165);
#6581=CIRCLE('',#17215,0.165);
#6582=CIRCLE('',#17217,0.165);
#6583=CIRCLE('',#17218,0.165);
#6584=CIRCLE('',#17220,0.165);
#6585=CIRCLE('',#17221,0.165);
#6586=CIRCLE('',#17223,0.165);
#6587=CIRCLE('',#17224,0.165);
#6588=CIRCLE('',#17226,2.35);
#6589=CIRCLE('',#17227,2.35);
#6590=CIRCLE('',#17229,0.165);
#6591=CIRCLE('',#17230,0.165);
#6592=CIRCLE('',#17232,0.165);
#6593=CIRCLE('',#17233,0.165);
#6594=CIRCLE('',#17235,0.165);
#6595=CIRCLE('',#17236,0.165);
#6596=CIRCLE('',#17238,0.165);
#6597=CIRCLE('',#17239,0.165);
#6598=CIRCLE('',#17241,1.6);
#6599=CIRCLE('',#17242,1.6);
#6600=CIRCLE('',#17244,0.33);
#6601=CIRCLE('',#17245,0.33);
#6602=CIRCLE('',#17247,0.33);
#6603=CIRCLE('',#17248,0.33);
#6604=CIRCLE('',#17250,0.329999999999998);
#6605=CIRCLE('',#17251,0.329999999999998);
#6606=CIRCLE('',#17262,0.225);
#6607=CIRCLE('',#17263,0.225);
#6608=CIRCLE('',#17265,0.225);
#6609=CIRCLE('',#17266,0.225);
#6610=CIRCLE('',#17268,0.225);
#6611=CIRCLE('',#17269,0.225);
#6612=CIRCLE('',#17271,0.225);
#6613=CIRCLE('',#17272,0.225);
#6614=CIRCLE('',#17274,1.59);
#6615=CIRCLE('',#17275,1.59);
#6616=CIRCLE('',#17277,1.2);
#6617=CIRCLE('',#17279,1.2);
#6618=CIRCLE('',#17281,2.5);
#6619=CIRCLE('',#17282,2.5);
#6620=CIRCLE('',#17287,0.225);
#6621=CIRCLE('',#17288,0.225);
#6622=CIRCLE('',#17290,0.225);
#6623=CIRCLE('',#17291,0.225);
#6624=CIRCLE('',#17293,0.225);
#6625=CIRCLE('',#17294,0.225);
#6626=CIRCLE('',#17296,0.225);
#6627=CIRCLE('',#17297,0.225);
#6628=CIRCLE('',#17299,1.59);
#6629=CIRCLE('',#17300,1.59);
#6630=CIRCLE('',#17302,1.2);
#6631=CIRCLE('',#17304,1.2);
#6632=CIRCLE('',#17306,2.5);
#6633=CIRCLE('',#17307,2.5);
#6634=CIRCLE('',#17312,0.225);
#6635=CIRCLE('',#17313,0.225);
#6636=CIRCLE('',#17315,0.225);
#6637=CIRCLE('',#17316,0.225);
#6638=CIRCLE('',#17318,0.225000000000001);
#6639=CIRCLE('',#17319,0.225000000000001);
#6640=CIRCLE('',#17321,0.225000000000001);
#6641=CIRCLE('',#17322,0.225000000000001);
#6642=CIRCLE('',#17324,2.34);
#6643=CIRCLE('',#17325,2.34);
#6644=CIRCLE('',#17327,1.9);
#6645=CIRCLE('',#17329,1.9);
#6646=CIRCLE('',#17331,3.);
#6647=CIRCLE('',#17332,3.);
#6648=CIRCLE('',#17337,0.225);
#6649=CIRCLE('',#17338,0.225);
#6650=CIRCLE('',#17340,0.225);
#6651=CIRCLE('',#17341,0.225);
#6652=CIRCLE('',#17343,0.225000000000001);
#6653=CIRCLE('',#17344,0.225000000000001);
#6654=CIRCLE('',#17346,0.225000000000001);
#6655=CIRCLE('',#17347,0.225000000000001);
#6656=CIRCLE('',#17349,2.34);
#6657=CIRCLE('',#17350,2.34);
#6658=CIRCLE('',#17352,1.9);
#6659=CIRCLE('',#17354,1.9);
#6660=CIRCLE('',#17356,3.);
#6661=CIRCLE('',#17357,3.);
#6662=CIRCLE('',#17370,0.2942);
#6663=CIRCLE('',#17372,0.45);
#6664=CIRCLE('',#17374,0.5);
#6665=CIRCLE('',#17376,0.5);
#6666=CIRCLE('',#17378,0.47);
#6667=CIRCLE('',#17380,0.32);
#6668=CIRCLE('',#17382,0.2942);
#6669=CIRCLE('',#17386,0.225);
#6670=CIRCLE('',#17387,0.225);
#6671=CIRCLE('',#17389,0.225);
#6672=CIRCLE('',#17390,0.225);
#6673=CIRCLE('',#17392,0.225);
#6674=CIRCLE('',#17393,0.225);
#6675=CIRCLE('',#17395,0.225);
#6676=CIRCLE('',#17396,0.225);
#6677=CIRCLE('',#17398,1.59);
#6678=CIRCLE('',#17399,1.59);
#6679=CIRCLE('',#17401,1.2);
#6680=CIRCLE('',#17403,1.2);
#6681=CIRCLE('',#17405,2.5);
#6682=CIRCLE('',#17406,2.5);
#6683=CIRCLE('',#17411,0.225);
#6684=CIRCLE('',#17412,0.225);
#6685=CIRCLE('',#17414,0.225);
#6686=CIRCLE('',#17415,0.225);
#6687=CIRCLE('',#17417,0.225);
#6688=CIRCLE('',#17418,0.225);
#6689=CIRCLE('',#17420,0.225);
#6690=CIRCLE('',#17421,0.225);
#6691=CIRCLE('',#17423,1.59);
#6692=CIRCLE('',#17424,1.59);
#6693=CIRCLE('',#17426,1.2);
#6694=CIRCLE('',#17428,1.2);
#6695=CIRCLE('',#17430,2.5);
#6696=CIRCLE('',#17431,2.5);
#6697=CIRCLE('',#17436,0.225000000000001);
#6698=CIRCLE('',#17437,0.225000000000001);
#6699=CIRCLE('',#17439,0.225000000000001);
#6700=CIRCLE('',#17440,0.225000000000001);
#6701=CIRCLE('',#17442,0.225000000000001);
#6702=CIRCLE('',#17443,0.225000000000001);
#6703=CIRCLE('',#17445,0.225000000000001);
#6704=CIRCLE('',#17446,0.225000000000001);
#6705=CIRCLE('',#17448,2.34);
#6706=CIRCLE('',#17449,2.34);
#6707=CIRCLE('',#17451,1.9);
#6708=CIRCLE('',#17453,1.9);
#6709=CIRCLE('',#17455,3.);
#6710=CIRCLE('',#17456,3.);
#6711=CIRCLE('',#17461,0.225000000000001);
#6712=CIRCLE('',#17462,0.225000000000001);
#6713=CIRCLE('',#17464,0.225000000000001);
#6714=CIRCLE('',#17465,0.225000000000001);
#6715=CIRCLE('',#17467,0.225000000000001);
#6716=CIRCLE('',#17468,0.225000000000001);
#6717=CIRCLE('',#17470,0.225000000000001);
#6718=CIRCLE('',#17471,0.225000000000001);
#6719=CIRCLE('',#17473,2.34);
#6720=CIRCLE('',#17474,2.34);
#6721=CIRCLE('',#17476,1.9);
#6722=CIRCLE('',#17478,1.9);
#6723=CIRCLE('',#17480,3.);
#6724=CIRCLE('',#17481,3.);
#6725=CIRCLE('',#17487,1.070235);
#6726=CIRCLE('',#17488,1.070235);
#6727=CIRCLE('',#17489,0.309556);
#6728=CIRCLE('',#17490,1.070235);
#6729=CIRCLE('',#17491,1.070235);
#6730=CIRCLE('',#17493,1.070235);
#6731=CIRCLE('',#17495,0.6);
#6732=CIRCLE('',#17496,0.6);
#6733=CIRCLE('',#17498,0.66);
#6734=CIRCLE('',#17501,1.070235);
#6735=CIRCLE('',#17503,0.66);
#6736=CIRCLE('',#17507,1.129765);
#6737=CIRCLE('',#17508,1.129765);
#6738=CIRCLE('',#17509,0.309556);
#6739=CIRCLE('',#17510,1.129765);
#6740=CIRCLE('',#17511,1.129765);
#6741=CIRCLE('',#17513,1.129765);
#6742=CIRCLE('',#17515,1.54);
#6743=CIRCLE('',#17516,1.129765);
#6744=CIRCLE('',#17518,1.6);
#6745=CIRCLE('',#17520,1.6);
#6746=CIRCLE('',#17522,1.54);
#6747=CIRCLE('',#17527,0.29765);
#6748=CIRCLE('',#17529,0.29765);
#6749=CIRCLE('',#17531,0.29765);
#6750=CIRCLE('',#17533,0.29765);
#6751=CIRCLE('',#17535,0.29765);
#6752=CIRCLE('',#17537,0.29765);
#6753=CIRCLE('',#17539,0.29765);
#6754=CIRCLE('',#17542,0.303778037777585);
#6755=CIRCLE('',#17543,0.303778037777585);
#6756=CIRCLE('',#17545,1.123812);
#6757=CIRCLE('',#17546,1.123812);
#6758=CIRCLE('',#17547,1.123812);
#6759=CIRCLE('',#17548,1.123812);
#6760=CIRCLE('',#17549,1.123812);
#6761=CIRCLE('',#17550,1.123812);
#6762=CIRCLE('',#17551,1.123812);
#6763=CIRCLE('',#17552,1.123812);
#6764=CIRCLE('',#17553,1.123812);
#6765=CIRCLE('',#17555,1.076188);
#6766=CIRCLE('',#17556,0.303778037777585);
#6767=CIRCLE('',#17558,0.303778037777585);
#6768=CIRCLE('',#17560,1.076188);
#6769=CIRCLE('',#17561,0.303778037777585);
#6770=CIRCLE('',#17563,0.303778037777585);
#6771=CIRCLE('',#17565,1.076188);
#6772=CIRCLE('',#17566,1.076188);
#6773=CIRCLE('',#17567,0.303778037777585);
#6774=CIRCLE('',#17569,0.303778037777585);
#6775=CIRCLE('',#17571,1.076188);
#6776=CIRCLE('',#17572,0.303778037777585);
#6777=CIRCLE('',#17574,0.303778037777585);
#6778=CIRCLE('',#17576,1.076188);
#6779=CIRCLE('',#17577,0.303778037777585);
#6780=CIRCLE('',#17579,0.303778037777585);
#6781=CIRCLE('',#17581,1.076188);
#6782=CIRCLE('',#17582,1.076188);
#6783=CIRCLE('',#17583,1.076188);
#6784=CIRCLE('',#17585,0.303778037777585);
#6785=CIRCLE('',#17587,0.303778037777585);
#6786=CIRCLE('',#17592,1.119765);
#6787=CIRCLE('',#17593,1.085235);
#6788=CIRCLE('',#17595,1.119765);
#6789=CIRCLE('',#17597,1.085235);
#6790=CIRCLE('',#17600,1.119765);
#6791=CIRCLE('',#17601,1.085235);
#6792=CIRCLE('',#17603,1.119765);
#6793=CIRCLE('',#17605,1.085235);
#6794=CIRCLE('',#17615,1.63531);
#6795=CIRCLE('',#17616,1.63531);
#6796=CIRCLE('',#17617,0.412776);
#6797=CIRCLE('',#17618,1.63531);
#6798=CIRCLE('',#17619,1.63531);
#6799=CIRCLE('',#17621,1.63531);
#6800=CIRCLE('',#17623,1.);
#6801=CIRCLE('',#17624,1.);
#6802=CIRCLE('',#17626,1.1);
#6803=CIRCLE('',#17629,1.63531);
#6804=CIRCLE('',#17631,1.1);
#6805=CIRCLE('',#17635,1.71469);
#6806=CIRCLE('',#17636,1.71469);
#6807=CIRCLE('',#17637,0.412776);
#6808=CIRCLE('',#17638,1.71469);
#6809=CIRCLE('',#17639,1.71469);
#6810=CIRCLE('',#17641,1.71469);
#6811=CIRCLE('',#17643,2.25);
#6812=CIRCLE('',#17644,1.71469);
#6813=CIRCLE('',#17646,2.35);
#6814=CIRCLE('',#17648,2.35);
#6815=CIRCLE('',#17650,2.25);
#6816=CIRCLE('',#17655,0.3969);
#6817=CIRCLE('',#17657,0.3969);
#6818=CIRCLE('',#17659,0.3969);
#6819=CIRCLE('',#17661,0.3969);
#6820=CIRCLE('',#17663,0.3969);
#6821=CIRCLE('',#17665,0.3969);
#6822=CIRCLE('',#17667,0.3969);
#6823=CIRCLE('',#17669,0.3969);
#6824=CIRCLE('',#17672,0.405071403305639);
#6825=CIRCLE('',#17673,0.405071403305639);
#6826=CIRCLE('',#17675,1.706752);
#6827=CIRCLE('',#17676,1.706752);
#6828=CIRCLE('',#17677,1.706752);
#6829=CIRCLE('',#17678,1.706752);
#6830=CIRCLE('',#17679,1.706752);
#6831=CIRCLE('',#17680,1.706752);
#6832=CIRCLE('',#17681,1.706752);
#6833=CIRCLE('',#17682,1.706752);
#6834=CIRCLE('',#17683,1.706752);
#6835=CIRCLE('',#17685,1.643248);
#6836=CIRCLE('',#17686,0.405071403305639);
#6837=CIRCLE('',#17688,0.405071403305639);
#6838=CIRCLE('',#17690,1.643248);
#6839=CIRCLE('',#17691,0.405071403305639);
#6840=CIRCLE('',#17693,0.405071403305639);
#6841=CIRCLE('',#17695,1.643248);
#6842=CIRCLE('',#17696,0.405071403305639);
#6843=CIRCLE('',#17698,0.405071403305639);
#6844=CIRCLE('',#17700,1.643248);
#6845=CIRCLE('',#17701,0.405071403305639);
#6846=CIRCLE('',#17703,0.405071403305639);
#6847=CIRCLE('',#17705,1.643248);
#6848=CIRCLE('',#17706,0.405071403305639);
#6849=CIRCLE('',#17708,0.405071403305639);
#6850=CIRCLE('',#17710,1.643248);
#6851=CIRCLE('',#17711,0.405071403305639);
#6852=CIRCLE('',#17713,0.405071403305639);
#6853=CIRCLE('',#17715,1.643248);
#6854=CIRCLE('',#17716,1.643248);
#6855=CIRCLE('',#17717,1.643248);
#6856=CIRCLE('',#17719,0.405071403305639);
#6857=CIRCLE('',#17721,0.405071403305639);
#6858=CIRCLE('',#17726,1.70469);
#6859=CIRCLE('',#17727,1.65031);
#6860=CIRCLE('',#17729,1.70469);
#6861=CIRCLE('',#17731,1.65031);
#6862=CIRCLE('',#17734,1.70469);
#6863=CIRCLE('',#17735,1.65031);
#6864=CIRCLE('',#17737,1.70469);
#6865=CIRCLE('',#17739,1.65031);
#6866=CIRCLE('',#17756,0.1954);
#6867=CIRCLE('',#17758,0.3);
#6868=CIRCLE('',#17760,0.35);
#6869=CIRCLE('',#17762,0.35);
#6870=CIRCLE('',#17764,0.32);
#6871=CIRCLE('',#17766,0.22);
#6872=CIRCLE('',#17768,0.1954);
#6873=CIRCLE('',#17892,0.225000000000001);
#6874=CIRCLE('',#17893,0.225000000000001);
#6875=CIRCLE('',#17895,0.225000000000001);
#6876=CIRCLE('',#17896,0.225000000000001);
#6877=CIRCLE('',#17898,1.525);
#6878=CIRCLE('',#17899,1.525);
#6879=CIRCLE('',#17907,4.);
#6880=CIRCLE('',#17910,4.);
#6881=CIRCLE('',#17914,0.164999999999999);
#6882=CIRCLE('',#17915,0.164999999999999);
#6883=CIRCLE('',#17917,0.5);
#6884=CIRCLE('',#17918,0.5);
#6885=CIRCLE('',#17923,0.164999999999999);
#6886=CIRCLE('',#17924,0.164999999999999);
#6887=CIRCLE('',#17926,0.5);
#6888=CIRCLE('',#17927,0.5);
#6889=CIRCLE('',#17954,0.2);
#6890=CIRCLE('',#17955,0.1954);
#6891=CIRCLE('',#17957,0.2);
#6892=CIRCLE('',#17960,0.3);
#6893=CIRCLE('',#17962,0.35);
#6894=CIRCLE('',#17964,0.35);
#6895=CIRCLE('',#17966,0.32);
#6896=CIRCLE('',#17968,0.22);
#6897=CIRCLE('',#17970,0.1954);
#6898=CIRCLE('',#17975,0.165);
#6899=CIRCLE('',#17976,0.165);
#6900=CIRCLE('',#17980,0.6);
#6901=CIRCLE('',#17984,0.6);
#6902=CIRCLE('',#17987,0.6);
#6903=CIRCLE('',#17991,0.6);
#6904=CIRCLE('',#17993,0.9);
#6905=CIRCLE('',#17994,0.6);
#6906=CIRCLE('',#17996,0.9);
#6907=CIRCLE('',#17997,0.6);
#6908=CIRCLE('',#18000,0.6);
#6909=CIRCLE('',#18002,0.6);
#6910=CIRCLE('',#18007,0.605);
#6911=CIRCLE('',#18008,0.605);
#6912=CIRCLE('',#18010,0.9);
#6913=CIRCLE('',#18011,0.9);
#6914=CIRCLE('',#18016,0.605);
#6915=CIRCLE('',#18017,0.605);
#6916=CIRCLE('',#18019,0.9);
#6917=CIRCLE('',#18020,0.9);
#6918=CIRCLE('',#18025,0.21);
#6919=CIRCLE('',#18027,0.21);
#6920=CIRCLE('',#18028,0.21);
#6921=CIRCLE('',#18031,0.605);
#6922=CIRCLE('',#18032,0.605);
#6923=CIRCLE('',#18034,1.);
#6924=CIRCLE('',#18035,1.);
#6925=CIRCLE('',#18040,0.25);
#6926=CIRCLE('',#18041,0.25);
#6927=CIRCLE('',#18046,1.25);
#6928=CIRCLE('',#18047,0.6);
#6929=CIRCLE('',#18049,0.6);
#6930=CIRCLE('',#18051,1.);
#6931=CIRCLE('',#18052,1.);
#6932=CIRCLE('',#18054,1.25);
#6933=CIRCLE('',#18057,1.25);
#6934=CIRCLE('',#18060,1.25);
#6935=CIRCLE('',#18064,0.605);
#6936=CIRCLE('',#18065,0.605);
#6937=CIRCLE('',#18067,0.9);
#6938=CIRCLE('',#18068,0.9);
#6939=CIRCLE('',#18073,0.605);
#6940=CIRCLE('',#18074,0.605);
#6941=CIRCLE('',#18076,0.9);
#6942=CIRCLE('',#18077,0.9);
#6943=CIRCLE('',#18082,0.225);
#6944=CIRCLE('',#18083,0.225);
#6945=CIRCLE('',#18085,1.);
#6946=CIRCLE('',#18086,1.);
#6947=CIRCLE('',#18091,0.33);
#6948=CIRCLE('',#18092,0.33);
#6949=CIRCLE('',#18094,0.4);
#6950=CIRCLE('',#18095,0.4);
#6951=CIRCLE('',#18100,0.32);
#6952=CIRCLE('',#18101,0.32);
#6953=CIRCLE('',#18103,0.6);
#6954=CIRCLE('',#18104,0.6);
#6955=CIRCLE('',#18117,0.3);
#6956=CIRCLE('',#18118,0.2942);
#6957=CIRCLE('',#18120,0.3);
#6958=CIRCLE('',#18123,0.45);
#6959=CIRCLE('',#18125,0.5);
#6960=CIRCLE('',#18127,0.5);
#6961=CIRCLE('',#18129,0.47);
#6962=CIRCLE('',#18131,0.32);
#6963=CIRCLE('',#18133,0.2942);
#6964=CIRCLE('',#18138,0.165);
#6965=CIRCLE('',#18139,0.165);
#6966=CIRCLE('',#18143,1.);
#6967=CIRCLE('',#18147,1.);
#6968=CIRCLE('',#18149,1.3);
#6969=CIRCLE('',#18150,1.);
#6970=CIRCLE('',#18152,1.3);
#6971=CIRCLE('',#18153,1.);
#6972=CIRCLE('',#18156,1.);
#6973=CIRCLE('',#18158,1.);
#6974=CIRCLE('',#18163,1.005);
#6975=CIRCLE('',#18164,1.005);
#6976=CIRCLE('',#18166,1.3);
#6977=CIRCLE('',#18167,1.3);
#6978=CIRCLE('',#18172,1.005);
#6979=CIRCLE('',#18173,1.005);
#6980=CIRCLE('',#18175,1.3);
#6981=CIRCLE('',#18176,1.3);
#6982=CIRCLE('',#18181,0.21);
#6983=CIRCLE('',#18183,0.21);
#6984=CIRCLE('',#18184,0.21);
#6985=CIRCLE('',#18187,1.005);
#6986=CIRCLE('',#18188,1.005);
#6987=CIRCLE('',#18190,1.4);
#6988=CIRCLE('',#18191,1.4);
#6989=CIRCLE('',#18196,0.225);
#6990=CIRCLE('',#18197,0.225);
#6991=CIRCLE('',#18199,1.4);
#6992=CIRCLE('',#18200,1.4);
#6993=CIRCLE('',#18206,0.164999999999999);
#6994=CIRCLE('',#18207,0.164999999999999);
#6995=CIRCLE('',#18211,0.6);
#6996=CIRCLE('',#18215,0.6);
#6997=CIRCLE('',#18217,0.9);
#6998=CIRCLE('',#18218,0.6);
#6999=CIRCLE('',#18220,0.9);
#7000=CIRCLE('',#18221,0.6);
#7001=CIRCLE('',#18224,0.6);
#7002=CIRCLE('',#18226,0.6);
#7003=CIRCLE('',#18231,0.605);
#7004=CIRCLE('',#18232,0.605);
#7005=CIRCLE('',#18234,0.9);
#7006=CIRCLE('',#18235,0.9);
#7007=CIRCLE('',#18240,0.605);
#7008=CIRCLE('',#18241,0.605);
#7009=CIRCLE('',#18243,0.9);
#7010=CIRCLE('',#18244,0.9);
#7011=CIRCLE('',#18249,0.210000000000001);
#7012=CIRCLE('',#18251,0.210000000000001);
#7013=CIRCLE('',#18252,0.210000000000001);
#7014=CIRCLE('',#18255,0.605);
#7015=CIRCLE('',#18256,0.605);
#7016=CIRCLE('',#18258,1.);
#7017=CIRCLE('',#18259,1.);
#7018=CIRCLE('',#18264,0.225);
#7019=CIRCLE('',#18265,0.225);
#7020=CIRCLE('',#18267,1.);
#7021=CIRCLE('',#18268,1.);
#7022=CIRCLE('',#18276,1.75);
#7023=CIRCLE('',#18277,1.75);
#7024=CIRCLE('',#18278,1.75);
#7025=CIRCLE('',#18279,1.75);
#7026=CIRCLE('',#18280,1.75);
#7027=CIRCLE('',#18281,1.75);
#7028=CIRCLE('',#18282,1.75);
#7029=CIRCLE('',#18283,1.75);
#7030=CIRCLE('',#18284,1.75);
#7031=CIRCLE('',#18285,1.75);
#7032=CIRCLE('',#18286,1.75);
#7033=CIRCLE('',#18287,1.75);
#7034=CIRCLE('',#18288,1.75);
#7035=CIRCLE('',#18289,1.75);
#7036=CIRCLE('',#18290,1.75);
#7037=CIRCLE('',#18291,1.75);
#7038=CIRCLE('',#18292,1.75);
#7039=CIRCLE('',#18293,1.75);
#7040=CIRCLE('',#18294,1.75);
#7041=CIRCLE('',#18295,1.75);
#7042=CIRCLE('',#18296,0.6);
#7043=CIRCLE('',#18298,0.6);
#7044=CIRCLE('',#18300,1.4);
#7045=CIRCLE('',#18301,1.4);
#7046=CIRCLE('',#18305,1.75);
#7047=CIRCLE('',#18308,1.75);
#7048=CIRCLE('',#18311,1.75);
#7049=CIRCLE('',#18314,1.75);
#7050=CIRCLE('',#18317,1.75);
#7051=CIRCLE('',#18320,1.75);
#7052=CIRCLE('',#18323,1.75);
#7053=CIRCLE('',#18326,1.75);
#7054=CIRCLE('',#18329,1.75);
#7055=CIRCLE('',#18332,1.75);
#7056=CIRCLE('',#18335,1.75);
#7057=CIRCLE('',#18338,1.75);
#7058=CIRCLE('',#18341,1.75);
#7059=CIRCLE('',#18344,1.75);
#7060=CIRCLE('',#18347,1.75);
#7061=CIRCLE('',#18350,1.75);
#7062=CIRCLE('',#18353,1.75);
#7063=CIRCLE('',#18356,1.75);
#7064=CIRCLE('',#18359,1.75);
#7065=CIRCLE('',#18362,1.75);
#7066=CIRCLE('',#18378,0.164999999999999);
#7067=CIRCLE('',#18379,0.164999999999999);
#7068=CIRCLE('',#18383,1.);
#7069=CIRCLE('',#18387,1.);
#7070=CIRCLE('',#18389,1.3);
#7071=CIRCLE('',#18390,1.);
#7072=CIRCLE('',#18392,1.3);
#7073=CIRCLE('',#18393,1.);
#7074=CIRCLE('',#18396,1.);
#7075=CIRCLE('',#18398,1.);
#7076=CIRCLE('',#18403,1.005);
#7077=CIRCLE('',#18404,1.005);
#7078=CIRCLE('',#18406,1.3);
#7079=CIRCLE('',#18407,1.3);
#7080=CIRCLE('',#18412,1.005);
#7081=CIRCLE('',#18413,1.005);
#7082=CIRCLE('',#18415,1.3);
#7083=CIRCLE('',#18416,1.3);
#7084=CIRCLE('',#18421,0.210000000000001);
#7085=CIRCLE('',#18423,0.210000000000001);
#7086=CIRCLE('',#18424,0.210000000000001);
#7087=CIRCLE('',#18427,1.005);
#7088=CIRCLE('',#18428,1.005);
#7089=CIRCLE('',#18430,1.4);
#7090=CIRCLE('',#18431,1.4);
#7091=CIRCLE('',#18436,1.005);
#7092=CIRCLE('',#18437,1.005);
#7093=CIRCLE('',#18439,1.4);
#7094=CIRCLE('',#18440,1.4);
#7095=CIRCLE('',#18445,1.005);
#7096=CIRCLE('',#18446,1.005);
#7097=CIRCLE('',#18448,1.4);
#7098=CIRCLE('',#18449,1.4);
#7099=CIRCLE('',#18454,0.210000000000001);
#7100=CIRCLE('',#18456,0.210000000000001);
#7101=CIRCLE('',#18457,0.210000000000001);
#7102=CIRCLE('',#18461,1.5);
#7103=CIRCLE('',#18463,1.5);
#7104=CIRCLE('',#18466,1.);
#7105=CIRCLE('',#18467,1.);
#7106=CIRCLE('',#18469,1.5);
#7107=CIRCLE('',#18470,1.5);
#7108=CIRCLE('',#18475,0.225000000000001);
#7109=CIRCLE('',#18476,0.225000000000001);
#7110=CIRCLE('',#18478,1.4);
#7111=CIRCLE('',#18479,1.4);
#7112=CIRCLE('',#18487,3.75);
#7113=CIRCLE('',#18488,3.75);
#7114=CIRCLE('',#18489,3.75);
#7115=CIRCLE('',#18490,3.75);
#7116=CIRCLE('',#18491,3.75);
#7117=CIRCLE('',#18492,3.75);
#7118=CIRCLE('',#18493,3.75);
#7119=CIRCLE('',#18494,3.75);
#7120=CIRCLE('',#18495,3.75);
#7121=CIRCLE('',#18496,3.75);
#7122=CIRCLE('',#18497,3.75);
#7123=CIRCLE('',#18498,3.75);
#7124=CIRCLE('',#18499,3.75);
#7125=CIRCLE('',#18500,3.75);
#7126=CIRCLE('',#18501,3.75);
#7127=CIRCLE('',#18502,3.75);
#7128=CIRCLE('',#18503,3.75);
#7129=CIRCLE('',#18504,3.75);
#7130=CIRCLE('',#18505,3.75);
#7131=CIRCLE('',#18506,3.75);
#7132=CIRCLE('',#18507,3.75);
#7133=CIRCLE('',#18508,3.75);
#7134=CIRCLE('',#18509,3.75);
#7135=CIRCLE('',#18510,3.75);
#7136=CIRCLE('',#18511,3.75);
#7137=CIRCLE('',#18512,3.75);
#7138=CIRCLE('',#18513,3.75);
#7139=CIRCLE('',#18514,3.75);
#7140=CIRCLE('',#18515,3.75);
#7141=CIRCLE('',#18516,3.75);
#7142=CIRCLE('',#18517,3.75);
#7143=CIRCLE('',#18518,3.75);
#7144=CIRCLE('',#18519,3.75);
#7145=CIRCLE('',#18520,3.75);
#7146=CIRCLE('',#18521,3.75);
#7147=CIRCLE('',#18522,3.75);
#7148=CIRCLE('',#18523,3.75);
#7149=CIRCLE('',#18524,3.75);
#7150=CIRCLE('',#18525,3.75);
#7151=CIRCLE('',#18526,3.75);
#7152=CIRCLE('',#18527,1.);
#7153=CIRCLE('',#18529,1.);
#7154=CIRCLE('',#18531,2.);
#7155=CIRCLE('',#18532,2.);
#7156=CIRCLE('',#18536,3.75);
#7157=CIRCLE('',#18539,3.75);
#7158=CIRCLE('',#18542,3.75);
#7159=CIRCLE('',#18545,3.75);
#7160=CIRCLE('',#18548,3.75);
#7161=CIRCLE('',#18551,3.75);
#7162=CIRCLE('',#18554,3.75);
#7163=CIRCLE('',#18557,3.75);
#7164=CIRCLE('',#18560,3.75);
#7165=CIRCLE('',#18563,3.75);
#7166=CIRCLE('',#18566,3.75);
#7167=CIRCLE('',#18569,3.75);
#7168=CIRCLE('',#18572,3.75);
#7169=CIRCLE('',#18575,3.75);
#7170=CIRCLE('',#18578,3.75);
#7171=CIRCLE('',#18581,3.75);
#7172=CIRCLE('',#18584,3.75);
#7173=CIRCLE('',#18587,3.75);
#7174=CIRCLE('',#18590,3.75);
#7175=CIRCLE('',#18593,3.75);
#7176=CIRCLE('',#18596,3.75);
#7177=CIRCLE('',#18599,3.75);
#7178=CIRCLE('',#18602,3.75);
#7179=CIRCLE('',#18605,3.75);
#7180=CIRCLE('',#18608,3.75);
#7181=CIRCLE('',#18611,3.75);
#7182=CIRCLE('',#18614,3.75);
#7183=CIRCLE('',#18617,3.75);
#7184=CIRCLE('',#18620,3.75);
#7185=CIRCLE('',#18623,3.75);
#7186=CIRCLE('',#18626,3.75);
#7187=CIRCLE('',#18629,3.75);
#7188=CIRCLE('',#18632,3.75);
#7189=CIRCLE('',#18635,3.75);
#7190=CIRCLE('',#18638,3.75);
#7191=CIRCLE('',#18641,3.75);
#7192=CIRCLE('',#18644,3.75);
#7193=CIRCLE('',#18647,3.75);
#7194=CIRCLE('',#18650,3.75);
#7195=CIRCLE('',#18653,3.75);
#7196=CIRCLE('',#18675,0.22);
#7197=CIRCLE('',#18677,0.24505);
#7198=CIRCLE('',#18679,0.24505);
#7199=CIRCLE('',#18681,0.175);
#7200=CIRCLE('',#18685,0.3);
#7201=CIRCLE('',#18687,0.35);
#7202=CIRCLE('',#18689,0.35);
#7203=CIRCLE('',#18691,0.32);
#7204=CIRCLE('',#18693,0.22);
#7205=CIRCLE('',#18695,0.1954);
#7206=CIRCLE('',#18697,0.1954);
#7207=CIRCLE('',#18699,0.16);
#7208=CIRCLE('',#18817,0.405);
#7209=CIRCLE('',#18818,0.405);
#7210=CIRCLE('',#18820,0.9);
#7211=CIRCLE('',#18821,0.9);
#7212=VERTEX_POINT('',#23313);
#7213=VERTEX_POINT('',#23315);
#7214=VERTEX_POINT('',#23319);
#7215=VERTEX_POINT('',#23321);
#7216=VERTEX_POINT('',#23325);
#7217=VERTEX_POINT('',#23327);
#7218=VERTEX_POINT('',#23331);
#7219=VERTEX_POINT('',#23332);
#7220=VERTEX_POINT('',#23334);
#7221=VERTEX_POINT('',#23336);
#7222=VERTEX_POINT('',#23340);
#7223=VERTEX_POINT('',#23342);
#7224=VERTEX_POINT('',#23346);
#7225=VERTEX_POINT('',#23348);
#7226=VERTEX_POINT('',#23358);
#7227=VERTEX_POINT('',#23360);
#7228=VERTEX_POINT('',#23364);
#7229=VERTEX_POINT('',#23366);
#7230=VERTEX_POINT('',#23370);
#7231=VERTEX_POINT('',#23372);
#7232=VERTEX_POINT('',#23376);
#7233=VERTEX_POINT('',#23378);
#7234=VERTEX_POINT('',#23382);
#7235=VERTEX_POINT('',#23384);
#7236=VERTEX_POINT('',#23388);
#7237=VERTEX_POINT('',#23390);
#7238=VERTEX_POINT('',#23394);
#7239=VERTEX_POINT('',#23396);
#7240=VERTEX_POINT('',#23400);
#7241=VERTEX_POINT('',#23402);
#7242=VERTEX_POINT('',#23406);
#7243=VERTEX_POINT('',#23408);
#7244=VERTEX_POINT('',#23412);
#7245=VERTEX_POINT('',#23414);
#7246=VERTEX_POINT('',#23418);
#7247=VERTEX_POINT('',#23420);
#7248=VERTEX_POINT('',#23424);
#7249=VERTEX_POINT('',#23426);
#7250=VERTEX_POINT('',#23430);
#7251=VERTEX_POINT('',#23432);
#7252=VERTEX_POINT('',#23436);
#7253=VERTEX_POINT('',#23438);
#7254=VERTEX_POINT('',#23442);
#7255=VERTEX_POINT('',#23444);
#7256=VERTEX_POINT('',#23448);
#7257=VERTEX_POINT('',#23450);
#7258=VERTEX_POINT('',#23454);
#7259=VERTEX_POINT('',#23456);
#7260=VERTEX_POINT('',#23460);
#7261=VERTEX_POINT('',#23462);
#7262=VERTEX_POINT('',#23466);
#7263=VERTEX_POINT('',#23468);
#7264=VERTEX_POINT('',#23472);
#7265=VERTEX_POINT('',#23474);
#7266=VERTEX_POINT('',#23478);
#7267=VERTEX_POINT('',#23480);
#7268=VERTEX_POINT('',#23484);
#7269=VERTEX_POINT('',#23486);
#7270=VERTEX_POINT('',#23490);
#7271=VERTEX_POINT('',#23492);
#7272=VERTEX_POINT('',#23496);
#7273=VERTEX_POINT('',#23498);
#7274=VERTEX_POINT('',#23502);
#7275=VERTEX_POINT('',#23504);
#7276=VERTEX_POINT('',#23508);
#7277=VERTEX_POINT('',#23509);
#7278=VERTEX_POINT('',#23511);
#7279=VERTEX_POINT('',#23513);
#7280=VERTEX_POINT('',#23517);
#7281=VERTEX_POINT('',#23519);
#7282=VERTEX_POINT('',#23523);
#7283=VERTEX_POINT('',#23524);
#7284=VERTEX_POINT('',#23526);
#7285=VERTEX_POINT('',#23528);
#7286=VERTEX_POINT('',#23533);
#7287=VERTEX_POINT('',#23537);
#7288=VERTEX_POINT('',#23547);
#7289=VERTEX_POINT('',#23549);
#7290=VERTEX_POINT('',#23553);
#7291=VERTEX_POINT('',#23555);
#7292=VERTEX_POINT('',#23559);
#7293=VERTEX_POINT('',#23561);
#7294=VERTEX_POINT('',#23565);
#7295=VERTEX_POINT('',#23567);
#7296=VERTEX_POINT('',#23571);
#7297=VERTEX_POINT('',#23573);
#7298=VERTEX_POINT('',#23577);
#7299=VERTEX_POINT('',#23580);
#7300=VERTEX_POINT('',#23584);
#7301=VERTEX_POINT('',#23586);
#7302=VERTEX_POINT('',#23593);
#7303=VERTEX_POINT('',#23595);
#7304=VERTEX_POINT('',#23599);
#7305=VERTEX_POINT('',#23601);
#7306=VERTEX_POINT('',#23605);
#7307=VERTEX_POINT('',#23607);
#7308=VERTEX_POINT('',#23611);
#7309=VERTEX_POINT('',#23613);
#7310=VERTEX_POINT('',#23617);
#7311=VERTEX_POINT('',#23619);
#7312=VERTEX_POINT('',#23623);
#7313=VERTEX_POINT('',#23626);
#7314=VERTEX_POINT('',#23630);
#7315=VERTEX_POINT('',#23632);
#7316=VERTEX_POINT('',#23639);
#7317=VERTEX_POINT('',#23641);
#7318=VERTEX_POINT('',#23645);
#7319=VERTEX_POINT('',#23647);
#7320=VERTEX_POINT('',#23651);
#7321=VERTEX_POINT('',#23653);
#7322=VERTEX_POINT('',#23657);
#7323=VERTEX_POINT('',#23659);
#7324=VERTEX_POINT('',#23663);
#7325=VERTEX_POINT('',#23665);
#7326=VERTEX_POINT('',#23669);
#7327=VERTEX_POINT('',#23672);
#7328=VERTEX_POINT('',#23676);
#7329=VERTEX_POINT('',#23678);
#7330=VERTEX_POINT('',#23685);
#7331=VERTEX_POINT('',#23687);
#7332=VERTEX_POINT('',#23691);
#7333=VERTEX_POINT('',#23693);
#7334=VERTEX_POINT('',#23697);
#7335=VERTEX_POINT('',#23699);
#7336=VERTEX_POINT('',#23703);
#7337=VERTEX_POINT('',#23705);
#7338=VERTEX_POINT('',#23709);
#7339=VERTEX_POINT('',#23711);
#7340=VERTEX_POINT('',#23715);
#7341=VERTEX_POINT('',#23718);
#7342=VERTEX_POINT('',#23722);
#7343=VERTEX_POINT('',#23724);
#7344=VERTEX_POINT('',#23731);
#7345=VERTEX_POINT('',#23732);
#7346=VERTEX_POINT('',#23734);
#7347=VERTEX_POINT('',#23736);
#7348=VERTEX_POINT('',#23740);
#7349=VERTEX_POINT('',#23742);
#7350=VERTEX_POINT('',#23746);
#7351=VERTEX_POINT('',#23748);
#7352=VERTEX_POINT('',#23752);
#7353=VERTEX_POINT('',#23754);
#7354=VERTEX_POINT('',#23758);
#7355=VERTEX_POINT('',#23760);
#7356=VERTEX_POINT('',#23769);
#7357=VERTEX_POINT('',#23772);
#7358=VERTEX_POINT('',#23775);
#7359=VERTEX_POINT('',#23779);
#7360=VERTEX_POINT('',#23783);
#7361=VERTEX_POINT('',#23787);
#7362=VERTEX_POINT('',#23790);
#7363=VERTEX_POINT('',#23797);
#7364=VERTEX_POINT('',#23799);
#7365=VERTEX_POINT('',#23803);
#7366=VERTEX_POINT('',#23805);
#7367=VERTEX_POINT('',#23809);
#7368=VERTEX_POINT('',#23811);
#7369=VERTEX_POINT('',#23815);
#7370=VERTEX_POINT('',#23817);
#7371=VERTEX_POINT('',#23821);
#7372=VERTEX_POINT('',#23823);
#7373=VERTEX_POINT('',#23827);
#7374=VERTEX_POINT('',#23830);
#7375=VERTEX_POINT('',#23834);
#7376=VERTEX_POINT('',#23836);
#7377=VERTEX_POINT('',#23843);
#7378=VERTEX_POINT('',#23845);
#7379=VERTEX_POINT('',#23849);
#7380=VERTEX_POINT('',#23851);
#7381=VERTEX_POINT('',#23855);
#7382=VERTEX_POINT('',#23857);
#7383=VERTEX_POINT('',#23861);
#7384=VERTEX_POINT('',#23863);
#7385=VERTEX_POINT('',#23867);
#7386=VERTEX_POINT('',#23869);
#7387=VERTEX_POINT('',#23873);
#7388=VERTEX_POINT('',#23876);
#7389=VERTEX_POINT('',#23880);
#7390=VERTEX_POINT('',#23882);
#7391=VERTEX_POINT('',#23889);
#7392=VERTEX_POINT('',#23891);
#7393=VERTEX_POINT('',#23895);
#7394=VERTEX_POINT('',#23897);
#7395=VERTEX_POINT('',#23901);
#7396=VERTEX_POINT('',#23903);
#7397=VERTEX_POINT('',#23907);
#7398=VERTEX_POINT('',#23909);
#7399=VERTEX_POINT('',#23913);
#7400=VERTEX_POINT('',#23915);
#7401=VERTEX_POINT('',#23919);
#7402=VERTEX_POINT('',#23922);
#7403=VERTEX_POINT('',#23926);
#7404=VERTEX_POINT('',#23928);
#7405=VERTEX_POINT('',#23935);
#7406=VERTEX_POINT('',#23937);
#7407=VERTEX_POINT('',#23941);
#7408=VERTEX_POINT('',#23943);
#7409=VERTEX_POINT('',#23947);
#7410=VERTEX_POINT('',#23949);
#7411=VERTEX_POINT('',#23953);
#7412=VERTEX_POINT('',#23955);
#7413=VERTEX_POINT('',#23959);
#7414=VERTEX_POINT('',#23961);
#7415=VERTEX_POINT('',#23965);
#7416=VERTEX_POINT('',#23968);
#7417=VERTEX_POINT('',#23972);
#7418=VERTEX_POINT('',#23974);
#7419=VERTEX_POINT('',#23982);
#7420=VERTEX_POINT('',#23983);
#7421=VERTEX_POINT('',#23986);
#7422=VERTEX_POINT('',#23988);
#7423=VERTEX_POINT('',#23992);
#7424=VERTEX_POINT('',#23996);
#7425=VERTEX_POINT('',#23998);
#7426=VERTEX_POINT('',#24002);
#7427=VERTEX_POINT('',#24007);
#7428=VERTEX_POINT('',#24011);
#7429=VERTEX_POINT('',#24017);
#7430=VERTEX_POINT('',#24018);
#7431=VERTEX_POINT('',#24021);
#7432=VERTEX_POINT('',#24023);
#7433=VERTEX_POINT('',#24027);
#7434=VERTEX_POINT('',#24031);
#7435=VERTEX_POINT('',#24033);
#7436=VERTEX_POINT('',#24036);
#7437=VERTEX_POINT('',#24040);
#7438=VERTEX_POINT('',#24044);
#7439=VERTEX_POINT('',#24052);
#7440=VERTEX_POINT('',#24053);
#7441=VERTEX_POINT('',#24056);
#7442=VERTEX_POINT('',#24057);
#7443=VERTEX_POINT('',#24060);
#7444=VERTEX_POINT('',#24061);
#7445=VERTEX_POINT('',#24064);
#7446=VERTEX_POINT('',#24065);
#7447=VERTEX_POINT('',#24068);
#7448=VERTEX_POINT('',#24069);
#7449=VERTEX_POINT('',#24072);
#7450=VERTEX_POINT('',#24073);
#7451=VERTEX_POINT('',#24076);
#7452=VERTEX_POINT('',#24077);
#7453=VERTEX_POINT('',#24081);
#7454=VERTEX_POINT('',#24082);
#7455=VERTEX_POINT('',#24105);
#7456=VERTEX_POINT('',#24107);
#7457=VERTEX_POINT('',#24132);
#7458=VERTEX_POINT('',#24134);
#7459=VERTEX_POINT('',#24157);
#7460=VERTEX_POINT('',#24159);
#7461=VERTEX_POINT('',#24182);
#7462=VERTEX_POINT('',#24184);
#7463=VERTEX_POINT('',#24187);
#7464=VERTEX_POINT('',#24189);
#7465=VERTEX_POINT('',#24212);
#7466=VERTEX_POINT('',#24214);
#7467=VERTEX_POINT('',#24237);
#7468=VERTEX_POINT('',#24239);
#7469=VERTEX_POINT('',#24262);
#7470=VERTEX_POINT('',#24264);
#7471=VERTEX_POINT('',#24289);
#7472=VERTEX_POINT('',#24293);
#7473=VERTEX_POINT('',#24318);
#7474=VERTEX_POINT('',#24322);
#7475=VERTEX_POINT('',#24347);
#7476=VERTEX_POINT('',#24349);
#7477=VERTEX_POINT('',#24353);
#7478=VERTEX_POINT('',#24378);
#7479=VERTEX_POINT('',#24382);
#7480=VERTEX_POINT('',#24407);
#7481=VERTEX_POINT('',#24411);
#7482=VERTEX_POINT('',#24436);
#7483=VERTEX_POINT('',#24439);
#7484=VERTEX_POINT('',#24441);
#7485=VERTEX_POINT('',#24473);
#7486=VERTEX_POINT('',#24475);
#7487=VERTEX_POINT('',#24478);
#7488=VERTEX_POINT('',#24482);
#7489=VERTEX_POINT('',#24487);
#7490=VERTEX_POINT('',#24489);
#7491=VERTEX_POINT('',#24492);
#7492=VERTEX_POINT('',#24496);
#7493=VERTEX_POINT('',#24508);
#7494=VERTEX_POINT('',#24509);
#7495=VERTEX_POINT('',#24512);
#7496=VERTEX_POINT('',#24514);
#7497=VERTEX_POINT('',#24518);
#7498=VERTEX_POINT('',#24522);
#7499=VERTEX_POINT('',#24524);
#7500=VERTEX_POINT('',#24528);
#7501=VERTEX_POINT('',#24533);
#7502=VERTEX_POINT('',#24537);
#7503=VERTEX_POINT('',#24543);
#7504=VERTEX_POINT('',#24544);
#7505=VERTEX_POINT('',#24547);
#7506=VERTEX_POINT('',#24549);
#7507=VERTEX_POINT('',#24553);
#7508=VERTEX_POINT('',#24557);
#7509=VERTEX_POINT('',#24559);
#7510=VERTEX_POINT('',#24562);
#7511=VERTEX_POINT('',#24566);
#7512=VERTEX_POINT('',#24570);
#7513=VERTEX_POINT('',#24578);
#7514=VERTEX_POINT('',#24579);
#7515=VERTEX_POINT('',#24582);
#7516=VERTEX_POINT('',#24583);
#7517=VERTEX_POINT('',#24586);
#7518=VERTEX_POINT('',#24587);
#7519=VERTEX_POINT('',#24590);
#7520=VERTEX_POINT('',#24591);
#7521=VERTEX_POINT('',#24594);
#7522=VERTEX_POINT('',#24595);
#7523=VERTEX_POINT('',#24598);
#7524=VERTEX_POINT('',#24599);
#7525=VERTEX_POINT('',#24602);
#7526=VERTEX_POINT('',#24603);
#7527=VERTEX_POINT('',#24606);
#7528=VERTEX_POINT('',#24607);
#7529=VERTEX_POINT('',#24611);
#7530=VERTEX_POINT('',#24612);
#7531=VERTEX_POINT('',#24635);
#7532=VERTEX_POINT('',#24637);
#7533=VERTEX_POINT('',#24662);
#7534=VERTEX_POINT('',#24664);
#7535=VERTEX_POINT('',#24687);
#7536=VERTEX_POINT('',#24689);
#7537=VERTEX_POINT('',#24712);
#7538=VERTEX_POINT('',#24714);
#7539=VERTEX_POINT('',#24727);
#7540=VERTEX_POINT('',#24730);
#7541=VERTEX_POINT('',#24743);
#7542=VERTEX_POINT('',#24745);
#7543=VERTEX_POINT('',#24768);
#7544=VERTEX_POINT('',#24770);
#7545=VERTEX_POINT('',#24793);
#7546=VERTEX_POINT('',#24795);
#7547=VERTEX_POINT('',#24818);
#7548=VERTEX_POINT('',#24820);
#7549=VERTEX_POINT('',#24845);
#7550=VERTEX_POINT('',#24849);
#7551=VERTEX_POINT('',#24874);
#7552=VERTEX_POINT('',#24878);
#7553=VERTEX_POINT('',#24903);
#7554=VERTEX_POINT('',#24907);
#7555=VERTEX_POINT('',#24908);
#7556=VERTEX_POINT('',#24935);
#7557=VERTEX_POINT('',#24939);
#7558=VERTEX_POINT('',#24964);
#7559=VERTEX_POINT('',#24968);
#7560=VERTEX_POINT('',#24993);
#7561=VERTEX_POINT('',#24997);
#7562=VERTEX_POINT('',#25022);
#7563=VERTEX_POINT('',#25025);
#7564=VERTEX_POINT('',#25027);
#7565=VERTEX_POINT('',#25059);
#7566=VERTEX_POINT('',#25061);
#7567=VERTEX_POINT('',#25064);
#7568=VERTEX_POINT('',#25068);
#7569=VERTEX_POINT('',#25073);
#7570=VERTEX_POINT('',#25075);
#7571=VERTEX_POINT('',#25078);
#7572=VERTEX_POINT('',#25082);
#7573=VERTEX_POINT('',#25093);
#7574=VERTEX_POINT('',#25094);
#7575=VERTEX_POINT('',#25096);
#7576=VERTEX_POINT('',#25098);
#7577=VERTEX_POINT('',#25102);
#7578=VERTEX_POINT('',#25104);
#7579=VERTEX_POINT('',#25108);
#7580=VERTEX_POINT('',#25110);
#7581=VERTEX_POINT('',#25114);
#7582=VERTEX_POINT('',#25116);
#7583=VERTEX_POINT('',#25120);
#7584=VERTEX_POINT('',#25122);
#7585=VERTEX_POINT('',#25131);
#7586=VERTEX_POINT('',#25134);
#7587=VERTEX_POINT('',#25137);
#7588=VERTEX_POINT('',#25141);
#7589=VERTEX_POINT('',#25145);
#7590=VERTEX_POINT('',#25149);
#7591=VERTEX_POINT('',#25152);
#7592=VERTEX_POINT('',#25159);
#7593=VERTEX_POINT('',#25160);
#7594=VERTEX_POINT('',#25162);
#7595=VERTEX_POINT('',#25164);
#7596=VERTEX_POINT('',#25168);
#7597=VERTEX_POINT('',#25170);
#7598=VERTEX_POINT('',#25174);
#7599=VERTEX_POINT('',#25176);
#7600=VERTEX_POINT('',#25184);
#7601=VERTEX_POINT('',#25185);
#7602=VERTEX_POINT('',#25187);
#7603=VERTEX_POINT('',#25189);
#7604=VERTEX_POINT('',#25193);
#7605=VERTEX_POINT('',#25195);
#7606=VERTEX_POINT('',#25199);
#7607=VERTEX_POINT('',#25201);
#7608=VERTEX_POINT('',#25209);
#7609=VERTEX_POINT('',#25210);
#7610=VERTEX_POINT('',#25212);
#7611=VERTEX_POINT('',#25214);
#7612=VERTEX_POINT('',#25218);
#7613=VERTEX_POINT('',#25220);
#7614=VERTEX_POINT('',#25224);
#7615=VERTEX_POINT('',#25226);
#7616=VERTEX_POINT('',#25234);
#7617=VERTEX_POINT('',#25235);
#7618=VERTEX_POINT('',#25237);
#7619=VERTEX_POINT('',#25239);
#7620=VERTEX_POINT('',#25243);
#7621=VERTEX_POINT('',#25245);
#7622=VERTEX_POINT('',#25249);
#7623=VERTEX_POINT('',#25251);
#7624=VERTEX_POINT('',#25259);
#7625=VERTEX_POINT('',#25260);
#7626=VERTEX_POINT('',#25262);
#7627=VERTEX_POINT('',#25264);
#7628=VERTEX_POINT('',#25268);
#7629=VERTEX_POINT('',#25270);
#7630=VERTEX_POINT('',#25274);
#7631=VERTEX_POINT('',#25276);
#7632=VERTEX_POINT('',#25284);
#7633=VERTEX_POINT('',#25285);
#7634=VERTEX_POINT('',#25287);
#7635=VERTEX_POINT('',#25289);
#7636=VERTEX_POINT('',#25293);
#7637=VERTEX_POINT('',#25295);
#7638=VERTEX_POINT('',#25299);
#7639=VERTEX_POINT('',#25301);
#7640=VERTEX_POINT('',#25309);
#7641=VERTEX_POINT('',#25310);
#7642=VERTEX_POINT('',#25312);
#7643=VERTEX_POINT('',#25314);
#7644=VERTEX_POINT('',#25318);
#7645=VERTEX_POINT('',#25320);
#7646=VERTEX_POINT('',#25324);
#7647=VERTEX_POINT('',#25326);
#7648=VERTEX_POINT('',#25334);
#7649=VERTEX_POINT('',#25335);
#7650=VERTEX_POINT('',#25337);
#7651=VERTEX_POINT('',#25339);
#7652=VERTEX_POINT('',#25343);
#7653=VERTEX_POINT('',#25345);
#7654=VERTEX_POINT('',#25349);
#7655=VERTEX_POINT('',#25351);
#7656=VERTEX_POINT('',#25359);
#7657=VERTEX_POINT('',#25360);
#7658=VERTEX_POINT('',#25362);
#7659=VERTEX_POINT('',#25364);
#7660=VERTEX_POINT('',#25368);
#7661=VERTEX_POINT('',#25370);
#7662=VERTEX_POINT('',#25374);
#7663=VERTEX_POINT('',#25376);
#7664=VERTEX_POINT('',#25384);
#7665=VERTEX_POINT('',#25385);
#7666=VERTEX_POINT('',#25387);
#7667=VERTEX_POINT('',#25389);
#7668=VERTEX_POINT('',#25393);
#7669=VERTEX_POINT('',#25395);
#7670=VERTEX_POINT('',#25399);
#7671=VERTEX_POINT('',#25401);
#7672=VERTEX_POINT('',#25409);
#7673=VERTEX_POINT('',#25410);
#7674=VERTEX_POINT('',#25412);
#7675=VERTEX_POINT('',#25414);
#7676=VERTEX_POINT('',#25418);
#7677=VERTEX_POINT('',#25420);
#7678=VERTEX_POINT('',#25424);
#7679=VERTEX_POINT('',#25426);
#7680=VERTEX_POINT('',#25434);
#7681=VERTEX_POINT('',#25435);
#7682=VERTEX_POINT('',#25437);
#7683=VERTEX_POINT('',#25439);
#7684=VERTEX_POINT('',#25443);
#7685=VERTEX_POINT('',#25445);
#7686=VERTEX_POINT('',#25449);
#7687=VERTEX_POINT('',#25451);
#7688=VERTEX_POINT('',#25459);
#7689=VERTEX_POINT('',#25460);
#7690=VERTEX_POINT('',#25462);
#7691=VERTEX_POINT('',#25464);
#7692=VERTEX_POINT('',#25468);
#7693=VERTEX_POINT('',#25470);
#7694=VERTEX_POINT('',#25474);
#7695=VERTEX_POINT('',#25476);
#7696=VERTEX_POINT('',#25484);
#7697=VERTEX_POINT('',#25485);
#7698=VERTEX_POINT('',#25487);
#7699=VERTEX_POINT('',#25489);
#7700=VERTEX_POINT('',#25493);
#7701=VERTEX_POINT('',#25495);
#7702=VERTEX_POINT('',#25499);
#7703=VERTEX_POINT('',#25501);
#7704=VERTEX_POINT('',#25509);
#7705=VERTEX_POINT('',#25510);
#7706=VERTEX_POINT('',#25512);
#7707=VERTEX_POINT('',#25514);
#7708=VERTEX_POINT('',#25518);
#7709=VERTEX_POINT('',#25520);
#7710=VERTEX_POINT('',#25524);
#7711=VERTEX_POINT('',#25526);
#7712=VERTEX_POINT('',#25534);
#7713=VERTEX_POINT('',#25535);
#7714=VERTEX_POINT('',#25537);
#7715=VERTEX_POINT('',#25539);
#7716=VERTEX_POINT('',#25543);
#7717=VERTEX_POINT('',#25545);
#7718=VERTEX_POINT('',#25549);
#7719=VERTEX_POINT('',#25551);
#7720=VERTEX_POINT('',#25559);
#7721=VERTEX_POINT('',#25560);
#7722=VERTEX_POINT('',#25562);
#7723=VERTEX_POINT('',#25564);
#7724=VERTEX_POINT('',#25568);
#7725=VERTEX_POINT('',#25570);
#7726=VERTEX_POINT('',#25574);
#7727=VERTEX_POINT('',#25576);
#7728=VERTEX_POINT('',#25584);
#7729=VERTEX_POINT('',#25585);
#7730=VERTEX_POINT('',#25587);
#7731=VERTEX_POINT('',#25589);
#7732=VERTEX_POINT('',#25593);
#7733=VERTEX_POINT('',#25595);
#7734=VERTEX_POINT('',#25599);
#7735=VERTEX_POINT('',#25601);
#7736=VERTEX_POINT('',#25609);
#7737=VERTEX_POINT('',#25610);
#7738=VERTEX_POINT('',#25612);
#7739=VERTEX_POINT('',#25614);
#7740=VERTEX_POINT('',#25618);
#7741=VERTEX_POINT('',#25620);
#7742=VERTEX_POINT('',#25624);
#7743=VERTEX_POINT('',#25626);
#7744=VERTEX_POINT('',#25634);
#7745=VERTEX_POINT('',#25635);
#7746=VERTEX_POINT('',#25637);
#7747=VERTEX_POINT('',#25639);
#7748=VERTEX_POINT('',#25643);
#7749=VERTEX_POINT('',#25645);
#7750=VERTEX_POINT('',#25649);
#7751=VERTEX_POINT('',#25651);
#7752=VERTEX_POINT('',#25659);
#7753=VERTEX_POINT('',#25660);
#7754=VERTEX_POINT('',#25662);
#7755=VERTEX_POINT('',#25664);
#7756=VERTEX_POINT('',#25668);
#7757=VERTEX_POINT('',#25670);
#7758=VERTEX_POINT('',#25674);
#7759=VERTEX_POINT('',#25676);
#7760=VERTEX_POINT('',#25684);
#7761=VERTEX_POINT('',#25685);
#7762=VERTEX_POINT('',#25687);
#7763=VERTEX_POINT('',#25689);
#7764=VERTEX_POINT('',#25693);
#7765=VERTEX_POINT('',#25695);
#7766=VERTEX_POINT('',#25699);
#7767=VERTEX_POINT('',#25701);
#7768=VERTEX_POINT('',#25709);
#7769=VERTEX_POINT('',#25710);
#7770=VERTEX_POINT('',#25712);
#7771=VERTEX_POINT('',#25714);
#7772=VERTEX_POINT('',#25718);
#7773=VERTEX_POINT('',#25720);
#7774=VERTEX_POINT('',#25724);
#7775=VERTEX_POINT('',#25726);
#7776=VERTEX_POINT('',#25734);
#7777=VERTEX_POINT('',#25735);
#7778=VERTEX_POINT('',#25737);
#7779=VERTEX_POINT('',#25739);
#7780=VERTEX_POINT('',#25743);
#7781=VERTEX_POINT('',#25745);
#7782=VERTEX_POINT('',#25749);
#7783=VERTEX_POINT('',#25751);
#7784=VERTEX_POINT('',#25759);
#7785=VERTEX_POINT('',#25761);
#7786=VERTEX_POINT('',#25765);
#7787=VERTEX_POINT('',#25767);
#7788=VERTEX_POINT('',#25771);
#7789=VERTEX_POINT('',#25773);
#7790=VERTEX_POINT('',#25777);
#7791=VERTEX_POINT('',#25778);
#7792=VERTEX_POINT('',#25780);
#7793=VERTEX_POINT('',#25782);
#7794=VERTEX_POINT('',#25786);
#7795=VERTEX_POINT('',#25787);
#7796=VERTEX_POINT('',#25789);
#7797=VERTEX_POINT('',#25791);
#7798=VERTEX_POINT('',#25795);
#7799=VERTEX_POINT('',#25797);
#7800=VERTEX_POINT('',#25801);
#7801=VERTEX_POINT('',#25803);
#7802=VERTEX_POINT('',#25810);
#7803=VERTEX_POINT('',#25812);
#7804=VERTEX_POINT('',#25816);
#7805=VERTEX_POINT('',#25820);
#7806=VERTEX_POINT('',#25828);
#7807=VERTEX_POINT('',#25830);
#7808=VERTEX_POINT('',#25834);
#7809=VERTEX_POINT('',#25836);
#7810=VERTEX_POINT('',#25843);
#7811=VERTEX_POINT('',#25845);
#7812=VERTEX_POINT('',#25849);
#7813=VERTEX_POINT('',#25851);
#7814=VERTEX_POINT('',#25858);
#7815=VERTEX_POINT('',#25859);
#7816=VERTEX_POINT('',#25861);
#7817=VERTEX_POINT('',#25863);
#7818=VERTEX_POINT('',#25867);
#7819=VERTEX_POINT('',#25869);
#7820=VERTEX_POINT('',#25873);
#7821=VERTEX_POINT('',#25875);
#7822=VERTEX_POINT('',#25885);
#7823=VERTEX_POINT('',#25886);
#7824=VERTEX_POINT('',#25888);
#7825=VERTEX_POINT('',#25890);
#7826=VERTEX_POINT('',#25894);
#7827=VERTEX_POINT('',#25896);
#7828=VERTEX_POINT('',#25900);
#7829=VERTEX_POINT('',#25902);
#7830=VERTEX_POINT('',#25912);
#7831=VERTEX_POINT('',#25913);
#7832=VERTEX_POINT('',#25915);
#7833=VERTEX_POINT('',#25917);
#7834=VERTEX_POINT('',#25921);
#7835=VERTEX_POINT('',#25923);
#7836=VERTEX_POINT('',#25927);
#7837=VERTEX_POINT('',#25929);
#7838=VERTEX_POINT('',#25933);
#7839=VERTEX_POINT('',#25935);
#7840=VERTEX_POINT('',#25939);
#7841=VERTEX_POINT('',#25941);
#7842=VERTEX_POINT('',#25950);
#7843=VERTEX_POINT('',#25952);
#7844=VERTEX_POINT('',#25955);
#7845=VERTEX_POINT('',#25960);
#7846=VERTEX_POINT('',#25963);
#7847=VERTEX_POINT('',#25967);
#7848=VERTEX_POINT('',#25971);
#7849=VERTEX_POINT('',#25975);
#7850=VERTEX_POINT('',#25978);
#7851=VERTEX_POINT('',#25986);
#7852=VERTEX_POINT('',#25988);
#7853=VERTEX_POINT('',#25993);
#7854=VERTEX_POINT('',#25994);
#7855=VERTEX_POINT('',#25996);
#7856=VERTEX_POINT('',#25998);
#7857=VERTEX_POINT('',#26002);
#7858=VERTEX_POINT('',#26004);
#7859=VERTEX_POINT('',#26008);
#7860=VERTEX_POINT('',#26010);
#7861=VERTEX_POINT('',#26018);
#7862=VERTEX_POINT('',#26019);
#7863=VERTEX_POINT('',#26021);
#7864=VERTEX_POINT('',#26023);
#7865=VERTEX_POINT('',#26027);
#7866=VERTEX_POINT('',#26029);
#7867=VERTEX_POINT('',#26033);
#7868=VERTEX_POINT('',#26035);
#7869=VERTEX_POINT('',#26043);
#7870=VERTEX_POINT('',#26045);
#7871=VERTEX_POINT('',#26048);
#7872=VERTEX_POINT('',#26050);
#7873=VERTEX_POINT('',#26055);
#7874=VERTEX_POINT('',#26059);
#7875=VERTEX_POINT('',#26066);
#7876=VERTEX_POINT('',#26068);
#7877=VERTEX_POINT('',#26072);
#7878=VERTEX_POINT('',#26074);
#7879=VERTEX_POINT('',#26081);
#7880=VERTEX_POINT('',#26083);
#7881=VERTEX_POINT('',#26087);
#7882=VERTEX_POINT('',#26089);
#7883=VERTEX_POINT('',#26096);
#7884=VERTEX_POINT('',#26097);
#7885=VERTEX_POINT('',#26101);
#7886=VERTEX_POINT('',#26112);
#7887=VERTEX_POINT('',#26114);
#7888=VERTEX_POINT('',#26116);
#7889=VERTEX_POINT('',#26153);
#7890=VERTEX_POINT('',#26168);
#7891=VERTEX_POINT('',#26170);
#7892=VERTEX_POINT('',#26174);
#7893=VERTEX_POINT('',#26176);
#7894=VERTEX_POINT('',#26183);
#7895=VERTEX_POINT('',#26185);
#7896=VERTEX_POINT('',#26189);
#7897=VERTEX_POINT('',#26190);
#7898=VERTEX_POINT('',#26192);
#7899=VERTEX_POINT('',#26194);
#7900=VERTEX_POINT('',#26198);
#7901=VERTEX_POINT('',#26200);
#7902=VERTEX_POINT('',#26204);
#7903=VERTEX_POINT('',#26206);
#7904=VERTEX_POINT('',#26210);
#7905=VERTEX_POINT('',#26216);
#7906=VERTEX_POINT('',#26217);
#7907=VERTEX_POINT('',#26219);
#7908=VERTEX_POINT('',#26221);
#7909=VERTEX_POINT('',#26225);
#7910=VERTEX_POINT('',#26227);
#7911=VERTEX_POINT('',#26231);
#7912=VERTEX_POINT('',#26235);
#7913=VERTEX_POINT('',#26241);
#7914=VERTEX_POINT('',#26247);
#7915=VERTEX_POINT('',#26249);
#7916=VERTEX_POINT('',#26253);
#7917=VERTEX_POINT('',#26255);
#7918=VERTEX_POINT('',#26262);
#7919=VERTEX_POINT('',#26264);
#7920=VERTEX_POINT('',#26268);
#7921=VERTEX_POINT('',#26270);
#7922=VERTEX_POINT('',#26277);
#7923=VERTEX_POINT('',#26279);
#7924=VERTEX_POINT('',#26283);
#7925=VERTEX_POINT('',#26285);
#7926=VERTEX_POINT('',#26292);
#7927=VERTEX_POINT('',#26294);
#7928=VERTEX_POINT('',#26298);
#7929=VERTEX_POINT('',#26300);
#7930=VERTEX_POINT('',#26307);
#7931=VERTEX_POINT('',#26309);
#7932=VERTEX_POINT('',#26313);
#7933=VERTEX_POINT('',#26315);
#7934=VERTEX_POINT('',#26322);
#7935=VERTEX_POINT('',#26323);
#7936=VERTEX_POINT('',#26325);
#7937=VERTEX_POINT('',#26327);
#7938=VERTEX_POINT('',#26331);
#7939=VERTEX_POINT('',#26333);
#7940=VERTEX_POINT('',#26337);
#7941=VERTEX_POINT('',#26339);
#7942=VERTEX_POINT('',#26343);
#7943=VERTEX_POINT('',#26345);
#7944=VERTEX_POINT('',#26349);
#7945=VERTEX_POINT('',#26351);
#7946=VERTEX_POINT('',#26360);
#7947=VERTEX_POINT('',#26362);
#7948=VERTEX_POINT('',#26365);
#7949=VERTEX_POINT('',#26370);
#7950=VERTEX_POINT('',#26373);
#7951=VERTEX_POINT('',#26377);
#7952=VERTEX_POINT('',#26381);
#7953=VERTEX_POINT('',#26385);
#7954=VERTEX_POINT('',#26388);
#7955=VERTEX_POINT('',#26396);
#7956=VERTEX_POINT('',#26398);
#7957=VERTEX_POINT('',#26403);
#7958=VERTEX_POINT('',#26404);
#7959=VERTEX_POINT('',#26406);
#7960=VERTEX_POINT('',#26408);
#7961=VERTEX_POINT('',#26412);
#7962=VERTEX_POINT('',#26414);
#7963=VERTEX_POINT('',#26418);
#7964=VERTEX_POINT('',#26420);
#7965=VERTEX_POINT('',#26428);
#7966=VERTEX_POINT('',#26430);
#7967=VERTEX_POINT('',#26433);
#7968=VERTEX_POINT('',#26435);
#7969=VERTEX_POINT('',#26440);
#7970=VERTEX_POINT('',#26444);
#7971=VERTEX_POINT('',#26451);
#7972=VERTEX_POINT('',#26453);
#7973=VERTEX_POINT('',#26457);
#7974=VERTEX_POINT('',#26459);
#7975=VERTEX_POINT('',#26466);
#7976=VERTEX_POINT('',#26468);
#7977=VERTEX_POINT('',#26472);
#7978=VERTEX_POINT('',#26474);
#7979=VERTEX_POINT('',#26481);
#7980=VERTEX_POINT('',#26482);
#7981=VERTEX_POINT('',#26486);
#7982=VERTEX_POINT('',#26501);
#7983=VERTEX_POINT('',#26503);
#7984=VERTEX_POINT('',#26505);
#7985=VERTEX_POINT('',#26542);
#7986=VERTEX_POINT('',#26561);
#7987=VERTEX_POINT('',#26563);
#7988=VERTEX_POINT('',#26567);
#7989=VERTEX_POINT('',#26569);
#7990=VERTEX_POINT('',#26576);
#7991=VERTEX_POINT('',#26578);
#7992=VERTEX_POINT('',#26582);
#7993=VERTEX_POINT('',#26584);
#7994=VERTEX_POINT('',#26592);
#7995=VERTEX_POINT('',#26594);
#7996=VERTEX_POINT('',#26599);
#7997=VERTEX_POINT('',#26600);
#7998=VERTEX_POINT('',#26602);
#7999=VERTEX_POINT('',#26604);
#8000=VERTEX_POINT('',#26608);
#8001=VERTEX_POINT('',#26610);
#8002=VERTEX_POINT('',#26614);
#8003=VERTEX_POINT('',#26616);
#8004=VERTEX_POINT('',#26624);
#8005=VERTEX_POINT('',#26626);
#8006=VERTEX_POINT('',#26629);
#8007=VERTEX_POINT('',#26631);
#8008=VERTEX_POINT('',#26636);
#8009=VERTEX_POINT('',#26640);
#8010=VERTEX_POINT('',#26647);
#8011=VERTEX_POINT('',#26649);
#8012=VERTEX_POINT('',#26653);
#8013=VERTEX_POINT('',#26655);
#8014=VERTEX_POINT('',#26662);
#8015=VERTEX_POINT('',#26664);
#8016=VERTEX_POINT('',#26668);
#8017=VERTEX_POINT('',#26670);
#8018=VERTEX_POINT('',#26677);
#8019=VERTEX_POINT('',#26678);
#8020=VERTEX_POINT('',#26682);
#8021=VERTEX_POINT('',#26693);
#8022=VERTEX_POINT('',#26695);
#8023=VERTEX_POINT('',#26697);
#8024=VERTEX_POINT('',#26734);
#8025=VERTEX_POINT('',#26749);
#8026=VERTEX_POINT('',#26751);
#8027=VERTEX_POINT('',#26755);
#8028=VERTEX_POINT('',#26757);
#8029=VERTEX_POINT('',#26764);
#8030=VERTEX_POINT('',#26766);
#8031=VERTEX_POINT('',#26770);
#8032=VERTEX_POINT('',#26772);
#8033=VERTEX_POINT('',#26779);
#8034=VERTEX_POINT('',#26780);
#8035=VERTEX_POINT('',#26782);
#8036=VERTEX_POINT('',#26784);
#8037=VERTEX_POINT('',#26788);
#8038=VERTEX_POINT('',#26790);
#8039=VERTEX_POINT('',#26794);
#8040=VERTEX_POINT('',#26796);
#8041=VERTEX_POINT('',#26800);
#8042=VERTEX_POINT('',#26801);
#8043=VERTEX_POINT('',#26803);
#8044=VERTEX_POINT('',#26874);
#8045=VERTEX_POINT('',#26876);
#8046=VERTEX_POINT('',#26947);
#8047=VERTEX_POINT('',#26949);
#8048=VERTEX_POINT('',#27020);
#8049=VERTEX_POINT('',#27022);
#8050=VERTEX_POINT('',#27093);
#8051=VERTEX_POINT('',#27095);
#8052=VERTEX_POINT('',#27166);
#8053=VERTEX_POINT('',#27168);
#8054=VERTEX_POINT('',#27239);
#8055=VERTEX_POINT('',#27241);
#8056=VERTEX_POINT('',#27312);
#8057=VERTEX_POINT('',#27314);
#8058=VERTEX_POINT('',#27385);
#8059=VERTEX_POINT('',#27387);
#8060=VERTEX_POINT('',#27458);
#8061=VERTEX_POINT('',#27460);
#8062=VERTEX_POINT('',#27531);
#8063=VERTEX_POINT('',#27533);
#8064=VERTEX_POINT('',#27604);
#8065=VERTEX_POINT('',#27606);
#8066=VERTEX_POINT('',#27677);
#8067=VERTEX_POINT('',#27679);
#8068=VERTEX_POINT('',#27750);
#8069=VERTEX_POINT('',#27752);
#8070=VERTEX_POINT('',#27823);
#8071=VERTEX_POINT('',#27825);
#8072=VERTEX_POINT('',#27896);
#8073=VERTEX_POINT('',#27898);
#8074=VERTEX_POINT('',#27969);
#8075=VERTEX_POINT('',#27971);
#8076=VERTEX_POINT('',#28042);
#8077=VERTEX_POINT('',#28044);
#8078=VERTEX_POINT('',#28115);
#8079=VERTEX_POINT('',#28117);
#8080=VERTEX_POINT('',#28188);
#8081=VERTEX_POINT('',#28190);
#8082=VERTEX_POINT('',#28261);
#8083=VERTEX_POINT('',#28263);
#8084=VERTEX_POINT('',#28334);
#8085=VERTEX_POINT('',#28336);
#8086=VERTEX_POINT('',#28407);
#8087=VERTEX_POINT('',#28409);
#8088=VERTEX_POINT('',#28480);
#8089=VERTEX_POINT('',#28482);
#8090=VERTEX_POINT('',#28553);
#8091=VERTEX_POINT('',#28555);
#8092=VERTEX_POINT('',#28626);
#8093=VERTEX_POINT('',#28628);
#8094=VERTEX_POINT('',#28699);
#8095=VERTEX_POINT('',#28701);
#8096=VERTEX_POINT('',#28772);
#8097=VERTEX_POINT('',#28774);
#8098=VERTEX_POINT('',#28845);
#8099=VERTEX_POINT('',#28847);
#8100=VERTEX_POINT('',#28918);
#8101=VERTEX_POINT('',#28920);
#8102=VERTEX_POINT('',#28991);
#8103=VERTEX_POINT('',#28993);
#8104=VERTEX_POINT('',#29064);
#8105=VERTEX_POINT('',#29066);
#8106=VERTEX_POINT('',#29137);
#8107=VERTEX_POINT('',#29139);
#8108=VERTEX_POINT('',#29210);
#8109=VERTEX_POINT('',#29212);
#8110=VERTEX_POINT('',#29283);
#8111=VERTEX_POINT('',#29285);
#8112=VERTEX_POINT('',#29356);
#8113=VERTEX_POINT('',#29358);
#8114=VERTEX_POINT('',#29429);
#8115=VERTEX_POINT('',#29431);
#8116=VERTEX_POINT('',#29502);
#8117=VERTEX_POINT('',#29504);
#8118=VERTEX_POINT('',#29575);
#8119=VERTEX_POINT('',#29577);
#8120=VERTEX_POINT('',#29648);
#8121=VERTEX_POINT('',#29724);
#8122=VERTEX_POINT('',#29726);
#8123=VERTEX_POINT('',#29870);
#8124=VERTEX_POINT('',#29872);
#8125=VERTEX_POINT('',#29945);
#8126=VERTEX_POINT('',#30088);
#8127=VERTEX_POINT('',#30161);
#8128=VERTEX_POINT('',#30304);
#8129=VERTEX_POINT('',#30377);
#8130=VERTEX_POINT('',#30520);
#8131=VERTEX_POINT('',#30593);
#8132=VERTEX_POINT('',#30736);
#8133=VERTEX_POINT('',#30809);
#8134=VERTEX_POINT('',#30952);
#8135=VERTEX_POINT('',#31025);
#8136=VERTEX_POINT('',#31168);
#8137=VERTEX_POINT('',#31241);
#8138=VERTEX_POINT('',#31384);
#8139=VERTEX_POINT('',#31457);
#8140=VERTEX_POINT('',#31600);
#8141=VERTEX_POINT('',#31673);
#8142=VERTEX_POINT('',#31816);
#8143=VERTEX_POINT('',#31889);
#8144=VERTEX_POINT('',#32032);
#8145=VERTEX_POINT('',#32105);
#8146=VERTEX_POINT('',#32248);
#8147=VERTEX_POINT('',#32321);
#8148=VERTEX_POINT('',#32464);
#8149=VERTEX_POINT('',#32537);
#8150=VERTEX_POINT('',#32680);
#8151=VERTEX_POINT('',#32753);
#8152=VERTEX_POINT('',#32896);
#8153=VERTEX_POINT('',#32969);
#8154=VERTEX_POINT('',#33112);
#8155=VERTEX_POINT('',#33185);
#8156=VERTEX_POINT('',#33328);
#8157=VERTEX_POINT('',#33401);
#8158=VERTEX_POINT('',#33544);
#8159=VERTEX_POINT('',#33617);
#8160=VERTEX_POINT('',#33760);
#8161=VERTEX_POINT('',#33833);
#8162=VERTEX_POINT('',#33976);
#8163=VERTEX_POINT('',#34049);
#8164=VERTEX_POINT('',#34192);
#8165=VERTEX_POINT('',#34265);
#8166=VERTEX_POINT('',#34408);
#8167=VERTEX_POINT('',#34481);
#8168=VERTEX_POINT('',#34624);
#8169=VERTEX_POINT('',#34697);
#8170=VERTEX_POINT('',#34840);
#8171=VERTEX_POINT('',#34913);
#8172=VERTEX_POINT('',#35056);
#8173=VERTEX_POINT('',#35129);
#8174=VERTEX_POINT('',#35272);
#8175=VERTEX_POINT('',#35345);
#8176=VERTEX_POINT('',#35488);
#8177=VERTEX_POINT('',#35561);
#8178=VERTEX_POINT('',#35704);
#8179=VERTEX_POINT('',#35777);
#8180=VERTEX_POINT('',#35920);
#8181=VERTEX_POINT('',#35993);
#8182=VERTEX_POINT('',#36136);
#8183=VERTEX_POINT('',#36209);
#8184=VERTEX_POINT('',#36352);
#8185=VERTEX_POINT('',#36425);
#8186=VERTEX_POINT('',#36568);
#8187=VERTEX_POINT('',#36641);
#8188=VERTEX_POINT('',#36784);
#8189=VERTEX_POINT('',#36857);
#8190=VERTEX_POINT('',#37000);
#8191=VERTEX_POINT('',#37073);
#8192=VERTEX_POINT('',#37216);
#8193=VERTEX_POINT('',#37289);
#8194=VERTEX_POINT('',#37432);
#8195=VERTEX_POINT('',#37505);
#8196=VERTEX_POINT('',#37648);
#8197=VERTEX_POINT('',#37721);
#8198=VERTEX_POINT('',#37864);
#8199=VERTEX_POINT('',#37937);
#8200=VERTEX_POINT('',#38080);
#8201=VERTEX_POINT('',#38153);
#8202=VERTEX_POINT('',#38296);
#8203=VERTEX_POINT('',#38373);
#8204=VERTEX_POINT('',#38374);
#8205=VERTEX_POINT('',#38376);
#8206=VERTEX_POINT('',#38378);
#8207=VERTEX_POINT('',#38380);
#8208=VERTEX_POINT('',#38382);
#8209=VERTEX_POINT('',#38384);
#8210=VERTEX_POINT('',#38386);
#8211=VERTEX_POINT('',#38390);
#8212=VERTEX_POINT('',#38392);
#8213=VERTEX_POINT('',#38396);
#8214=VERTEX_POINT('',#38400);
#8215=VERTEX_POINT('',#38404);
#8216=VERTEX_POINT('',#38408);
#8217=VERTEX_POINT('',#38410);
#8218=VERTEX_POINT('',#38412);
#8219=VERTEX_POINT('',#38425);
#8220=VERTEX_POINT('',#38427);
#8221=VERTEX_POINT('',#38432);
#8222=VERTEX_POINT('',#38433);
#8223=VERTEX_POINT('',#38435);
#8224=VERTEX_POINT('',#38437);
#8225=VERTEX_POINT('',#38441);
#8226=VERTEX_POINT('',#38443);
#8227=VERTEX_POINT('',#38447);
#8228=VERTEX_POINT('',#38449);
#8229=VERTEX_POINT('',#38457);
#8230=VERTEX_POINT('',#38459);
#8231=VERTEX_POINT('',#38462);
#8232=VERTEX_POINT('',#38464);
#8233=VERTEX_POINT('',#38469);
#8234=VERTEX_POINT('',#38473);
#8235=VERTEX_POINT('',#38480);
#8236=VERTEX_POINT('',#38482);
#8237=VERTEX_POINT('',#38486);
#8238=VERTEX_POINT('',#38488);
#8239=VERTEX_POINT('',#38495);
#8240=VERTEX_POINT('',#38497);
#8241=VERTEX_POINT('',#38501);
#8242=VERTEX_POINT('',#38503);
#8243=VERTEX_POINT('',#38510);
#8244=VERTEX_POINT('',#38511);
#8245=VERTEX_POINT('',#38515);
#8246=VERTEX_POINT('',#38530);
#8247=VERTEX_POINT('',#38532);
#8248=VERTEX_POINT('',#38534);
#8249=VERTEX_POINT('',#38571);
#8250=VERTEX_POINT('',#38590);
#8251=VERTEX_POINT('',#38592);
#8252=VERTEX_POINT('',#38596);
#8253=VERTEX_POINT('',#38598);
#8254=VERTEX_POINT('',#38605);
#8255=VERTEX_POINT('',#38607);
#8256=VERTEX_POINT('',#38611);
#8257=VERTEX_POINT('',#38613);
#8258=VERTEX_POINT('',#38620);
#8259=VERTEX_POINT('',#38622);
#8260=VERTEX_POINT('',#38626);
#8261=VERTEX_POINT('',#38628);
#8262=VERTEX_POINT('',#38635);
#8263=VERTEX_POINT('',#38636);
#8264=VERTEX_POINT('',#38640);
#8265=VERTEX_POINT('',#38651);
#8266=VERTEX_POINT('',#38653);
#8267=VERTEX_POINT('',#38655);
#8268=VERTEX_POINT('',#38692);
#8269=VERTEX_POINT('',#38707);
#8270=VERTEX_POINT('',#38708);
#8271=VERTEX_POINT('',#38710);
#8272=VERTEX_POINT('',#38712);
#8273=VERTEX_POINT('',#38716);
#8274=VERTEX_POINT('',#38720);
#8275=VERTEX_POINT('',#38726);
#8276=VERTEX_POINT('',#38728);
#8277=VERTEX_POINT('',#38732);
#8278=VERTEX_POINT('',#38734);
#8279=VERTEX_POINT('',#38741);
#8280=VERTEX_POINT('',#38743);
#8281=VERTEX_POINT('',#38747);
#8282=VERTEX_POINT('',#38749);
#8283=VERTEX_POINT('',#38756);
#8284=VERTEX_POINT('',#38757);
#8285=VERTEX_POINT('',#38759);
#8286=VERTEX_POINT('',#38761);
#8287=VERTEX_POINT('',#38765);
#8288=VERTEX_POINT('',#38767);
#8289=VERTEX_POINT('',#38771);
#8290=VERTEX_POINT('',#38773);
#8291=VERTEX_POINT('',#38777);
#8292=VERTEX_POINT('',#38778);
#8293=VERTEX_POINT('',#38780);
#8294=VERTEX_POINT('',#38851);
#8295=VERTEX_POINT('',#38853);
#8296=VERTEX_POINT('',#38924);
#8297=VERTEX_POINT('',#38926);
#8298=VERTEX_POINT('',#38997);
#8299=VERTEX_POINT('',#38999);
#8300=VERTEX_POINT('',#39070);
#8301=VERTEX_POINT('',#39072);
#8302=VERTEX_POINT('',#39143);
#8303=VERTEX_POINT('',#39145);
#8304=VERTEX_POINT('',#39216);
#8305=VERTEX_POINT('',#39218);
#8306=VERTEX_POINT('',#39289);
#8307=VERTEX_POINT('',#39291);
#8308=VERTEX_POINT('',#39362);
#8309=VERTEX_POINT('',#39364);
#8310=VERTEX_POINT('',#39435);
#8311=VERTEX_POINT('',#39437);
#8312=VERTEX_POINT('',#39508);
#8313=VERTEX_POINT('',#39510);
#8314=VERTEX_POINT('',#39581);
#8315=VERTEX_POINT('',#39583);
#8316=VERTEX_POINT('',#39654);
#8317=VERTEX_POINT('',#39656);
#8318=VERTEX_POINT('',#39727);
#8319=VERTEX_POINT('',#39729);
#8320=VERTEX_POINT('',#39800);
#8321=VERTEX_POINT('',#39802);
#8322=VERTEX_POINT('',#39873);
#8323=VERTEX_POINT('',#39875);
#8324=VERTEX_POINT('',#39946);
#8325=VERTEX_POINT('',#39948);
#8326=VERTEX_POINT('',#40019);
#8327=VERTEX_POINT('',#40021);
#8328=VERTEX_POINT('',#40092);
#8329=VERTEX_POINT('',#40094);
#8330=VERTEX_POINT('',#40165);
#8331=VERTEX_POINT('',#40167);
#8332=VERTEX_POINT('',#40238);
#8333=VERTEX_POINT('',#40240);
#8334=VERTEX_POINT('',#40311);
#8335=VERTEX_POINT('',#40313);
#8336=VERTEX_POINT('',#40384);
#8337=VERTEX_POINT('',#40386);
#8338=VERTEX_POINT('',#40457);
#8339=VERTEX_POINT('',#40459);
#8340=VERTEX_POINT('',#40530);
#8341=VERTEX_POINT('',#40532);
#8342=VERTEX_POINT('',#40603);
#8343=VERTEX_POINT('',#40605);
#8344=VERTEX_POINT('',#40676);
#8345=VERTEX_POINT('',#40678);
#8346=VERTEX_POINT('',#40749);
#8347=VERTEX_POINT('',#40751);
#8348=VERTEX_POINT('',#40822);
#8349=VERTEX_POINT('',#40824);
#8350=VERTEX_POINT('',#40895);
#8351=VERTEX_POINT('',#40897);
#8352=VERTEX_POINT('',#40968);
#8353=VERTEX_POINT('',#40970);
#8354=VERTEX_POINT('',#41041);
#8355=VERTEX_POINT('',#41043);
#8356=VERTEX_POINT('',#41114);
#8357=VERTEX_POINT('',#41116);
#8358=VERTEX_POINT('',#41187);
#8359=VERTEX_POINT('',#41189);
#8360=VERTEX_POINT('',#41260);
#8361=VERTEX_POINT('',#41262);
#8362=VERTEX_POINT('',#41333);
#8363=VERTEX_POINT('',#41335);
#8364=VERTEX_POINT('',#41406);
#8365=VERTEX_POINT('',#41408);
#8366=VERTEX_POINT('',#41479);
#8367=VERTEX_POINT('',#41481);
#8368=VERTEX_POINT('',#41552);
#8369=VERTEX_POINT('',#41554);
#8370=VERTEX_POINT('',#41625);
#8371=VERTEX_POINT('',#41627);
#8372=VERTEX_POINT('',#41698);
#8373=VERTEX_POINT('',#41700);
#8374=VERTEX_POINT('',#41771);
#8375=VERTEX_POINT('',#41773);
#8376=VERTEX_POINT('',#41844);
#8377=VERTEX_POINT('',#41846);
#8378=VERTEX_POINT('',#41917);
#8379=VERTEX_POINT('',#41919);
#8380=VERTEX_POINT('',#41990);
#8381=VERTEX_POINT('',#41992);
#8382=VERTEX_POINT('',#42063);
#8383=VERTEX_POINT('',#42065);
#8384=VERTEX_POINT('',#42136);
#8385=VERTEX_POINT('',#42138);
#8386=VERTEX_POINT('',#42209);
#8387=VERTEX_POINT('',#42211);
#8388=VERTEX_POINT('',#42282);
#8389=VERTEX_POINT('',#42284);
#8390=VERTEX_POINT('',#42355);
#8391=VERTEX_POINT('',#42357);
#8392=VERTEX_POINT('',#42428);
#8393=VERTEX_POINT('',#42430);
#8394=VERTEX_POINT('',#42501);
#8395=VERTEX_POINT('',#42503);
#8396=VERTEX_POINT('',#42574);
#8397=VERTEX_POINT('',#42576);
#8398=VERTEX_POINT('',#42647);
#8399=VERTEX_POINT('',#42649);
#8400=VERTEX_POINT('',#42720);
#8401=VERTEX_POINT('',#42722);
#8402=VERTEX_POINT('',#42793);
#8403=VERTEX_POINT('',#42795);
#8404=VERTEX_POINT('',#42866);
#8405=VERTEX_POINT('',#42868);
#8406=VERTEX_POINT('',#42939);
#8407=VERTEX_POINT('',#42941);
#8408=VERTEX_POINT('',#43012);
#8409=VERTEX_POINT('',#43014);
#8410=VERTEX_POINT('',#43085);
#8411=VERTEX_POINT('',#43087);
#8412=VERTEX_POINT('',#43158);
#8413=VERTEX_POINT('',#43160);
#8414=VERTEX_POINT('',#43231);
#8415=VERTEX_POINT('',#43233);
#8416=VERTEX_POINT('',#43304);
#8417=VERTEX_POINT('',#43306);
#8418=VERTEX_POINT('',#43377);
#8419=VERTEX_POINT('',#43379);
#8420=VERTEX_POINT('',#43450);
#8421=VERTEX_POINT('',#43452);
#8422=VERTEX_POINT('',#43523);
#8423=VERTEX_POINT('',#43525);
#8424=VERTEX_POINT('',#43596);
#8425=VERTEX_POINT('',#43598);
#8426=VERTEX_POINT('',#43669);
#8427=VERTEX_POINT('',#43671);
#8428=VERTEX_POINT('',#43742);
#8429=VERTEX_POINT('',#43744);
#8430=VERTEX_POINT('',#43815);
#8431=VERTEX_POINT('',#43817);
#8432=VERTEX_POINT('',#43888);
#8433=VERTEX_POINT('',#43890);
#8434=VERTEX_POINT('',#43961);
#8435=VERTEX_POINT('',#43963);
#8436=VERTEX_POINT('',#44034);
#8437=VERTEX_POINT('',#44036);
#8438=VERTEX_POINT('',#44107);
#8439=VERTEX_POINT('',#44109);
#8440=VERTEX_POINT('',#44180);
#8441=VERTEX_POINT('',#44182);
#8442=VERTEX_POINT('',#44253);
#8443=VERTEX_POINT('',#44255);
#8444=VERTEX_POINT('',#44326);
#8445=VERTEX_POINT('',#44328);
#8446=VERTEX_POINT('',#44399);
#8447=VERTEX_POINT('',#44401);
#8448=VERTEX_POINT('',#44472);
#8449=VERTEX_POINT('',#44474);
#8450=VERTEX_POINT('',#44545);
#8451=VERTEX_POINT('',#44621);
#8452=VERTEX_POINT('',#44623);
#8453=VERTEX_POINT('',#44767);
#8454=VERTEX_POINT('',#44774);
#8455=VERTEX_POINT('',#44986);
#8456=VERTEX_POINT('',#44993);
#8457=VERTEX_POINT('',#45068);
#8458=VERTEX_POINT('',#45216);
#8459=VERTEX_POINT('',#45428);
#8460=VERTEX_POINT('',#45435);
#8461=VERTEX_POINT('',#45510);
#8462=VERTEX_POINT('',#45658);
#8463=VERTEX_POINT('',#45870);
#8464=VERTEX_POINT('',#45877);
#8465=VERTEX_POINT('',#45952);
#8466=VERTEX_POINT('',#46100);
#8467=VERTEX_POINT('',#46312);
#8468=VERTEX_POINT('',#46319);
#8469=VERTEX_POINT('',#46394);
#8470=VERTEX_POINT('',#46542);
#8471=VERTEX_POINT('',#46754);
#8472=VERTEX_POINT('',#46761);
#8473=VERTEX_POINT('',#46836);
#8474=VERTEX_POINT('',#46984);
#8475=VERTEX_POINT('',#47196);
#8476=VERTEX_POINT('',#47203);
#8477=VERTEX_POINT('',#47278);
#8478=VERTEX_POINT('',#47426);
#8479=VERTEX_POINT('',#47638);
#8480=VERTEX_POINT('',#47645);
#8481=VERTEX_POINT('',#47720);
#8482=VERTEX_POINT('',#47868);
#8483=VERTEX_POINT('',#48080);
#8484=VERTEX_POINT('',#48087);
#8485=VERTEX_POINT('',#48162);
#8486=VERTEX_POINT('',#48310);
#8487=VERTEX_POINT('',#48522);
#8488=VERTEX_POINT('',#48529);
#8489=VERTEX_POINT('',#48604);
#8490=VERTEX_POINT('',#48752);
#8491=VERTEX_POINT('',#48964);
#8492=VERTEX_POINT('',#48971);
#8493=VERTEX_POINT('',#49046);
#8494=VERTEX_POINT('',#49194);
#8495=VERTEX_POINT('',#49406);
#8496=VERTEX_POINT('',#49413);
#8497=VERTEX_POINT('',#49488);
#8498=VERTEX_POINT('',#49636);
#8499=VERTEX_POINT('',#49848);
#8500=VERTEX_POINT('',#49855);
#8501=VERTEX_POINT('',#49930);
#8502=VERTEX_POINT('',#50078);
#8503=VERTEX_POINT('',#50290);
#8504=VERTEX_POINT('',#50297);
#8505=VERTEX_POINT('',#50372);
#8506=VERTEX_POINT('',#50520);
#8507=VERTEX_POINT('',#50732);
#8508=VERTEX_POINT('',#50739);
#8509=VERTEX_POINT('',#50814);
#8510=VERTEX_POINT('',#50962);
#8511=VERTEX_POINT('',#51174);
#8512=VERTEX_POINT('',#51181);
#8513=VERTEX_POINT('',#51256);
#8514=VERTEX_POINT('',#51404);
#8515=VERTEX_POINT('',#51616);
#8516=VERTEX_POINT('',#51623);
#8517=VERTEX_POINT('',#51698);
#8518=VERTEX_POINT('',#51846);
#8519=VERTEX_POINT('',#52058);
#8520=VERTEX_POINT('',#52065);
#8521=VERTEX_POINT('',#52140);
#8522=VERTEX_POINT('',#52288);
#8523=VERTEX_POINT('',#52500);
#8524=VERTEX_POINT('',#52507);
#8525=VERTEX_POINT('',#52582);
#8526=VERTEX_POINT('',#52730);
#8527=VERTEX_POINT('',#52942);
#8528=VERTEX_POINT('',#52949);
#8529=VERTEX_POINT('',#53024);
#8530=VERTEX_POINT('',#53172);
#8531=VERTEX_POINT('',#53384);
#8532=VERTEX_POINT('',#53391);
#8533=VERTEX_POINT('',#53466);
#8534=VERTEX_POINT('',#53614);
#8535=VERTEX_POINT('',#53826);
#8536=VERTEX_POINT('',#53833);
#8537=VERTEX_POINT('',#53908);
#8538=VERTEX_POINT('',#54056);
#8539=VERTEX_POINT('',#54268);
#8540=VERTEX_POINT('',#54275);
#8541=VERTEX_POINT('',#54350);
#8542=VERTEX_POINT('',#54498);
#8543=VERTEX_POINT('',#54710);
#8544=VERTEX_POINT('',#54717);
#8545=VERTEX_POINT('',#54792);
#8546=VERTEX_POINT('',#54940);
#8547=VERTEX_POINT('',#55152);
#8548=VERTEX_POINT('',#55159);
#8549=VERTEX_POINT('',#55234);
#8550=VERTEX_POINT('',#55382);
#8551=VERTEX_POINT('',#55594);
#8552=VERTEX_POINT('',#55601);
#8553=VERTEX_POINT('',#55676);
#8554=VERTEX_POINT('',#55824);
#8555=VERTEX_POINT('',#56036);
#8556=VERTEX_POINT('',#56043);
#8557=VERTEX_POINT('',#56118);
#8558=VERTEX_POINT('',#56266);
#8559=VERTEX_POINT('',#56478);
#8560=VERTEX_POINT('',#56485);
#8561=VERTEX_POINT('',#56560);
#8562=VERTEX_POINT('',#56708);
#8563=VERTEX_POINT('',#56920);
#8564=VERTEX_POINT('',#56927);
#8565=VERTEX_POINT('',#57002);
#8566=VERTEX_POINT('',#57150);
#8567=VERTEX_POINT('',#57362);
#8568=VERTEX_POINT('',#57369);
#8569=VERTEX_POINT('',#57444);
#8570=VERTEX_POINT('',#57592);
#8571=VERTEX_POINT('',#57804);
#8572=VERTEX_POINT('',#57811);
#8573=VERTEX_POINT('',#57886);
#8574=VERTEX_POINT('',#58034);
#8575=VERTEX_POINT('',#58246);
#8576=VERTEX_POINT('',#58253);
#8577=VERTEX_POINT('',#58328);
#8578=VERTEX_POINT('',#58476);
#8579=VERTEX_POINT('',#58688);
#8580=VERTEX_POINT('',#58695);
#8581=VERTEX_POINT('',#58770);
#8582=VERTEX_POINT('',#58918);
#8583=VERTEX_POINT('',#59130);
#8584=VERTEX_POINT('',#59137);
#8585=VERTEX_POINT('',#59212);
#8586=VERTEX_POINT('',#59360);
#8587=VERTEX_POINT('',#59572);
#8588=VERTEX_POINT('',#59579);
#8589=VERTEX_POINT('',#59654);
#8590=VERTEX_POINT('',#59802);
#8591=VERTEX_POINT('',#60014);
#8592=VERTEX_POINT('',#60021);
#8593=VERTEX_POINT('',#60096);
#8594=VERTEX_POINT('',#60244);
#8595=VERTEX_POINT('',#60456);
#8596=VERTEX_POINT('',#60463);
#8597=VERTEX_POINT('',#60538);
#8598=VERTEX_POINT('',#60686);
#8599=VERTEX_POINT('',#60898);
#8600=VERTEX_POINT('',#60905);
#8601=VERTEX_POINT('',#60980);
#8602=VERTEX_POINT('',#61128);
#8603=VERTEX_POINT('',#61340);
#8604=VERTEX_POINT('',#61347);
#8605=VERTEX_POINT('',#61422);
#8606=VERTEX_POINT('',#61570);
#8607=VERTEX_POINT('',#61643);
#8608=VERTEX_POINT('',#61786);
#8609=VERTEX_POINT('',#61864);
#8610=VERTEX_POINT('',#62012);
#8611=VERTEX_POINT('',#62019);
#8612=VERTEX_POINT('',#62231);
#8613=VERTEX_POINT('',#62310);
#8614=VERTEX_POINT('',#62311);
#8615=VERTEX_POINT('',#62313);
#8616=VERTEX_POINT('',#62315);
#8617=VERTEX_POINT('',#62317);
#8618=VERTEX_POINT('',#62319);
#8619=VERTEX_POINT('',#62321);
#8620=VERTEX_POINT('',#62323);
#8621=VERTEX_POINT('',#62327);
#8622=VERTEX_POINT('',#62329);
#8623=VERTEX_POINT('',#62333);
#8624=VERTEX_POINT('',#62337);
#8625=VERTEX_POINT('',#62341);
#8626=VERTEX_POINT('',#62345);
#8627=VERTEX_POINT('',#62346);
#8628=VERTEX_POINT('',#62349);
#8629=VERTEX_POINT('',#62361);
#8630=VERTEX_POINT('',#62362);
#8631=VERTEX_POINT('',#62364);
#8632=VERTEX_POINT('',#62366);
#8633=VERTEX_POINT('',#62370);
#8634=VERTEX_POINT('',#62372);
#8635=VERTEX_POINT('',#62376);
#8636=VERTEX_POINT('',#62378);
#8637=VERTEX_POINT('',#62382);
#8638=VERTEX_POINT('',#62384);
#8639=VERTEX_POINT('',#62388);
#8640=VERTEX_POINT('',#62390);
#8641=VERTEX_POINT('',#62398);
#8642=VERTEX_POINT('',#62401);
#8643=VERTEX_POINT('',#62405);
#8644=VERTEX_POINT('',#62409);
#8645=VERTEX_POINT('',#62415);
#8646=VERTEX_POINT('',#62418);
#8647=VERTEX_POINT('',#62422);
#8648=VERTEX_POINT('',#62426);
#8649=VERTEX_POINT('',#62430);
#8650=VERTEX_POINT('',#62433);
#8651=VERTEX_POINT('',#62437);
#8652=VERTEX_POINT('',#62441);
#8653=VERTEX_POINT('',#62446);
#8654=VERTEX_POINT('',#62447);
#8655=VERTEX_POINT('',#62449);
#8656=VERTEX_POINT('',#62451);
#8657=VERTEX_POINT('',#62455);
#8658=VERTEX_POINT('',#62457);
#8659=VERTEX_POINT('',#62461);
#8660=VERTEX_POINT('',#62463);
#8661=VERTEX_POINT('',#62467);
#8662=VERTEX_POINT('',#62469);
#8663=VERTEX_POINT('',#62473);
#8664=VERTEX_POINT('',#62475);
#8665=VERTEX_POINT('',#62591);
#8666=VERTEX_POINT('',#62593);
#8667=VERTEX_POINT('',#62597);
#8668=VERTEX_POINT('',#62599);
#8669=EDGE_CURVE('',#7212,#7212,#6550,.T.);
#8670=EDGE_CURVE('',#7212,#7213,#4286,.T.);
#8671=EDGE_CURVE('',#7213,#7213,#6551,.T.);
#8672=EDGE_CURVE('',#7214,#7214,#6552,.T.);
#8673=EDGE_CURVE('',#7214,#7215,#4287,.T.);
#8674=EDGE_CURVE('',#7215,#7215,#6553,.T.);
#8675=EDGE_CURVE('',#7216,#7216,#6554,.T.);
#8676=EDGE_CURVE('',#7216,#7217,#4288,.T.);
#8677=EDGE_CURVE('',#7217,#7217,#6555,.T.);
#8678=EDGE_CURVE('',#7218,#7219,#4289,.T.);
#8679=EDGE_CURVE('',#7219,#7220,#4290,.T.);
#8680=EDGE_CURVE('',#7221,#7220,#4291,.T.);
#8681=EDGE_CURVE('',#7218,#7221,#4292,.T.);
#8682=EDGE_CURVE('',#7222,#7218,#4293,.T.);
#8683=EDGE_CURVE('',#7223,#7221,#4294,.T.);
#8684=EDGE_CURVE('',#7222,#7223,#4295,.T.);
#8685=EDGE_CURVE('',#7224,#7222,#4296,.T.);
#8686=EDGE_CURVE('',#7225,#7223,#4297,.T.);
#8687=EDGE_CURVE('',#7224,#7225,#4298,.T.);
#8688=EDGE_CURVE('',#7219,#7224,#4299,.T.);
#8689=EDGE_CURVE('',#7220,#7225,#4300,.T.);
#8690=EDGE_CURVE('',#7226,#7226,#6556,.T.);
#8691=EDGE_CURVE('',#7226,#7227,#4301,.T.);
#8692=EDGE_CURVE('',#7227,#7227,#6557,.T.);
#8693=EDGE_CURVE('',#7228,#7228,#6558,.T.);
#8694=EDGE_CURVE('',#7228,#7229,#4302,.T.);
#8695=EDGE_CURVE('',#7229,#7229,#6559,.T.);
#8696=EDGE_CURVE('',#7230,#7230,#6560,.T.);
#8697=EDGE_CURVE('',#7230,#7231,#4303,.T.);
#8698=EDGE_CURVE('',#7231,#7231,#6561,.T.);
#8699=EDGE_CURVE('',#7232,#7232,#6562,.T.);
#8700=EDGE_CURVE('',#7232,#7233,#4304,.T.);
#8701=EDGE_CURVE('',#7233,#7233,#6563,.T.);
#8702=EDGE_CURVE('',#7234,#7234,#6564,.T.);
#8703=EDGE_CURVE('',#7234,#7235,#4305,.T.);
#8704=EDGE_CURVE('',#7235,#7235,#6565,.T.);
#8705=EDGE_CURVE('',#7236,#7236,#6566,.T.);
#8706=EDGE_CURVE('',#7236,#7237,#4306,.T.);
#8707=EDGE_CURVE('',#7237,#7237,#6567,.T.);
#8708=EDGE_CURVE('',#7238,#7238,#6568,.T.);
#8709=EDGE_CURVE('',#7238,#7239,#4307,.T.);
#8710=EDGE_CURVE('',#7239,#7239,#6569,.T.);
#8711=EDGE_CURVE('',#7240,#7240,#6570,.T.);
#8712=EDGE_CURVE('',#7240,#7241,#4308,.T.);
#8713=EDGE_CURVE('',#7241,#7241,#6571,.T.);
#8714=EDGE_CURVE('',#7242,#7242,#6572,.T.);
#8715=EDGE_CURVE('',#7242,#7243,#4309,.T.);
#8716=EDGE_CURVE('',#7243,#7243,#6573,.T.);
#8717=EDGE_CURVE('',#7244,#7244,#6574,.T.);
#8718=EDGE_CURVE('',#7244,#7245,#4310,.T.);
#8719=EDGE_CURVE('',#7245,#7245,#6575,.T.);
#8720=EDGE_CURVE('',#7246,#7246,#6576,.T.);
#8721=EDGE_CURVE('',#7246,#7247,#4311,.T.);
#8722=EDGE_CURVE('',#7247,#7247,#6577,.T.);
#8723=EDGE_CURVE('',#7248,#7248,#6578,.T.);
#8724=EDGE_CURVE('',#7248,#7249,#4312,.T.);
#8725=EDGE_CURVE('',#7249,#7249,#6579,.T.);
#8726=EDGE_CURVE('',#7250,#7250,#6580,.T.);
#8727=EDGE_CURVE('',#7250,#7251,#4313,.T.);
#8728=EDGE_CURVE('',#7251,#7251,#6581,.T.);
#8729=EDGE_CURVE('',#7252,#7252,#6582,.T.);
#8730=EDGE_CURVE('',#7252,#7253,#4314,.T.);
#8731=EDGE_CURVE('',#7253,#7253,#6583,.T.);
#8732=EDGE_CURVE('',#7254,#7254,#6584,.T.);
#8733=EDGE_CURVE('',#7254,#7255,#4315,.T.);
#8734=EDGE_CURVE('',#7255,#7255,#6585,.T.);
#8735=EDGE_CURVE('',#7256,#7256,#6586,.T.);
#8736=EDGE_CURVE('',#7256,#7257,#4316,.T.);
#8737=EDGE_CURVE('',#7257,#7257,#6587,.T.);
#8738=EDGE_CURVE('',#7258,#7258,#6588,.T.);
#8739=EDGE_CURVE('',#7258,#7259,#4317,.T.);
#8740=EDGE_CURVE('',#7259,#7259,#6589,.T.);
#8741=EDGE_CURVE('',#7260,#7260,#6590,.T.);
#8742=EDGE_CURVE('',#7260,#7261,#4318,.T.);
#8743=EDGE_CURVE('',#7261,#7261,#6591,.T.);
#8744=EDGE_CURVE('',#7262,#7262,#6592,.T.);
#8745=EDGE_CURVE('',#7262,#7263,#4319,.T.);
#8746=EDGE_CURVE('',#7263,#7263,#6593,.T.);
#8747=EDGE_CURVE('',#7264,#7264,#6594,.T.);
#8748=EDGE_CURVE('',#7264,#7265,#4320,.T.);
#8749=EDGE_CURVE('',#7265,#7265,#6595,.T.);
#8750=EDGE_CURVE('',#7266,#7266,#6596,.T.);
#8751=EDGE_CURVE('',#7266,#7267,#4321,.T.);
#8752=EDGE_CURVE('',#7267,#7267,#6597,.T.);
#8753=EDGE_CURVE('',#7268,#7268,#6598,.T.);
#8754=EDGE_CURVE('',#7268,#7269,#4322,.T.);
#8755=EDGE_CURVE('',#7269,#7269,#6599,.T.);
#8756=EDGE_CURVE('',#7270,#7270,#6600,.T.);
#8757=EDGE_CURVE('',#7270,#7271,#4323,.T.);
#8758=EDGE_CURVE('',#7271,#7271,#6601,.T.);
#8759=EDGE_CURVE('',#7272,#7272,#6602,.T.);
#8760=EDGE_CURVE('',#7272,#7273,#4324,.T.);
#8761=EDGE_CURVE('',#7273,#7273,#6603,.T.);
#8762=EDGE_CURVE('',#7274,#7274,#6604,.T.);
#8763=EDGE_CURVE('',#7274,#7275,#4325,.T.);
#8764=EDGE_CURVE('',#7275,#7275,#6605,.T.);
#8765=EDGE_CURVE('',#7276,#7277,#4326,.T.);
#8766=EDGE_CURVE('',#7276,#7278,#4327,.T.);
#8767=EDGE_CURVE('',#7279,#7278,#4328,.T.);
#8768=EDGE_CURVE('',#7277,#7279,#4329,.T.);
#8769=EDGE_CURVE('',#7277,#7280,#4330,.T.);
#8770=EDGE_CURVE('',#7280,#7281,#4331,.T.);
#8771=EDGE_CURVE('',#7281,#7276,#4332,.T.);
#8772=EDGE_CURVE('',#7282,#7283,#4333,.T.);
#8773=EDGE_CURVE('',#7283,#7284,#4334,.T.);
#8774=EDGE_CURVE('',#7285,#7284,#4335,.T.);
#8775=EDGE_CURVE('',#7282,#7285,#4336,.T.);
#8776=EDGE_CURVE('',#7281,#7282,#4337,.T.);
#8777=EDGE_CURVE('',#7286,#7285,#4338,.T.);
#8778=EDGE_CURVE('',#7278,#7286,#4339,.T.);
#8779=EDGE_CURVE('',#7287,#7286,#4340,.T.);
#8780=EDGE_CURVE('',#7279,#7287,#4341,.T.);
#8781=EDGE_CURVE('',#7283,#7280,#4342,.T.);
#8782=EDGE_CURVE('',#7284,#7287,#4343,.T.);
#8783=EDGE_CURVE('',#7288,#7288,#6606,.T.);
#8784=EDGE_CURVE('',#7288,#7289,#4344,.T.);
#8785=EDGE_CURVE('',#7289,#7289,#6607,.T.);
#8786=EDGE_CURVE('',#7290,#7290,#6608,.T.);
#8787=EDGE_CURVE('',#7290,#7291,#4345,.T.);
#8788=EDGE_CURVE('',#7291,#7291,#6609,.T.);
#8789=EDGE_CURVE('',#7292,#7292,#6610,.T.);
#8790=EDGE_CURVE('',#7292,#7293,#4346,.T.);
#8791=EDGE_CURVE('',#7293,#7293,#6611,.T.);
#8792=EDGE_CURVE('',#7294,#7294,#6612,.T.);
#8793=EDGE_CURVE('',#7294,#7295,#4347,.T.);
#8794=EDGE_CURVE('',#7295,#7295,#6613,.T.);
#8795=EDGE_CURVE('',#7296,#7296,#6614,.T.);
#8796=EDGE_CURVE('',#7296,#7297,#4348,.T.);
#8797=EDGE_CURVE('',#7297,#7297,#6615,.T.);
#8798=EDGE_CURVE('',#7298,#7298,#6616,.T.);
#8799=EDGE_CURVE('',#7298,#7299,#4349,.T.);
#8800=EDGE_CURVE('',#7299,#7299,#6617,.T.);
#8801=EDGE_CURVE('',#7300,#7300,#6618,.T.);
#8802=EDGE_CURVE('',#7300,#7301,#4350,.T.);
#8803=EDGE_CURVE('',#7301,#7301,#6619,.T.);
#8804=EDGE_CURVE('',#7302,#7302,#6620,.T.);
#8805=EDGE_CURVE('',#7302,#7303,#4351,.T.);
#8806=EDGE_CURVE('',#7303,#7303,#6621,.T.);
#8807=EDGE_CURVE('',#7304,#7304,#6622,.T.);
#8808=EDGE_CURVE('',#7304,#7305,#4352,.T.);
#8809=EDGE_CURVE('',#7305,#7305,#6623,.T.);
#8810=EDGE_CURVE('',#7306,#7306,#6624,.T.);
#8811=EDGE_CURVE('',#7306,#7307,#4353,.T.);
#8812=EDGE_CURVE('',#7307,#7307,#6625,.T.);
#8813=EDGE_CURVE('',#7308,#7308,#6626,.T.);
#8814=EDGE_CURVE('',#7308,#7309,#4354,.T.);
#8815=EDGE_CURVE('',#7309,#7309,#6627,.T.);
#8816=EDGE_CURVE('',#7310,#7310,#6628,.T.);
#8817=EDGE_CURVE('',#7310,#7311,#4355,.T.);
#8818=EDGE_CURVE('',#7311,#7311,#6629,.T.);
#8819=EDGE_CURVE('',#7312,#7312,#6630,.T.);
#8820=EDGE_CURVE('',#7313,#7313,#6631,.T.);
#8821=EDGE_CURVE('',#7313,#7312,#4356,.T.);
#8822=EDGE_CURVE('',#7314,#7314,#6632,.T.);
#8823=EDGE_CURVE('',#7314,#7315,#4357,.T.);
#8824=EDGE_CURVE('',#7315,#7315,#6633,.T.);
#8825=EDGE_CURVE('',#7316,#7316,#6634,.T.);
#8826=EDGE_CURVE('',#7316,#7317,#4358,.T.);
#8827=EDGE_CURVE('',#7317,#7317,#6635,.T.);
#8828=EDGE_CURVE('',#7318,#7318,#6636,.T.);
#8829=EDGE_CURVE('',#7318,#7319,#4359,.T.);
#8830=EDGE_CURVE('',#7319,#7319,#6637,.T.);
#8831=EDGE_CURVE('',#7320,#7320,#6638,.T.);
#8832=EDGE_CURVE('',#7320,#7321,#4360,.T.);
#8833=EDGE_CURVE('',#7321,#7321,#6639,.T.);
#8834=EDGE_CURVE('',#7322,#7322,#6640,.T.);
#8835=EDGE_CURVE('',#7322,#7323,#4361,.T.);
#8836=EDGE_CURVE('',#7323,#7323,#6641,.T.);
#8837=EDGE_CURVE('',#7324,#7324,#6642,.T.);
#8838=EDGE_CURVE('',#7324,#7325,#4362,.T.);
#8839=EDGE_CURVE('',#7325,#7325,#6643,.T.);
#8840=EDGE_CURVE('',#7326,#7326,#6644,.T.);
#8841=EDGE_CURVE('',#7326,#7327,#4363,.T.);
#8842=EDGE_CURVE('',#7327,#7327,#6645,.T.);
#8843=EDGE_CURVE('',#7328,#7328,#6646,.T.);
#8844=EDGE_CURVE('',#7328,#7329,#4364,.T.);
#8845=EDGE_CURVE('',#7329,#7329,#6647,.T.);
#8846=EDGE_CURVE('',#7330,#7330,#6648,.T.);
#8847=EDGE_CURVE('',#7330,#7331,#4365,.T.);
#8848=EDGE_CURVE('',#7331,#7331,#6649,.T.);
#8849=EDGE_CURVE('',#7332,#7332,#6650,.T.);
#8850=EDGE_CURVE('',#7332,#7333,#4366,.T.);
#8851=EDGE_CURVE('',#7333,#7333,#6651,.T.);
#8852=EDGE_CURVE('',#7334,#7334,#6652,.T.);
#8853=EDGE_CURVE('',#7334,#7335,#4367,.T.);
#8854=EDGE_CURVE('',#7335,#7335,#6653,.T.);
#8855=EDGE_CURVE('',#7336,#7336,#6654,.T.);
#8856=EDGE_CURVE('',#7336,#7337,#4368,.T.);
#8857=EDGE_CURVE('',#7337,#7337,#6655,.T.);
#8858=EDGE_CURVE('',#7338,#7338,#6656,.T.);
#8859=EDGE_CURVE('',#7338,#7339,#4369,.T.);
#8860=EDGE_CURVE('',#7339,#7339,#6657,.T.);
#8861=EDGE_CURVE('',#7340,#7340,#6658,.T.);
#8862=EDGE_CURVE('',#7341,#7341,#6659,.T.);
#8863=EDGE_CURVE('',#7341,#7340,#4370,.T.);
#8864=EDGE_CURVE('',#7342,#7342,#6660,.T.);
#8865=EDGE_CURVE('',#7342,#7343,#4371,.T.);
#8866=EDGE_CURVE('',#7343,#7343,#6661,.T.);
#8867=EDGE_CURVE('',#7344,#7345,#4372,.T.);
#8868=EDGE_CURVE('',#7345,#7346,#4373,.T.);
#8869=EDGE_CURVE('',#7346,#7347,#4374,.T.);
#8870=EDGE_CURVE('',#7344,#7347,#4375,.T.);
#8871=EDGE_CURVE('',#7345,#7348,#4376,.T.);
#8872=EDGE_CURVE('',#7348,#7349,#4377,.T.);
#8873=EDGE_CURVE('',#7349,#7346,#4378,.T.);
#8874=EDGE_CURVE('',#7348,#7350,#4379,.T.);
#8875=EDGE_CURVE('',#7350,#7351,#4380,.T.);
#8876=EDGE_CURVE('',#7351,#7349,#4381,.T.);
#8877=EDGE_CURVE('',#7350,#7352,#4382,.T.);
#8878=EDGE_CURVE('',#7352,#7353,#4383,.T.);
#8879=EDGE_CURVE('',#7353,#7351,#4384,.T.);
#8880=EDGE_CURVE('',#7352,#7354,#4385,.T.);
#8881=EDGE_CURVE('',#7354,#7355,#4386,.T.);
#8882=EDGE_CURVE('',#7355,#7353,#4387,.T.);
#8883=EDGE_CURVE('',#7354,#7344,#4388,.T.);
#8884=EDGE_CURVE('',#7347,#7355,#4389,.T.);
#8885=EDGE_CURVE('',#7356,#7356,#6662,.T.);
#8886=EDGE_CURVE('',#7357,#7357,#6663,.T.);
#8887=EDGE_CURVE('',#7358,#7358,#6664,.T.);
#8888=EDGE_CURVE('',#7358,#7357,#4390,.T.);
#8889=EDGE_CURVE('',#7359,#7359,#6665,.T.);
#8890=EDGE_CURVE('',#7359,#7358,#4391,.T.);
#8891=EDGE_CURVE('',#7360,#7360,#6666,.T.);
#8892=EDGE_CURVE('',#7360,#7359,#4392,.T.);
#8893=EDGE_CURVE('',#7361,#7361,#6667,.T.);
#8894=EDGE_CURVE('',#7362,#7362,#6668,.F.);
#8895=EDGE_CURVE('',#7362,#7361,#4393,.T.);
#8896=EDGE_CURVE('',#7356,#7362,#4394,.T.);
#8897=EDGE_CURVE('',#7363,#7363,#6669,.T.);
#8898=EDGE_CURVE('',#7363,#7364,#4395,.T.);
#8899=EDGE_CURVE('',#7364,#7364,#6670,.T.);
#8900=EDGE_CURVE('',#7365,#7365,#6671,.T.);
#8901=EDGE_CURVE('',#7365,#7366,#4396,.T.);
#8902=EDGE_CURVE('',#7366,#7366,#6672,.T.);
#8903=EDGE_CURVE('',#7367,#7367,#6673,.T.);
#8904=EDGE_CURVE('',#7367,#7368,#4397,.T.);
#8905=EDGE_CURVE('',#7368,#7368,#6674,.T.);
#8906=EDGE_CURVE('',#7369,#7369,#6675,.T.);
#8907=EDGE_CURVE('',#7369,#7370,#4398,.T.);
#8908=EDGE_CURVE('',#7370,#7370,#6676,.T.);
#8909=EDGE_CURVE('',#7371,#7371,#6677,.T.);
#8910=EDGE_CURVE('',#7371,#7372,#4399,.T.);
#8911=EDGE_CURVE('',#7372,#7372,#6678,.T.);
#8912=EDGE_CURVE('',#7373,#7373,#6679,.T.);
#8913=EDGE_CURVE('',#7373,#7374,#4400,.T.);
#8914=EDGE_CURVE('',#7374,#7374,#6680,.T.);
#8915=EDGE_CURVE('',#7375,#7375,#6681,.T.);
#8916=EDGE_CURVE('',#7375,#7376,#4401,.T.);
#8917=EDGE_CURVE('',#7376,#7376,#6682,.T.);
#8918=EDGE_CURVE('',#7377,#7377,#6683,.T.);
#8919=EDGE_CURVE('',#7377,#7378,#4402,.T.);
#8920=EDGE_CURVE('',#7378,#7378,#6684,.T.);
#8921=EDGE_CURVE('',#7379,#7379,#6685,.T.);
#8922=EDGE_CURVE('',#7379,#7380,#4403,.T.);
#8923=EDGE_CURVE('',#7380,#7380,#6686,.T.);
#8924=EDGE_CURVE('',#7381,#7381,#6687,.T.);
#8925=EDGE_CURVE('',#7381,#7382,#4404,.T.);
#8926=EDGE_CURVE('',#7382,#7382,#6688,.T.);
#8927=EDGE_CURVE('',#7383,#7383,#6689,.T.);
#8928=EDGE_CURVE('',#7383,#7384,#4405,.T.);
#8929=EDGE_CURVE('',#7384,#7384,#6690,.T.);
#8930=EDGE_CURVE('',#7385,#7385,#6691,.T.);
#8931=EDGE_CURVE('',#7385,#7386,#4406,.T.);
#8932=EDGE_CURVE('',#7386,#7386,#6692,.T.);
#8933=EDGE_CURVE('',#7387,#7387,#6693,.T.);
#8934=EDGE_CURVE('',#7388,#7388,#6694,.T.);
#8935=EDGE_CURVE('',#7388,#7387,#4407,.T.);
#8936=EDGE_CURVE('',#7389,#7389,#6695,.T.);
#8937=EDGE_CURVE('',#7389,#7390,#4408,.T.);
#8938=EDGE_CURVE('',#7390,#7390,#6696,.T.);
#8939=EDGE_CURVE('',#7391,#7391,#6697,.T.);
#8940=EDGE_CURVE('',#7391,#7392,#4409,.T.);
#8941=EDGE_CURVE('',#7392,#7392,#6698,.T.);
#8942=EDGE_CURVE('',#7393,#7393,#6699,.T.);
#8943=EDGE_CURVE('',#7393,#7394,#4410,.T.);
#8944=EDGE_CURVE('',#7394,#7394,#6700,.T.);
#8945=EDGE_CURVE('',#7395,#7395,#6701,.T.);
#8946=EDGE_CURVE('',#7395,#7396,#4411,.T.);
#8947=EDGE_CURVE('',#7396,#7396,#6702,.T.);
#8948=EDGE_CURVE('',#7397,#7397,#6703,.T.);
#8949=EDGE_CURVE('',#7397,#7398,#4412,.T.);
#8950=EDGE_CURVE('',#7398,#7398,#6704,.T.);
#8951=EDGE_CURVE('',#7399,#7399,#6705,.T.);
#8952=EDGE_CURVE('',#7399,#7400,#4413,.T.);
#8953=EDGE_CURVE('',#7400,#7400,#6706,.T.);
#8954=EDGE_CURVE('',#7401,#7401,#6707,.T.);
#8955=EDGE_CURVE('',#7401,#7402,#4414,.T.);
#8956=EDGE_CURVE('',#7402,#7402,#6708,.T.);
#8957=EDGE_CURVE('',#7403,#7403,#6709,.T.);
#8958=EDGE_CURVE('',#7403,#7404,#4415,.T.);
#8959=EDGE_CURVE('',#7404,#7404,#6710,.T.);
#8960=EDGE_CURVE('',#7405,#7405,#6711,.T.);
#8961=EDGE_CURVE('',#7405,#7406,#4416,.T.);
#8962=EDGE_CURVE('',#7406,#7406,#6712,.T.);
#8963=EDGE_CURVE('',#7407,#7407,#6713,.T.);
#8964=EDGE_CURVE('',#7407,#7408,#4417,.T.);
#8965=EDGE_CURVE('',#7408,#7408,#6714,.T.);
#8966=EDGE_CURVE('',#7409,#7409,#6715,.T.);
#8967=EDGE_CURVE('',#7409,#7410,#4418,.T.);
#8968=EDGE_CURVE('',#7410,#7410,#6716,.T.);
#8969=EDGE_CURVE('',#7411,#7411,#6717,.T.);
#8970=EDGE_CURVE('',#7411,#7412,#4419,.T.);
#8971=EDGE_CURVE('',#7412,#7412,#6718,.T.);
#8972=EDGE_CURVE('',#7413,#7413,#6719,.T.);
#8973=EDGE_CURVE('',#7413,#7414,#4420,.T.);
#8974=EDGE_CURVE('',#7414,#7414,#6720,.T.);
#8975=EDGE_CURVE('',#7415,#7415,#6721,.T.);
#8976=EDGE_CURVE('',#7416,#7416,#6722,.T.);
#8977=EDGE_CURVE('',#7416,#7415,#4421,.T.);
#8978=EDGE_CURVE('',#7417,#7417,#6723,.T.);
#8979=EDGE_CURVE('',#7417,#7418,#4422,.T.);
#8980=EDGE_CURVE('',#7418,#7418,#6724,.T.);
#8981=EDGE_CURVE('',#7419,#7420,#6725,.T.);
#8982=EDGE_CURVE('',#7420,#7419,#6726,.T.);
#8983=EDGE_CURVE('',#7420,#7421,#6727,.T.);
#8984=EDGE_CURVE('',#7422,#7421,#6728,.T.);
#8985=EDGE_CURVE('',#7421,#7422,#6729,.T.);
#8986=EDGE_CURVE('',#7422,#7423,#4423,.T.);
#8987=EDGE_CURVE('',#7423,#7423,#6730,.T.);
#8988=EDGE_CURVE('',#7424,#7424,#6731,.T.);
#8989=EDGE_CURVE('',#7424,#7425,#4424,.T.);
#8990=EDGE_CURVE('',#7425,#7425,#6732,.T.);
#8991=EDGE_CURVE('',#7425,#7426,#4425,.T.);
#8992=EDGE_CURVE('',#7426,#7426,#6733,.T.);
#8993=EDGE_CURVE('',#7427,#7427,#6734,.T.);
#8994=EDGE_CURVE('',#7427,#7419,#4426,.T.);
#8995=EDGE_CURVE('',#7428,#7428,#6735,.T.);
#8996=EDGE_CURVE('',#7428,#7424,#4427,.T.);
#8997=EDGE_CURVE('',#7429,#7430,#6736,.T.);
#8998=EDGE_CURVE('',#7430,#7429,#6737,.T.);
#8999=EDGE_CURVE('',#7430,#7431,#6738,.T.);
#9000=EDGE_CURVE('',#7432,#7431,#6739,.T.);
#9001=EDGE_CURVE('',#7431,#7432,#6740,.T.);
#9002=EDGE_CURVE('',#7433,#7433,#6741,.T.);
#9003=EDGE_CURVE('',#7433,#7432,#4428,.T.);
#9004=EDGE_CURVE('',#7434,#7434,#6742,.T.);
#9005=EDGE_CURVE('',#7435,#7435,#6743,.T.);
#9006=EDGE_CURVE('',#7436,#7436,#6744,.T.);
#9007=EDGE_CURVE('',#7436,#7434,#4429,.T.);
#9008=EDGE_CURVE('',#7437,#7437,#6745,.T.);
#9009=EDGE_CURVE('',#7437,#7436,#4430,.T.);
#9010=EDGE_CURVE('',#7438,#7438,#6746,.T.);
#9011=EDGE_CURVE('',#7438,#7437,#4431,.T.);
#9012=EDGE_CURVE('',#7429,#7435,#4432,.T.);
#9013=EDGE_CURVE('',#7439,#7440,#6747,.T.);
#9014=EDGE_CURVE('',#7441,#7442,#6748,.T.);
#9015=EDGE_CURVE('',#7443,#7444,#6749,.T.);
#9016=EDGE_CURVE('',#7445,#7446,#6750,.T.);
#9017=EDGE_CURVE('',#7447,#7448,#6751,.T.);
#9018=EDGE_CURVE('',#7449,#7450,#6752,.T.);
#9019=EDGE_CURVE('',#7451,#7452,#6753,.T.);
#9020=EDGE_CURVE('',#7453,#7454,#859,.T.);
#9021=EDGE_CURVE('',#7455,#7453,#6754,.T.);
#9022=EDGE_CURVE('',#7456,#7455,#860,.T.);
#9023=EDGE_CURVE('',#7454,#7456,#6755,.T.);
#9024=EDGE_CURVE('',#7457,#7455,#6756,.T.);
#9025=EDGE_CURVE('',#7457,#7458,#861,.T.);
#9026=EDGE_CURVE('',#7459,#7458,#6757,.T.);
#9027=EDGE_CURVE('',#7459,#7460,#862,.T.);
#9028=EDGE_CURVE('',#7461,#7460,#6758,.T.);
#9029=EDGE_CURVE('',#7461,#7462,#4433,.T.);
#9030=EDGE_CURVE('',#7462,#7462,#6759,.T.);
#9031=EDGE_CURVE('',#7463,#7461,#6760,.T.);
#9032=EDGE_CURVE('',#7463,#7464,#863,.T.);
#9033=EDGE_CURVE('',#7465,#7464,#6761,.T.);
#9034=EDGE_CURVE('',#7465,#7466,#864,.T.);
#9035=EDGE_CURVE('',#7467,#7466,#6762,.T.);
#9036=EDGE_CURVE('',#7467,#7468,#865,.T.);
#9037=EDGE_CURVE('',#7469,#7468,#6763,.T.);
#9038=EDGE_CURVE('',#7469,#7470,#866,.T.);
#9039=EDGE_CURVE('',#7456,#7470,#6764,.T.);
#9040=EDGE_CURVE('',#7453,#7471,#6765,.T.);
#9041=EDGE_CURVE('',#7471,#7457,#6766,.T.);
#9042=EDGE_CURVE('',#7472,#7471,#867,.T.);
#9043=EDGE_CURVE('',#7458,#7472,#6767,.T.);
#9044=EDGE_CURVE('',#7472,#7473,#6768,.T.);
#9045=EDGE_CURVE('',#7473,#7459,#6769,.T.);
#9046=EDGE_CURVE('',#7474,#7473,#868,.T.);
#9047=EDGE_CURVE('',#7460,#7474,#6770,.T.);
#9048=EDGE_CURVE('',#7474,#7475,#6771,.T.);
#9049=EDGE_CURVE('',#7475,#7476,#6772,.T.);
#9050=EDGE_CURVE('',#7476,#7463,#6773,.T.);
#9051=EDGE_CURVE('',#7477,#7476,#869,.T.);
#9052=EDGE_CURVE('',#7464,#7477,#6774,.T.);
#9053=EDGE_CURVE('',#7477,#7478,#6775,.T.);
#9054=EDGE_CURVE('',#7478,#7465,#6776,.T.);
#9055=EDGE_CURVE('',#7479,#7478,#870,.T.);
#9056=EDGE_CURVE('',#7466,#7479,#6777,.T.);
#9057=EDGE_CURVE('',#7479,#7480,#6778,.T.);
#9058=EDGE_CURVE('',#7480,#7467,#6779,.T.);
#9059=EDGE_CURVE('',#7481,#7480,#871,.T.);
#9060=EDGE_CURVE('',#7468,#7481,#6780,.T.);
#9061=EDGE_CURVE('',#7482,#7482,#6781,.T.);
#9062=EDGE_CURVE('',#7482,#7475,#4434,.T.);
#9063=EDGE_CURVE('',#7483,#7454,#6782,.T.);
#9064=EDGE_CURVE('',#7483,#7484,#872,.T.);
#9065=EDGE_CURVE('',#7481,#7484,#6783,.T.);
#9066=EDGE_CURVE('',#7470,#7483,#6784,.T.);
#9067=EDGE_CURVE('',#7484,#7469,#6785,.T.);
#9068=EDGE_CURVE('',#7485,#7485,#6786,.T.);
#9069=EDGE_CURVE('',#7486,#7486,#6787,.T.);
#9070=EDGE_CURVE('',#7487,#7487,#6788,.T.);
#9071=EDGE_CURVE('',#7487,#7485,#4435,.T.);
#9072=EDGE_CURVE('',#7488,#7488,#6789,.T.);
#9073=EDGE_CURVE('',#7488,#7486,#4436,.T.);
#9074=EDGE_CURVE('',#7489,#7489,#6790,.T.);
#9075=EDGE_CURVE('',#7490,#7490,#6791,.T.);
#9076=EDGE_CURVE('',#7491,#7491,#6792,.T.);
#9077=EDGE_CURVE('',#7491,#7489,#4437,.T.);
#9078=EDGE_CURVE('',#7492,#7492,#6793,.T.);
#9079=EDGE_CURVE('',#7492,#7490,#4438,.T.);
#9080=EDGE_CURVE('',#7493,#7494,#6794,.T.);
#9081=EDGE_CURVE('',#7494,#7493,#6795,.T.);
#9082=EDGE_CURVE('',#7494,#7495,#6796,.T.);
#9083=EDGE_CURVE('',#7496,#7495,#6797,.T.);
#9084=EDGE_CURVE('',#7495,#7496,#6798,.T.);
#9085=EDGE_CURVE('',#7496,#7497,#4439,.T.);
#9086=EDGE_CURVE('',#7497,#7497,#6799,.T.);
#9087=EDGE_CURVE('',#7498,#7498,#6800,.T.);
#9088=EDGE_CURVE('',#7498,#7499,#4440,.T.);
#9089=EDGE_CURVE('',#7499,#7499,#6801,.T.);
#9090=EDGE_CURVE('',#7499,#7500,#4441,.T.);
#9091=EDGE_CURVE('',#7500,#7500,#6802,.T.);
#9092=EDGE_CURVE('',#7501,#7501,#6803,.T.);
#9093=EDGE_CURVE('',#7501,#7493,#4442,.T.);
#9094=EDGE_CURVE('',#7502,#7502,#6804,.T.);
#9095=EDGE_CURVE('',#7502,#7498,#4443,.T.);
#9096=EDGE_CURVE('',#7503,#7504,#6805,.T.);
#9097=EDGE_CURVE('',#7504,#7503,#6806,.T.);
#9098=EDGE_CURVE('',#7504,#7505,#6807,.T.);
#9099=EDGE_CURVE('',#7506,#7505,#6808,.T.);
#9100=EDGE_CURVE('',#7505,#7506,#6809,.T.);
#9101=EDGE_CURVE('',#7507,#7507,#6810,.T.);
#9102=EDGE_CURVE('',#7507,#7506,#4444,.T.);
#9103=EDGE_CURVE('',#7508,#7508,#6811,.T.);
#9104=EDGE_CURVE('',#7509,#7509,#6812,.T.);
#9105=EDGE_CURVE('',#7510,#7510,#6813,.T.);
#9106=EDGE_CURVE('',#7510,#7508,#4445,.T.);
#9107=EDGE_CURVE('',#7511,#7511,#6814,.T.);
#9108=EDGE_CURVE('',#7511,#7510,#4446,.T.);
#9109=EDGE_CURVE('',#7512,#7512,#6815,.T.);
#9110=EDGE_CURVE('',#7512,#7511,#4447,.T.);
#9111=EDGE_CURVE('',#7503,#7509,#4448,.T.);
#9112=EDGE_CURVE('',#7513,#7514,#6816,.T.);
#9113=EDGE_CURVE('',#7515,#7516,#6817,.T.);
#9114=EDGE_CURVE('',#7517,#7518,#6818,.T.);
#9115=EDGE_CURVE('',#7519,#7520,#6819,.T.);
#9116=EDGE_CURVE('',#7521,#7522,#6820,.T.);
#9117=EDGE_CURVE('',#7523,#7524,#6821,.T.);
#9118=EDGE_CURVE('',#7525,#7526,#6822,.T.);
#9119=EDGE_CURVE('',#7527,#7528,#6823,.T.);
#9120=EDGE_CURVE('',#7529,#7530,#873,.T.);
#9121=EDGE_CURVE('',#7531,#7529,#6824,.T.);
#9122=EDGE_CURVE('',#7532,#7531,#874,.T.);
#9123=EDGE_CURVE('',#7530,#7532,#6825,.T.);
#9124=EDGE_CURVE('',#7533,#7531,#6826,.T.);
#9125=EDGE_CURVE('',#7533,#7534,#875,.T.);
#9126=EDGE_CURVE('',#7535,#7534,#6827,.T.);
#9127=EDGE_CURVE('',#7535,#7536,#876,.T.);
#9128=EDGE_CURVE('',#7537,#7536,#6828,.T.);
#9129=EDGE_CURVE('',#7537,#7538,#877,.T.);
#9130=EDGE_CURVE('',#7538,#7539,#4449,.T.);
#9131=EDGE_CURVE('',#7539,#7539,#6829,.T.);
#9132=EDGE_CURVE('',#7538,#7540,#878,.T.);
#9133=EDGE_CURVE('',#7541,#7540,#6830,.T.);
#9134=EDGE_CURVE('',#7541,#7542,#879,.T.);
#9135=EDGE_CURVE('',#7543,#7542,#6831,.T.);
#9136=EDGE_CURVE('',#7543,#7544,#880,.T.);
#9137=EDGE_CURVE('',#7545,#7544,#6832,.T.);
#9138=EDGE_CURVE('',#7545,#7546,#881,.T.);
#9139=EDGE_CURVE('',#7547,#7546,#6833,.T.);
#9140=EDGE_CURVE('',#7547,#7548,#882,.T.);
#9141=EDGE_CURVE('',#7532,#7548,#6834,.T.);
#9142=EDGE_CURVE('',#7529,#7549,#6835,.T.);
#9143=EDGE_CURVE('',#7549,#7533,#6836,.T.);
#9144=EDGE_CURVE('',#7550,#7549,#883,.T.);
#9145=EDGE_CURVE('',#7534,#7550,#6837,.T.);
#9146=EDGE_CURVE('',#7550,#7551,#6838,.T.);
#9147=EDGE_CURVE('',#7551,#7535,#6839,.T.);
#9148=EDGE_CURVE('',#7552,#7551,#884,.T.);
#9149=EDGE_CURVE('',#7536,#7552,#6840,.T.);
#9150=EDGE_CURVE('',#7552,#7553,#6841,.T.);
#9151=EDGE_CURVE('',#7553,#7537,#6842,.T.);
#9152=EDGE_CURVE('',#7554,#7555,#885,.T.);
#9153=EDGE_CURVE('',#7540,#7554,#6843,.T.);
#9154=EDGE_CURVE('',#7555,#7553,#886,.T.);
#9155=EDGE_CURVE('',#7554,#7556,#6844,.T.);
#9156=EDGE_CURVE('',#7556,#7541,#6845,.T.);
#9157=EDGE_CURVE('',#7557,#7556,#887,.T.);
#9158=EDGE_CURVE('',#7542,#7557,#6846,.T.);
#9159=EDGE_CURVE('',#7557,#7558,#6847,.T.);
#9160=EDGE_CURVE('',#7558,#7543,#6848,.T.);
#9161=EDGE_CURVE('',#7559,#7558,#888,.T.);
#9162=EDGE_CURVE('',#7544,#7559,#6849,.T.);
#9163=EDGE_CURVE('',#7559,#7560,#6850,.T.);
#9164=EDGE_CURVE('',#7560,#7545,#6851,.T.);
#9165=EDGE_CURVE('',#7561,#7560,#889,.T.);
#9166=EDGE_CURVE('',#7546,#7561,#6852,.T.);
#9167=EDGE_CURVE('',#7562,#7562,#6853,.T.);
#9168=EDGE_CURVE('',#7562,#7555,#4450,.T.);
#9169=EDGE_CURVE('',#7563,#7530,#6854,.T.);
#9170=EDGE_CURVE('',#7563,#7564,#890,.T.);
#9171=EDGE_CURVE('',#7561,#7564,#6855,.T.);
#9172=EDGE_CURVE('',#7548,#7563,#6856,.T.);
#9173=EDGE_CURVE('',#7564,#7547,#6857,.T.);
#9174=EDGE_CURVE('',#7565,#7565,#6858,.T.);
#9175=EDGE_CURVE('',#7566,#7566,#6859,.T.);
#9176=EDGE_CURVE('',#7567,#7567,#6860,.T.);
#9177=EDGE_CURVE('',#7567,#7565,#4451,.T.);
#9178=EDGE_CURVE('',#7568,#7568,#6861,.T.);
#9179=EDGE_CURVE('',#7568,#7566,#4452,.T.);
#9180=EDGE_CURVE('',#7569,#7569,#6862,.T.);
#9181=EDGE_CURVE('',#7570,#7570,#6863,.T.);
#9182=EDGE_CURVE('',#7571,#7571,#6864,.T.);
#9183=EDGE_CURVE('',#7571,#7569,#4453,.T.);
#9184=EDGE_CURVE('',#7572,#7572,#6865,.T.);
#9185=EDGE_CURVE('',#7572,#7570,#4454,.T.);
#9186=EDGE_CURVE('',#7573,#7574,#4455,.T.);
#9187=EDGE_CURVE('',#7574,#7575,#4456,.T.);
#9188=EDGE_CURVE('',#7575,#7576,#4457,.T.);
#9189=EDGE_CURVE('',#7573,#7576,#4458,.T.);
#9190=EDGE_CURVE('',#7574,#7577,#4459,.T.);
#9191=EDGE_CURVE('',#7577,#7578,#4460,.T.);
#9192=EDGE_CURVE('',#7578,#7575,#4461,.T.);
#9193=EDGE_CURVE('',#7577,#7579,#4462,.T.);
#9194=EDGE_CURVE('',#7579,#7580,#4463,.T.);
#9195=EDGE_CURVE('',#7580,#7578,#4464,.T.);
#9196=EDGE_CURVE('',#7579,#7581,#4465,.T.);
#9197=EDGE_CURVE('',#7581,#7582,#4466,.T.);
#9198=EDGE_CURVE('',#7582,#7580,#4467,.T.);
#9199=EDGE_CURVE('',#7581,#7583,#4468,.T.);
#9200=EDGE_CURVE('',#7583,#7584,#4469,.T.);
#9201=EDGE_CURVE('',#7584,#7582,#4470,.T.);
#9202=EDGE_CURVE('',#7583,#7573,#4471,.T.);
#9203=EDGE_CURVE('',#7576,#7584,#4472,.T.);
#9204=EDGE_CURVE('',#7585,#7585,#6866,.T.);
#9205=EDGE_CURVE('',#7586,#7586,#6867,.T.);
#9206=EDGE_CURVE('',#7587,#7587,#6868,.T.);
#9207=EDGE_CURVE('',#7587,#7586,#4473,.T.);
#9208=EDGE_CURVE('',#7588,#7588,#6869,.T.);
#9209=EDGE_CURVE('',#7588,#7587,#4474,.T.);
#9210=EDGE_CURVE('',#7589,#7589,#6870,.T.);
#9211=EDGE_CURVE('',#7589,#7588,#4475,.T.);
#9212=EDGE_CURVE('',#7590,#7590,#6871,.T.);
#9213=EDGE_CURVE('',#7591,#7591,#6872,.F.);
#9214=EDGE_CURVE('',#7591,#7590,#4476,.T.);
#9215=EDGE_CURVE('',#7585,#7591,#4477,.T.);
#9216=EDGE_CURVE('',#7592,#7593,#4478,.T.);
#9217=EDGE_CURVE('',#7594,#7592,#4479,.T.);
#9218=EDGE_CURVE('',#7594,#7595,#4480,.T.);
#9219=EDGE_CURVE('',#7595,#7593,#4481,.T.);
#9220=EDGE_CURVE('',#7593,#7596,#4482,.T.);
#9221=EDGE_CURVE('',#7595,#7597,#4483,.T.);
#9222=EDGE_CURVE('',#7597,#7596,#4484,.T.);
#9223=EDGE_CURVE('',#7596,#7598,#4485,.T.);
#9224=EDGE_CURVE('',#7597,#7599,#4486,.T.);
#9225=EDGE_CURVE('',#7599,#7598,#4487,.T.);
#9226=EDGE_CURVE('',#7598,#7592,#4488,.T.);
#9227=EDGE_CURVE('',#7599,#7594,#4489,.T.);
#9228=EDGE_CURVE('',#7600,#7601,#4490,.T.);
#9229=EDGE_CURVE('',#7602,#7600,#4491,.T.);
#9230=EDGE_CURVE('',#7602,#7603,#4492,.T.);
#9231=EDGE_CURVE('',#7603,#7601,#4493,.T.);
#9232=EDGE_CURVE('',#7601,#7604,#4494,.T.);
#9233=EDGE_CURVE('',#7603,#7605,#4495,.T.);
#9234=EDGE_CURVE('',#7605,#7604,#4496,.T.);
#9235=EDGE_CURVE('',#7604,#7606,#4497,.T.);
#9236=EDGE_CURVE('',#7605,#7607,#4498,.T.);
#9237=EDGE_CURVE('',#7607,#7606,#4499,.T.);
#9238=EDGE_CURVE('',#7606,#7600,#4500,.T.);
#9239=EDGE_CURVE('',#7607,#7602,#4501,.T.);
#9240=EDGE_CURVE('',#7608,#7609,#4502,.T.);
#9241=EDGE_CURVE('',#7610,#7608,#4503,.T.);
#9242=EDGE_CURVE('',#7610,#7611,#4504,.T.);
#9243=EDGE_CURVE('',#7611,#7609,#4505,.T.);
#9244=EDGE_CURVE('',#7609,#7612,#4506,.T.);
#9245=EDGE_CURVE('',#7611,#7613,#4507,.T.);
#9246=EDGE_CURVE('',#7613,#7612,#4508,.T.);
#9247=EDGE_CURVE('',#7612,#7614,#4509,.T.);
#9248=EDGE_CURVE('',#7613,#7615,#4510,.T.);
#9249=EDGE_CURVE('',#7615,#7614,#4511,.T.);
#9250=EDGE_CURVE('',#7614,#7608,#4512,.T.);
#9251=EDGE_CURVE('',#7615,#7610,#4513,.T.);
#9252=EDGE_CURVE('',#7616,#7617,#4514,.T.);
#9253=EDGE_CURVE('',#7618,#7616,#4515,.T.);
#9254=EDGE_CURVE('',#7618,#7619,#4516,.T.);
#9255=EDGE_CURVE('',#7619,#7617,#4517,.T.);
#9256=EDGE_CURVE('',#7617,#7620,#4518,.T.);
#9257=EDGE_CURVE('',#7619,#7621,#4519,.T.);
#9258=EDGE_CURVE('',#7621,#7620,#4520,.T.);
#9259=EDGE_CURVE('',#7620,#7622,#4521,.T.);
#9260=EDGE_CURVE('',#7621,#7623,#4522,.T.);
#9261=EDGE_CURVE('',#7623,#7622,#4523,.T.);
#9262=EDGE_CURVE('',#7622,#7616,#4524,.T.);
#9263=EDGE_CURVE('',#7623,#7618,#4525,.T.);
#9264=EDGE_CURVE('',#7624,#7625,#4526,.T.);
#9265=EDGE_CURVE('',#7626,#7624,#4527,.T.);
#9266=EDGE_CURVE('',#7626,#7627,#4528,.T.);
#9267=EDGE_CURVE('',#7627,#7625,#4529,.T.);
#9268=EDGE_CURVE('',#7625,#7628,#4530,.T.);
#9269=EDGE_CURVE('',#7627,#7629,#4531,.T.);
#9270=EDGE_CURVE('',#7629,#7628,#4532,.T.);
#9271=EDGE_CURVE('',#7628,#7630,#4533,.T.);
#9272=EDGE_CURVE('',#7629,#7631,#4534,.T.);
#9273=EDGE_CURVE('',#7631,#7630,#4535,.T.);
#9274=EDGE_CURVE('',#7630,#7624,#4536,.T.);
#9275=EDGE_CURVE('',#7631,#7626,#4537,.T.);
#9276=EDGE_CURVE('',#7632,#7633,#4538,.T.);
#9277=EDGE_CURVE('',#7634,#7632,#4539,.T.);
#9278=EDGE_CURVE('',#7634,#7635,#4540,.T.);
#9279=EDGE_CURVE('',#7635,#7633,#4541,.T.);
#9280=EDGE_CURVE('',#7633,#7636,#4542,.T.);
#9281=EDGE_CURVE('',#7635,#7637,#4543,.T.);
#9282=EDGE_CURVE('',#7637,#7636,#4544,.T.);
#9283=EDGE_CURVE('',#7636,#7638,#4545,.T.);
#9284=EDGE_CURVE('',#7637,#7639,#4546,.T.);
#9285=EDGE_CURVE('',#7639,#7638,#4547,.T.);
#9286=EDGE_CURVE('',#7638,#7632,#4548,.T.);
#9287=EDGE_CURVE('',#7639,#7634,#4549,.T.);
#9288=EDGE_CURVE('',#7640,#7641,#4550,.T.);
#9289=EDGE_CURVE('',#7642,#7640,#4551,.T.);
#9290=EDGE_CURVE('',#7642,#7643,#4552,.T.);
#9291=EDGE_CURVE('',#7643,#7641,#4553,.T.);
#9292=EDGE_CURVE('',#7641,#7644,#4554,.T.);
#9293=EDGE_CURVE('',#7643,#7645,#4555,.T.);
#9294=EDGE_CURVE('',#7645,#7644,#4556,.T.);
#9295=EDGE_CURVE('',#7644,#7646,#4557,.T.);
#9296=EDGE_CURVE('',#7645,#7647,#4558,.T.);
#9297=EDGE_CURVE('',#7647,#7646,#4559,.T.);
#9298=EDGE_CURVE('',#7646,#7640,#4560,.T.);
#9299=EDGE_CURVE('',#7647,#7642,#4561,.T.);
#9300=EDGE_CURVE('',#7648,#7649,#4562,.T.);
#9301=EDGE_CURVE('',#7650,#7648,#4563,.T.);
#9302=EDGE_CURVE('',#7650,#7651,#4564,.T.);
#9303=EDGE_CURVE('',#7651,#7649,#4565,.T.);
#9304=EDGE_CURVE('',#7649,#7652,#4566,.T.);
#9305=EDGE_CURVE('',#7651,#7653,#4567,.T.);
#9306=EDGE_CURVE('',#7653,#7652,#4568,.T.);
#9307=EDGE_CURVE('',#7652,#7654,#4569,.T.);
#9308=EDGE_CURVE('',#7653,#7655,#4570,.T.);
#9309=EDGE_CURVE('',#7655,#7654,#4571,.T.);
#9310=EDGE_CURVE('',#7654,#7648,#4572,.T.);
#9311=EDGE_CURVE('',#7655,#7650,#4573,.T.);
#9312=EDGE_CURVE('',#7656,#7657,#4574,.T.);
#9313=EDGE_CURVE('',#7658,#7656,#4575,.T.);
#9314=EDGE_CURVE('',#7658,#7659,#4576,.T.);
#9315=EDGE_CURVE('',#7659,#7657,#4577,.T.);
#9316=EDGE_CURVE('',#7657,#7660,#4578,.T.);
#9317=EDGE_CURVE('',#7659,#7661,#4579,.T.);
#9318=EDGE_CURVE('',#7661,#7660,#4580,.T.);
#9319=EDGE_CURVE('',#7660,#7662,#4581,.T.);
#9320=EDGE_CURVE('',#7661,#7663,#4582,.T.);
#9321=EDGE_CURVE('',#7663,#7662,#4583,.T.);
#9322=EDGE_CURVE('',#7662,#7656,#4584,.T.);
#9323=EDGE_CURVE('',#7663,#7658,#4585,.T.);
#9324=EDGE_CURVE('',#7664,#7665,#4586,.T.);
#9325=EDGE_CURVE('',#7666,#7664,#4587,.T.);
#9326=EDGE_CURVE('',#7666,#7667,#4588,.T.);
#9327=EDGE_CURVE('',#7667,#7665,#4589,.T.);
#9328=EDGE_CURVE('',#7665,#7668,#4590,.T.);
#9329=EDGE_CURVE('',#7667,#7669,#4591,.T.);
#9330=EDGE_CURVE('',#7669,#7668,#4592,.T.);
#9331=EDGE_CURVE('',#7668,#7670,#4593,.T.);
#9332=EDGE_CURVE('',#7669,#7671,#4594,.T.);
#9333=EDGE_CURVE('',#7671,#7670,#4595,.T.);
#9334=EDGE_CURVE('',#7670,#7664,#4596,.T.);
#9335=EDGE_CURVE('',#7671,#7666,#4597,.T.);
#9336=EDGE_CURVE('',#7672,#7673,#4598,.T.);
#9337=EDGE_CURVE('',#7674,#7672,#4599,.T.);
#9338=EDGE_CURVE('',#7674,#7675,#4600,.T.);
#9339=EDGE_CURVE('',#7675,#7673,#4601,.T.);
#9340=EDGE_CURVE('',#7673,#7676,#4602,.T.);
#9341=EDGE_CURVE('',#7675,#7677,#4603,.T.);
#9342=EDGE_CURVE('',#7677,#7676,#4604,.T.);
#9343=EDGE_CURVE('',#7676,#7678,#4605,.T.);
#9344=EDGE_CURVE('',#7677,#7679,#4606,.T.);
#9345=EDGE_CURVE('',#7679,#7678,#4607,.T.);
#9346=EDGE_CURVE('',#7678,#7672,#4608,.T.);
#9347=EDGE_CURVE('',#7679,#7674,#4609,.T.);
#9348=EDGE_CURVE('',#7680,#7681,#4610,.T.);
#9349=EDGE_CURVE('',#7682,#7680,#4611,.T.);
#9350=EDGE_CURVE('',#7682,#7683,#4612,.T.);
#9351=EDGE_CURVE('',#7683,#7681,#4613,.T.);
#9352=EDGE_CURVE('',#7681,#7684,#4614,.T.);
#9353=EDGE_CURVE('',#7683,#7685,#4615,.T.);
#9354=EDGE_CURVE('',#7685,#7684,#4616,.T.);
#9355=EDGE_CURVE('',#7684,#7686,#4617,.T.);
#9356=EDGE_CURVE('',#7685,#7687,#4618,.T.);
#9357=EDGE_CURVE('',#7687,#7686,#4619,.T.);
#9358=EDGE_CURVE('',#7686,#7680,#4620,.T.);
#9359=EDGE_CURVE('',#7687,#7682,#4621,.T.);
#9360=EDGE_CURVE('',#7688,#7689,#4622,.T.);
#9361=EDGE_CURVE('',#7690,#7688,#4623,.T.);
#9362=EDGE_CURVE('',#7690,#7691,#4624,.T.);
#9363=EDGE_CURVE('',#7691,#7689,#4625,.T.);
#9364=EDGE_CURVE('',#7689,#7692,#4626,.T.);
#9365=EDGE_CURVE('',#7691,#7693,#4627,.T.);
#9366=EDGE_CURVE('',#7693,#7692,#4628,.T.);
#9367=EDGE_CURVE('',#7692,#7694,#4629,.T.);
#9368=EDGE_CURVE('',#7693,#7695,#4630,.T.);
#9369=EDGE_CURVE('',#7695,#7694,#4631,.T.);
#9370=EDGE_CURVE('',#7694,#7688,#4632,.T.);
#9371=EDGE_CURVE('',#7695,#7690,#4633,.T.);
#9372=EDGE_CURVE('',#7696,#7697,#4634,.T.);
#9373=EDGE_CURVE('',#7698,#7696,#4635,.T.);
#9374=EDGE_CURVE('',#7698,#7699,#4636,.T.);
#9375=EDGE_CURVE('',#7699,#7697,#4637,.T.);
#9376=EDGE_CURVE('',#7697,#7700,#4638,.T.);
#9377=EDGE_CURVE('',#7699,#7701,#4639,.T.);
#9378=EDGE_CURVE('',#7701,#7700,#4640,.T.);
#9379=EDGE_CURVE('',#7700,#7702,#4641,.T.);
#9380=EDGE_CURVE('',#7701,#7703,#4642,.T.);
#9381=EDGE_CURVE('',#7703,#7702,#4643,.T.);
#9382=EDGE_CURVE('',#7702,#7696,#4644,.T.);
#9383=EDGE_CURVE('',#7703,#7698,#4645,.T.);
#9384=EDGE_CURVE('',#7704,#7705,#4646,.T.);
#9385=EDGE_CURVE('',#7706,#7704,#4647,.T.);
#9386=EDGE_CURVE('',#7706,#7707,#4648,.T.);
#9387=EDGE_CURVE('',#7707,#7705,#4649,.T.);
#9388=EDGE_CURVE('',#7705,#7708,#4650,.T.);
#9389=EDGE_CURVE('',#7707,#7709,#4651,.T.);
#9390=EDGE_CURVE('',#7709,#7708,#4652,.T.);
#9391=EDGE_CURVE('',#7708,#7710,#4653,.T.);
#9392=EDGE_CURVE('',#7709,#7711,#4654,.T.);
#9393=EDGE_CURVE('',#7711,#7710,#4655,.T.);
#9394=EDGE_CURVE('',#7710,#7704,#4656,.T.);
#9395=EDGE_CURVE('',#7711,#7706,#4657,.T.);
#9396=EDGE_CURVE('',#7712,#7713,#4658,.T.);
#9397=EDGE_CURVE('',#7714,#7712,#4659,.T.);
#9398=EDGE_CURVE('',#7714,#7715,#4660,.T.);
#9399=EDGE_CURVE('',#7715,#7713,#4661,.T.);
#9400=EDGE_CURVE('',#7713,#7716,#4662,.T.);
#9401=EDGE_CURVE('',#7715,#7717,#4663,.T.);
#9402=EDGE_CURVE('',#7717,#7716,#4664,.T.);
#9403=EDGE_CURVE('',#7716,#7718,#4665,.T.);
#9404=EDGE_CURVE('',#7717,#7719,#4666,.T.);
#9405=EDGE_CURVE('',#7719,#7718,#4667,.T.);
#9406=EDGE_CURVE('',#7718,#7712,#4668,.T.);
#9407=EDGE_CURVE('',#7719,#7714,#4669,.T.);
#9408=EDGE_CURVE('',#7720,#7721,#4670,.T.);
#9409=EDGE_CURVE('',#7722,#7720,#4671,.T.);
#9410=EDGE_CURVE('',#7722,#7723,#4672,.T.);
#9411=EDGE_CURVE('',#7723,#7721,#4673,.T.);
#9412=EDGE_CURVE('',#7721,#7724,#4674,.T.);
#9413=EDGE_CURVE('',#7723,#7725,#4675,.T.);
#9414=EDGE_CURVE('',#7725,#7724,#4676,.T.);
#9415=EDGE_CURVE('',#7724,#7726,#4677,.T.);
#9416=EDGE_CURVE('',#7725,#7727,#4678,.T.);
#9417=EDGE_CURVE('',#7727,#7726,#4679,.T.);
#9418=EDGE_CURVE('',#7726,#7720,#4680,.T.);
#9419=EDGE_CURVE('',#7727,#7722,#4681,.T.);
#9420=EDGE_CURVE('',#7728,#7729,#4682,.T.);
#9421=EDGE_CURVE('',#7730,#7728,#4683,.T.);
#9422=EDGE_CURVE('',#7730,#7731,#4684,.T.);
#9423=EDGE_CURVE('',#7731,#7729,#4685,.T.);
#9424=EDGE_CURVE('',#7729,#7732,#4686,.T.);
#9425=EDGE_CURVE('',#7731,#7733,#4687,.T.);
#9426=EDGE_CURVE('',#7733,#7732,#4688,.T.);
#9427=EDGE_CURVE('',#7732,#7734,#4689,.T.);
#9428=EDGE_CURVE('',#7733,#7735,#4690,.T.);
#9429=EDGE_CURVE('',#7735,#7734,#4691,.T.);
#9430=EDGE_CURVE('',#7734,#7728,#4692,.T.);
#9431=EDGE_CURVE('',#7735,#7730,#4693,.T.);
#9432=EDGE_CURVE('',#7736,#7737,#4694,.T.);
#9433=EDGE_CURVE('',#7738,#7736,#4695,.T.);
#9434=EDGE_CURVE('',#7738,#7739,#4696,.T.);
#9435=EDGE_CURVE('',#7739,#7737,#4697,.T.);
#9436=EDGE_CURVE('',#7737,#7740,#4698,.T.);
#9437=EDGE_CURVE('',#7739,#7741,#4699,.T.);
#9438=EDGE_CURVE('',#7741,#7740,#4700,.T.);
#9439=EDGE_CURVE('',#7740,#7742,#4701,.T.);
#9440=EDGE_CURVE('',#7741,#7743,#4702,.T.);
#9441=EDGE_CURVE('',#7743,#7742,#4703,.T.);
#9442=EDGE_CURVE('',#7742,#7736,#4704,.T.);
#9443=EDGE_CURVE('',#7743,#7738,#4705,.T.);
#9444=EDGE_CURVE('',#7744,#7745,#4706,.T.);
#9445=EDGE_CURVE('',#7746,#7744,#4707,.T.);
#9446=EDGE_CURVE('',#7746,#7747,#4708,.T.);
#9447=EDGE_CURVE('',#7747,#7745,#4709,.T.);
#9448=EDGE_CURVE('',#7745,#7748,#4710,.T.);
#9449=EDGE_CURVE('',#7747,#7749,#4711,.T.);
#9450=EDGE_CURVE('',#7749,#7748,#4712,.T.);
#9451=EDGE_CURVE('',#7748,#7750,#4713,.T.);
#9452=EDGE_CURVE('',#7749,#7751,#4714,.T.);
#9453=EDGE_CURVE('',#7751,#7750,#4715,.T.);
#9454=EDGE_CURVE('',#7750,#7744,#4716,.T.);
#9455=EDGE_CURVE('',#7751,#7746,#4717,.T.);
#9456=EDGE_CURVE('',#7752,#7753,#4718,.T.);
#9457=EDGE_CURVE('',#7754,#7752,#4719,.T.);
#9458=EDGE_CURVE('',#7754,#7755,#4720,.T.);
#9459=EDGE_CURVE('',#7755,#7753,#4721,.T.);
#9460=EDGE_CURVE('',#7753,#7756,#4722,.T.);
#9461=EDGE_CURVE('',#7755,#7757,#4723,.T.);
#9462=EDGE_CURVE('',#7757,#7756,#4724,.T.);
#9463=EDGE_CURVE('',#7756,#7758,#4725,.T.);
#9464=EDGE_CURVE('',#7757,#7759,#4726,.T.);
#9465=EDGE_CURVE('',#7759,#7758,#4727,.T.);
#9466=EDGE_CURVE('',#7758,#7752,#4728,.T.);
#9467=EDGE_CURVE('',#7759,#7754,#4729,.T.);
#9468=EDGE_CURVE('',#7760,#7761,#4730,.T.);
#9469=EDGE_CURVE('',#7762,#7760,#4731,.T.);
#9470=EDGE_CURVE('',#7762,#7763,#4732,.T.);
#9471=EDGE_CURVE('',#7763,#7761,#4733,.T.);
#9472=EDGE_CURVE('',#7761,#7764,#4734,.T.);
#9473=EDGE_CURVE('',#7763,#7765,#4735,.T.);
#9474=EDGE_CURVE('',#7765,#7764,#4736,.T.);
#9475=EDGE_CURVE('',#7764,#7766,#4737,.T.);
#9476=EDGE_CURVE('',#7765,#7767,#4738,.T.);
#9477=EDGE_CURVE('',#7767,#7766,#4739,.T.);
#9478=EDGE_CURVE('',#7766,#7760,#4740,.T.);
#9479=EDGE_CURVE('',#7767,#7762,#4741,.T.);
#9480=EDGE_CURVE('',#7768,#7769,#4742,.T.);
#9481=EDGE_CURVE('',#7770,#7768,#4743,.T.);
#9482=EDGE_CURVE('',#7770,#7771,#4744,.T.);
#9483=EDGE_CURVE('',#7771,#7769,#4745,.T.);
#9484=EDGE_CURVE('',#7769,#7772,#4746,.T.);
#9485=EDGE_CURVE('',#7771,#7773,#4747,.T.);
#9486=EDGE_CURVE('',#7773,#7772,#4748,.T.);
#9487=EDGE_CURVE('',#7772,#7774,#4749,.T.);
#9488=EDGE_CURVE('',#7773,#7775,#4750,.T.);
#9489=EDGE_CURVE('',#7775,#7774,#4751,.T.);
#9490=EDGE_CURVE('',#7774,#7768,#4752,.T.);
#9491=EDGE_CURVE('',#7775,#7770,#4753,.T.);
#9492=EDGE_CURVE('',#7776,#7777,#4754,.T.);
#9493=EDGE_CURVE('',#7778,#7776,#4755,.T.);
#9494=EDGE_CURVE('',#7778,#7779,#4756,.T.);
#9495=EDGE_CURVE('',#7779,#7777,#4757,.T.);
#9496=EDGE_CURVE('',#7777,#7780,#4758,.T.);
#9497=EDGE_CURVE('',#7779,#7781,#4759,.T.);
#9498=EDGE_CURVE('',#7781,#7780,#4760,.T.);
#9499=EDGE_CURVE('',#7780,#7782,#4761,.T.);
#9500=EDGE_CURVE('',#7781,#7783,#4762,.T.);
#9501=EDGE_CURVE('',#7783,#7782,#4763,.T.);
#9502=EDGE_CURVE('',#7782,#7776,#4764,.T.);
#9503=EDGE_CURVE('',#7783,#7778,#4765,.T.);
#9504=EDGE_CURVE('',#7784,#7784,#6873,.T.);
#9505=EDGE_CURVE('',#7784,#7785,#4766,.T.);
#9506=EDGE_CURVE('',#7785,#7785,#6874,.T.);
#9507=EDGE_CURVE('',#7786,#7786,#6875,.T.);
#9508=EDGE_CURVE('',#7786,#7787,#4767,.T.);
#9509=EDGE_CURVE('',#7787,#7787,#6876,.T.);
#9510=EDGE_CURVE('',#7788,#7788,#6877,.T.);
#9511=EDGE_CURVE('',#7788,#7789,#4768,.T.);
#9512=EDGE_CURVE('',#7789,#7789,#6878,.T.);
#9513=EDGE_CURVE('',#7790,#7791,#4769,.T.);
#9514=EDGE_CURVE('',#7792,#7790,#4770,.T.);
#9515=EDGE_CURVE('',#7792,#7793,#4771,.T.);
#9516=EDGE_CURVE('',#7791,#7793,#4772,.T.);
#9517=EDGE_CURVE('',#7794,#7795,#4773,.T.);
#9518=EDGE_CURVE('',#7796,#7794,#4774,.T.);
#9519=EDGE_CURVE('',#7797,#7796,#4775,.T.);
#9520=EDGE_CURVE('',#7795,#7797,#4776,.T.);
#9521=EDGE_CURVE('',#7797,#7798,#4777,.T.);
#9522=EDGE_CURVE('',#7799,#7796,#4778,.T.);
#9523=EDGE_CURVE('',#7798,#7799,#4779,.T.);
#9524=EDGE_CURVE('',#7798,#7800,#4780,.T.);
#9525=EDGE_CURVE('',#7801,#7799,#4781,.T.);
#9526=EDGE_CURVE('',#7800,#7801,#4782,.T.);
#9527=EDGE_CURVE('',#7800,#7792,#4783,.T.);
#9528=EDGE_CURVE('',#7793,#7801,#4784,.T.);
#9529=EDGE_CURVE('',#7802,#7795,#4785,.T.);
#9530=EDGE_CURVE('',#7803,#7802,#4786,.T.);
#9531=EDGE_CURVE('',#7794,#7803,#4787,.T.);
#9532=EDGE_CURVE('',#7790,#7804,#4788,.T.);
#9533=EDGE_CURVE('',#7802,#7804,#6879,.T.);
#9534=EDGE_CURVE('',#7805,#7791,#4789,.T.);
#9535=EDGE_CURVE('',#7804,#7805,#4790,.T.);
#9536=EDGE_CURVE('',#7803,#7805,#6880,.T.);
#9537=EDGE_CURVE('',#7806,#7806,#6881,.T.);
#9538=EDGE_CURVE('',#7806,#7807,#4791,.T.);
#9539=EDGE_CURVE('',#7807,#7807,#6882,.T.);
#9540=EDGE_CURVE('',#7808,#7808,#6883,.T.);
#9541=EDGE_CURVE('',#7808,#7809,#4792,.T.);
#9542=EDGE_CURVE('',#7809,#7809,#6884,.T.);
#9543=EDGE_CURVE('',#7810,#7810,#6885,.T.);
#9544=EDGE_CURVE('',#7810,#7811,#4793,.T.);
#9545=EDGE_CURVE('',#7811,#7811,#6886,.T.);
#9546=EDGE_CURVE('',#7812,#7812,#6887,.T.);
#9547=EDGE_CURVE('',#7812,#7813,#4794,.T.);
#9548=EDGE_CURVE('',#7813,#7813,#6888,.T.);
#9549=EDGE_CURVE('',#7814,#7815,#4795,.T.);
#9550=EDGE_CURVE('',#7815,#7816,#4796,.T.);
#9551=EDGE_CURVE('',#7817,#7816,#4797,.T.);
#9552=EDGE_CURVE('',#7814,#7817,#4798,.T.);
#9553=EDGE_CURVE('',#7818,#7814,#4799,.T.);
#9554=EDGE_CURVE('',#7819,#7817,#4800,.T.);
#9555=EDGE_CURVE('',#7818,#7819,#4801,.T.);
#9556=EDGE_CURVE('',#7820,#7818,#4802,.T.);
#9557=EDGE_CURVE('',#7821,#7819,#4803,.T.);
#9558=EDGE_CURVE('',#7820,#7821,#4804,.T.);
#9559=EDGE_CURVE('',#7815,#7820,#4805,.T.);
#9560=EDGE_CURVE('',#7816,#7821,#4806,.T.);
#9561=EDGE_CURVE('',#7822,#7823,#4807,.T.);
#9562=EDGE_CURVE('',#7823,#7824,#4808,.T.);
#9563=EDGE_CURVE('',#7825,#7824,#4809,.T.);
#9564=EDGE_CURVE('',#7822,#7825,#4810,.T.);
#9565=EDGE_CURVE('',#7826,#7822,#4811,.T.);
#9566=EDGE_CURVE('',#7827,#7825,#4812,.T.);
#9567=EDGE_CURVE('',#7826,#7827,#4813,.T.);
#9568=EDGE_CURVE('',#7828,#7826,#4814,.T.);
#9569=EDGE_CURVE('',#7829,#7827,#4815,.T.);
#9570=EDGE_CURVE('',#7828,#7829,#4816,.T.);
#9571=EDGE_CURVE('',#7823,#7828,#4817,.T.);
#9572=EDGE_CURVE('',#7824,#7829,#4818,.T.);
#9573=EDGE_CURVE('',#7830,#7831,#4819,.T.);
#9574=EDGE_CURVE('',#7831,#7832,#4820,.T.);
#9575=EDGE_CURVE('',#7832,#7833,#4821,.T.);
#9576=EDGE_CURVE('',#7830,#7833,#4822,.T.);
#9577=EDGE_CURVE('',#7831,#7834,#4823,.T.);
#9578=EDGE_CURVE('',#7834,#7835,#4824,.T.);
#9579=EDGE_CURVE('',#7835,#7832,#4825,.T.);
#9580=EDGE_CURVE('',#7834,#7836,#4826,.T.);
#9581=EDGE_CURVE('',#7836,#7837,#4827,.T.);
#9582=EDGE_CURVE('',#7837,#7835,#4828,.T.);
#9583=EDGE_CURVE('',#7836,#7838,#4829,.T.);
#9584=EDGE_CURVE('',#7838,#7839,#4830,.T.);
#9585=EDGE_CURVE('',#7839,#7837,#4831,.T.);
#9586=EDGE_CURVE('',#7838,#7840,#4832,.T.);
#9587=EDGE_CURVE('',#7840,#7841,#4833,.T.);
#9588=EDGE_CURVE('',#7841,#7839,#4834,.T.);
#9589=EDGE_CURVE('',#7840,#7830,#4835,.T.);
#9590=EDGE_CURVE('',#7833,#7841,#4836,.T.);
#9591=EDGE_CURVE('',#7842,#7842,#6889,.T.);
#9592=EDGE_CURVE('',#7843,#7843,#6890,.T.);
#9593=EDGE_CURVE('',#7842,#7844,#4837,.T.);
#9594=EDGE_CURVE('',#7844,#7844,#6891,.T.);
#9595=EDGE_CURVE('',#7845,#7845,#6892,.T.);
#9596=EDGE_CURVE('',#7846,#7846,#6893,.T.);
#9597=EDGE_CURVE('',#7846,#7845,#4838,.T.);
#9598=EDGE_CURVE('',#7847,#7847,#6894,.T.);
#9599=EDGE_CURVE('',#7847,#7846,#4839,.T.);
#9600=EDGE_CURVE('',#7848,#7848,#6895,.T.);
#9601=EDGE_CURVE('',#7848,#7847,#4840,.T.);
#9602=EDGE_CURVE('',#7849,#7849,#6896,.T.);
#9603=EDGE_CURVE('',#7850,#7850,#6897,.F.);
#9604=EDGE_CURVE('',#7850,#7849,#4841,.T.);
#9605=EDGE_CURVE('',#7843,#7850,#4842,.T.);
#9606=EDGE_CURVE('',#7851,#7851,#6898,.T.);
#9607=EDGE_CURVE('',#7851,#7852,#4843,.T.);
#9608=EDGE_CURVE('',#7852,#7852,#6899,.T.);
#9609=EDGE_CURVE('',#7853,#7854,#4844,.T.);
#9610=EDGE_CURVE('',#7853,#7855,#4845,.T.);
#9611=EDGE_CURVE('',#7856,#7855,#4846,.T.);
#9612=EDGE_CURVE('',#7856,#7854,#4847,.T.);
#9613=EDGE_CURVE('',#7854,#7857,#6900,.T.);
#9614=EDGE_CURVE('',#7858,#7856,#4848,.T.);
#9615=EDGE_CURVE('',#7857,#7858,#4849,.T.);
#9616=EDGE_CURVE('',#7857,#7859,#4850,.T.);
#9617=EDGE_CURVE('',#7858,#7860,#4851,.T.);
#9618=EDGE_CURVE('',#7860,#7859,#4852,.T.);
#9619=EDGE_CURVE('',#7855,#7860,#4853,.T.);
#9620=EDGE_CURVE('',#7859,#7853,#6901,.T.);
#9621=EDGE_CURVE('',#7861,#7862,#4854,.T.);
#9622=EDGE_CURVE('',#7861,#7863,#4855,.T.);
#9623=EDGE_CURVE('',#7864,#7863,#4856,.T.);
#9624=EDGE_CURVE('',#7864,#7862,#4857,.T.);
#9625=EDGE_CURVE('',#7862,#7865,#6902,.T.);
#9626=EDGE_CURVE('',#7866,#7864,#4858,.T.);
#9627=EDGE_CURVE('',#7865,#7866,#4859,.T.);
#9628=EDGE_CURVE('',#7865,#7867,#4860,.T.);
#9629=EDGE_CURVE('',#7866,#7868,#4861,.T.);
#9630=EDGE_CURVE('',#7868,#7867,#4862,.T.);
#9631=EDGE_CURVE('',#7863,#7868,#4863,.T.);
#9632=EDGE_CURVE('',#7867,#7861,#6903,.T.);
#9633=EDGE_CURVE('',#7869,#7869,#6904,.T.);
#9634=EDGE_CURVE('',#7870,#7870,#6905,.T.);
#9635=EDGE_CURVE('',#7871,#7871,#6906,.T.);
#9636=EDGE_CURVE('',#7872,#7872,#6907,.T.);
#9637=EDGE_CURVE('',#7869,#7871,#4864,.T.);
#9638=EDGE_CURVE('',#7872,#7873,#4865,.T.);
#9639=EDGE_CURVE('',#7873,#7873,#6908,.T.);
#9640=EDGE_CURVE('',#7874,#7874,#6909,.T.);
#9641=EDGE_CURVE('',#7874,#7870,#4866,.T.);
#9642=EDGE_CURVE('',#7875,#7875,#6910,.T.);
#9643=EDGE_CURVE('',#7875,#7876,#4867,.T.);
#9644=EDGE_CURVE('',#7876,#7876,#6911,.T.);
#9645=EDGE_CURVE('',#7877,#7877,#6912,.T.);
#9646=EDGE_CURVE('',#7877,#7878,#4868,.T.);
#9647=EDGE_CURVE('',#7878,#7878,#6913,.T.);
#9648=EDGE_CURVE('',#7879,#7879,#6914,.T.);
#9649=EDGE_CURVE('',#7879,#7880,#4869,.T.);
#9650=EDGE_CURVE('',#7880,#7880,#6915,.T.);
#9651=EDGE_CURVE('',#7881,#7881,#6916,.T.);
#9652=EDGE_CURVE('',#7881,#7882,#4870,.T.);
#9653=EDGE_CURVE('',#7882,#7882,#6917,.T.);
#9654=EDGE_CURVE('',#7883,#7884,#4871,.T.);
#9655=EDGE_CURVE('',#7883,#7884,#6918,.T.);
#9656=EDGE_CURVE('',#7885,#7883,#891,.T.);
#9657=EDGE_CURVE('',#7886,#7885,#6919,.T.);
#9658=EDGE_CURVE('',#7886,#7887,#4872,.T.);
#9659=EDGE_CURVE('',#7888,#7887,#892,.T.);
#9660=EDGE_CURVE('',#7887,#7888,#893,.T.);
#9661=EDGE_CURVE('',#7889,#7886,#6920,.T.);
#9662=EDGE_CURVE('',#7884,#7889,#894,.T.);
#9663=EDGE_CURVE('',#7889,#7885,#4873,.T.);
#9664=EDGE_CURVE('',#7890,#7890,#6921,.T.);
#9665=EDGE_CURVE('',#7890,#7891,#4874,.T.);
#9666=EDGE_CURVE('',#7891,#7891,#6922,.T.);
#9667=EDGE_CURVE('',#7892,#7892,#6923,.T.);
#9668=EDGE_CURVE('',#7892,#7893,#4875,.T.);
#9669=EDGE_CURVE('',#7893,#7893,#6924,.T.);
#9670=EDGE_CURVE('',#7894,#7894,#6925,.T.);
#9671=EDGE_CURVE('',#7894,#7895,#4876,.T.);
#9672=EDGE_CURVE('',#7895,#7895,#6926,.T.);
#9673=EDGE_CURVE('',#7896,#7897,#4877,.T.);
#9674=EDGE_CURVE('',#7896,#7898,#4878,.T.);
#9675=EDGE_CURVE('',#7899,#7898,#4879,.T.);
#9676=EDGE_CURVE('',#7897,#7899,#4880,.T.);
#9677=EDGE_CURVE('',#7900,#7896,#4881,.T.);
#9678=EDGE_CURVE('',#7900,#7901,#4882,.T.);
#9679=EDGE_CURVE('',#7898,#7901,#4883,.T.);
#9680=EDGE_CURVE('',#7902,#7900,#4884,.T.);
#9681=EDGE_CURVE('',#7903,#7902,#4885,.T.);
#9682=EDGE_CURVE('',#7901,#7903,#4886,.T.);
#9683=EDGE_CURVE('',#7904,#7904,#6927,.T.);
#9684=EDGE_CURVE('',#7903,#7899,#6928,.T.);
#9685=EDGE_CURVE('',#7902,#7897,#6929,.T.);
#9686=EDGE_CURVE('',#7905,#7906,#4887,.T.);
#9687=EDGE_CURVE('',#7907,#7905,#6930,.T.);
#9688=EDGE_CURVE('',#7908,#7907,#4888,.T.);
#9689=EDGE_CURVE('',#7908,#7906,#6931,.T.);
#9690=EDGE_CURVE('',#7908,#7909,#4889,.T.);
#9691=EDGE_CURVE('',#7910,#7909,#6932,.T.);
#9692=EDGE_CURVE('',#7910,#7906,#4890,.T.);
#9693=EDGE_CURVE('',#7911,#7907,#4891,.T.);
#9694=EDGE_CURVE('',#7909,#7911,#4892,.T.);
#9695=EDGE_CURVE('',#7905,#7912,#4893,.T.);
#9696=EDGE_CURVE('',#7911,#7912,#6933,.T.);
#9697=EDGE_CURVE('',#7912,#7910,#4894,.T.);
#9698=EDGE_CURVE('',#7904,#7913,#4895,.T.);
#9699=EDGE_CURVE('',#7913,#7913,#6934,.T.);
#9700=EDGE_CURVE('',#7914,#7914,#6935,.T.);
#9701=EDGE_CURVE('',#7914,#7915,#4896,.T.);
#9702=EDGE_CURVE('',#7915,#7915,#6936,.T.);
#9703=EDGE_CURVE('',#7916,#7916,#6937,.T.);
#9704=EDGE_CURVE('',#7916,#7917,#4897,.T.);
#9705=EDGE_CURVE('',#7917,#7917,#6938,.T.);
#9706=EDGE_CURVE('',#7918,#7918,#6939,.T.);
#9707=EDGE_CURVE('',#7918,#7919,#4898,.T.);
#9708=EDGE_CURVE('',#7919,#7919,#6940,.T.);
#9709=EDGE_CURVE('',#7920,#7920,#6941,.T.);
#9710=EDGE_CURVE('',#7920,#7921,#4899,.T.);
#9711=EDGE_CURVE('',#7921,#7921,#6942,.T.);
#9712=EDGE_CURVE('',#7922,#7922,#6943,.T.);
#9713=EDGE_CURVE('',#7922,#7923,#4900,.T.);
#9714=EDGE_CURVE('',#7923,#7923,#6944,.T.);
#9715=EDGE_CURVE('',#7924,#7924,#6945,.T.);
#9716=EDGE_CURVE('',#7924,#7925,#4901,.T.);
#9717=EDGE_CURVE('',#7925,#7925,#6946,.T.);
#9718=EDGE_CURVE('',#7926,#7926,#6947,.T.);
#9719=EDGE_CURVE('',#7926,#7927,#4902,.T.);
#9720=EDGE_CURVE('',#7927,#7927,#6948,.T.);
#9721=EDGE_CURVE('',#7928,#7928,#6949,.T.);
#9722=EDGE_CURVE('',#7928,#7929,#4903,.T.);
#9723=EDGE_CURVE('',#7929,#7929,#6950,.T.);
#9724=EDGE_CURVE('',#7930,#7930,#6951,.T.);
#9725=EDGE_CURVE('',#7930,#7931,#4904,.T.);
#9726=EDGE_CURVE('',#7931,#7931,#6952,.T.);
#9727=EDGE_CURVE('',#7932,#7932,#6953,.T.);
#9728=EDGE_CURVE('',#7932,#7933,#4905,.T.);
#9729=EDGE_CURVE('',#7933,#7933,#6954,.T.);
#9730=EDGE_CURVE('',#7934,#7935,#4906,.T.);
#9731=EDGE_CURVE('',#7935,#7936,#4907,.T.);
#9732=EDGE_CURVE('',#7936,#7937,#4908,.T.);
#9733=EDGE_CURVE('',#7934,#7937,#4909,.T.);
#9734=EDGE_CURVE('',#7935,#7938,#4910,.T.);
#9735=EDGE_CURVE('',#7938,#7939,#4911,.T.);
#9736=EDGE_CURVE('',#7939,#7936,#4912,.T.);
#9737=EDGE_CURVE('',#7938,#7940,#4913,.T.);
#9738=EDGE_CURVE('',#7940,#7941,#4914,.T.);
#9739=EDGE_CURVE('',#7941,#7939,#4915,.T.);
#9740=EDGE_CURVE('',#7940,#7942,#4916,.T.);
#9741=EDGE_CURVE('',#7942,#7943,#4917,.T.);
#9742=EDGE_CURVE('',#7943,#7941,#4918,.T.);
#9743=EDGE_CURVE('',#7942,#7944,#4919,.T.);
#9744=EDGE_CURVE('',#7944,#7945,#4920,.T.);
#9745=EDGE_CURVE('',#7945,#7943,#4921,.T.);
#9746=EDGE_CURVE('',#7944,#7934,#4922,.T.);
#9747=EDGE_CURVE('',#7937,#7945,#4923,.T.);
#9748=EDGE_CURVE('',#7946,#7946,#6955,.T.);
#9749=EDGE_CURVE('',#7947,#7947,#6956,.T.);
#9750=EDGE_CURVE('',#7946,#7948,#4924,.T.);
#9751=EDGE_CURVE('',#7948,#7948,#6957,.T.);
#9752=EDGE_CURVE('',#7949,#7949,#6958,.T.);
#9753=EDGE_CURVE('',#7950,#7950,#6959,.T.);
#9754=EDGE_CURVE('',#7950,#7949,#4925,.T.);
#9755=EDGE_CURVE('',#7951,#7951,#6960,.T.);
#9756=EDGE_CURVE('',#7951,#7950,#4926,.T.);
#9757=EDGE_CURVE('',#7952,#7952,#6961,.T.);
#9758=EDGE_CURVE('',#7952,#7951,#4927,.T.);
#9759=EDGE_CURVE('',#7953,#7953,#6962,.T.);
#9760=EDGE_CURVE('',#7954,#7954,#6963,.F.);
#9761=EDGE_CURVE('',#7954,#7953,#4928,.T.);
#9762=EDGE_CURVE('',#7947,#7954,#4929,.T.);
#9763=EDGE_CURVE('',#7955,#7955,#6964,.T.);
#9764=EDGE_CURVE('',#7955,#7956,#4930,.T.);
#9765=EDGE_CURVE('',#7956,#7956,#6965,.T.);
#9766=EDGE_CURVE('',#7957,#7958,#4931,.T.);
#9767=EDGE_CURVE('',#7957,#7959,#4932,.T.);
#9768=EDGE_CURVE('',#7960,#7959,#4933,.T.);
#9769=EDGE_CURVE('',#7960,#7958,#4934,.T.);
#9770=EDGE_CURVE('',#7958,#7961,#6966,.T.);
#9771=EDGE_CURVE('',#7962,#7960,#4935,.T.);
#9772=EDGE_CURVE('',#7961,#7962,#4936,.T.);
#9773=EDGE_CURVE('',#7961,#7963,#4937,.T.);
#9774=EDGE_CURVE('',#7962,#7964,#4938,.T.);
#9775=EDGE_CURVE('',#7964,#7963,#4939,.T.);
#9776=EDGE_CURVE('',#7959,#7964,#4940,.T.);
#9777=EDGE_CURVE('',#7963,#7957,#6967,.T.);
#9778=EDGE_CURVE('',#7965,#7965,#6968,.T.);
#9779=EDGE_CURVE('',#7966,#7966,#6969,.T.);
#9780=EDGE_CURVE('',#7967,#7967,#6970,.T.);
#9781=EDGE_CURVE('',#7968,#7968,#6971,.T.);
#9782=EDGE_CURVE('',#7965,#7967,#4941,.T.);
#9783=EDGE_CURVE('',#7968,#7969,#4942,.T.);
#9784=EDGE_CURVE('',#7969,#7969,#6972,.T.);
#9785=EDGE_CURVE('',#7970,#7970,#6973,.T.);
#9786=EDGE_CURVE('',#7970,#7966,#4943,.T.);
#9787=EDGE_CURVE('',#7971,#7971,#6974,.T.);
#9788=EDGE_CURVE('',#7971,#7972,#4944,.T.);
#9789=EDGE_CURVE('',#7972,#7972,#6975,.T.);
#9790=EDGE_CURVE('',#7973,#7973,#6976,.T.);
#9791=EDGE_CURVE('',#7973,#7974,#4945,.T.);
#9792=EDGE_CURVE('',#7974,#7974,#6977,.T.);
#9793=EDGE_CURVE('',#7975,#7975,#6978,.T.);
#9794=EDGE_CURVE('',#7975,#7976,#4946,.T.);
#9795=EDGE_CURVE('',#7976,#7976,#6979,.T.);
#9796=EDGE_CURVE('',#7977,#7977,#6980,.T.);
#9797=EDGE_CURVE('',#7977,#7978,#4947,.T.);
#9798=EDGE_CURVE('',#7978,#7978,#6981,.T.);
#9799=EDGE_CURVE('',#7979,#7980,#4948,.T.);
#9800=EDGE_CURVE('',#7979,#7980,#6982,.T.);
#9801=EDGE_CURVE('',#7981,#7979,#895,.T.);
#9802=EDGE_CURVE('',#7982,#7981,#6983,.T.);
#9803=EDGE_CURVE('',#7982,#7983,#4949,.T.);
#9804=EDGE_CURVE('',#7984,#7983,#896,.T.);
#9805=EDGE_CURVE('',#7983,#7984,#897,.T.);
#9806=EDGE_CURVE('',#7985,#7982,#6984,.T.);
#9807=EDGE_CURVE('',#7980,#7985,#898,.T.);
#9808=EDGE_CURVE('',#7985,#7981,#4950,.T.);
#9809=EDGE_CURVE('',#7986,#7986,#6985,.T.);
#9810=EDGE_CURVE('',#7986,#7987,#4951,.T.);
#9811=EDGE_CURVE('',#7987,#7987,#6986,.T.);
#9812=EDGE_CURVE('',#7988,#7988,#6987,.T.);
#9813=EDGE_CURVE('',#7988,#7989,#4952,.T.);
#9814=EDGE_CURVE('',#7989,#7989,#6988,.T.);
#9815=EDGE_CURVE('',#7990,#7990,#6989,.T.);
#9816=EDGE_CURVE('',#7990,#7991,#4953,.T.);
#9817=EDGE_CURVE('',#7991,#7991,#6990,.T.);
#9818=EDGE_CURVE('',#7992,#7992,#6991,.T.);
#9819=EDGE_CURVE('',#7992,#7993,#4954,.T.);
#9820=EDGE_CURVE('',#7993,#7993,#6992,.T.);
#9821=EDGE_CURVE('',#7994,#7994,#6993,.T.);
#9822=EDGE_CURVE('',#7994,#7995,#4955,.T.);
#9823=EDGE_CURVE('',#7995,#7995,#6994,.T.);
#9824=EDGE_CURVE('',#7996,#7997,#4956,.T.);
#9825=EDGE_CURVE('',#7996,#7998,#4957,.T.);
#9826=EDGE_CURVE('',#7999,#7998,#4958,.T.);
#9827=EDGE_CURVE('',#7999,#7997,#4959,.T.);
#9828=EDGE_CURVE('',#7997,#8000,#6995,.T.);
#9829=EDGE_CURVE('',#8001,#7999,#4960,.T.);
#9830=EDGE_CURVE('',#8000,#8001,#4961,.T.);
#9831=EDGE_CURVE('',#8000,#8002,#4962,.T.);
#9832=EDGE_CURVE('',#8001,#8003,#4963,.T.);
#9833=EDGE_CURVE('',#8003,#8002,#4964,.T.);
#9834=EDGE_CURVE('',#7998,#8003,#4965,.T.);
#9835=EDGE_CURVE('',#8002,#7996,#6996,.T.);
#9836=EDGE_CURVE('',#8004,#8004,#6997,.T.);
#9837=EDGE_CURVE('',#8005,#8005,#6998,.T.);
#9838=EDGE_CURVE('',#8006,#8006,#6999,.T.);
#9839=EDGE_CURVE('',#8007,#8007,#7000,.T.);
#9840=EDGE_CURVE('',#8004,#8006,#4966,.T.);
#9841=EDGE_CURVE('',#8007,#8008,#4967,.T.);
#9842=EDGE_CURVE('',#8008,#8008,#7001,.T.);
#9843=EDGE_CURVE('',#8009,#8009,#7002,.T.);
#9844=EDGE_CURVE('',#8009,#8005,#4968,.T.);
#9845=EDGE_CURVE('',#8010,#8010,#7003,.T.);
#9846=EDGE_CURVE('',#8010,#8011,#4969,.T.);
#9847=EDGE_CURVE('',#8011,#8011,#7004,.T.);
#9848=EDGE_CURVE('',#8012,#8012,#7005,.T.);
#9849=EDGE_CURVE('',#8012,#8013,#4970,.T.);
#9850=EDGE_CURVE('',#8013,#8013,#7006,.T.);
#9851=EDGE_CURVE('',#8014,#8014,#7007,.T.);
#9852=EDGE_CURVE('',#8014,#8015,#4971,.T.);
#9853=EDGE_CURVE('',#8015,#8015,#7008,.T.);
#9854=EDGE_CURVE('',#8016,#8016,#7009,.T.);
#9855=EDGE_CURVE('',#8016,#8017,#4972,.T.);
#9856=EDGE_CURVE('',#8017,#8017,#7010,.T.);
#9857=EDGE_CURVE('',#8018,#8019,#4973,.T.);
#9858=EDGE_CURVE('',#8018,#8019,#7011,.T.);
#9859=EDGE_CURVE('',#8020,#8018,#899,.T.);
#9860=EDGE_CURVE('',#8021,#8020,#7012,.T.);
#9861=EDGE_CURVE('',#8021,#8022,#4974,.T.);
#9862=EDGE_CURVE('',#8023,#8022,#900,.T.);
#9863=EDGE_CURVE('',#8022,#8023,#901,.T.);
#9864=EDGE_CURVE('',#8024,#8021,#7013,.T.);
#9865=EDGE_CURVE('',#8019,#8024,#902,.T.);
#9866=EDGE_CURVE('',#8024,#8020,#4975,.T.);
#9867=EDGE_CURVE('',#8025,#8025,#7014,.T.);
#9868=EDGE_CURVE('',#8025,#8026,#4976,.T.);
#9869=EDGE_CURVE('',#8026,#8026,#7015,.T.);
#9870=EDGE_CURVE('',#8027,#8027,#7016,.T.);
#9871=EDGE_CURVE('',#8027,#8028,#4977,.T.);
#9872=EDGE_CURVE('',#8028,#8028,#7017,.T.);
#9873=EDGE_CURVE('',#8029,#8029,#7018,.T.);
#9874=EDGE_CURVE('',#8029,#8030,#4978,.T.);
#9875=EDGE_CURVE('',#8030,#8030,#7019,.T.);
#9876=EDGE_CURVE('',#8031,#8031,#7020,.T.);
#9877=EDGE_CURVE('',#8031,#8032,#4979,.T.);
#9878=EDGE_CURVE('',#8032,#8032,#7021,.T.);
#9879=EDGE_CURVE('',#8033,#8034,#4980,.T.);
#9880=EDGE_CURVE('',#8035,#8033,#4981,.T.);
#9881=EDGE_CURVE('',#8036,#8035,#4982,.T.);
#9882=EDGE_CURVE('',#8034,#8036,#4983,.T.);
#9883=EDGE_CURVE('',#8037,#8033,#4984,.T.);
#9884=EDGE_CURVE('',#8037,#8038,#4985,.T.);
#9885=EDGE_CURVE('',#8035,#8038,#4986,.T.);
#9886=EDGE_CURVE('',#8039,#8037,#4987,.T.);
#9887=EDGE_CURVE('',#8040,#8039,#4988,.T.);
#9888=EDGE_CURVE('',#8038,#8040,#4989,.T.);
#9889=EDGE_CURVE('',#8041,#8042,#7022,.T.);
#9890=EDGE_CURVE('',#8042,#8043,#131,.T.);
#9891=EDGE_CURVE('',#8043,#8044,#4990,.T.);
#9892=EDGE_CURVE('',#8044,#8045,#132,.T.);
#9893=EDGE_CURVE('',#8045,#8046,#7023,.T.);
#9894=EDGE_CURVE('',#8046,#8047,#133,.T.);
#9895=EDGE_CURVE('',#8047,#8048,#4991,.T.);
#9896=EDGE_CURVE('',#8048,#8049,#134,.T.);
#9897=EDGE_CURVE('',#8049,#8050,#7024,.T.);
#9898=EDGE_CURVE('',#8050,#8051,#135,.T.);
#9899=EDGE_CURVE('',#8051,#8052,#4992,.T.);
#9900=EDGE_CURVE('',#8052,#8053,#136,.T.);
#9901=EDGE_CURVE('',#8053,#8054,#7025,.T.);
#9902=EDGE_CURVE('',#8054,#8055,#137,.T.);
#9903=EDGE_CURVE('',#8055,#8056,#4993,.T.);
#9904=EDGE_CURVE('',#8056,#8057,#138,.T.);
#9905=EDGE_CURVE('',#8057,#8058,#7026,.T.);
#9906=EDGE_CURVE('',#8058,#8059,#139,.T.);
#9907=EDGE_CURVE('',#8059,#8060,#4994,.T.);
#9908=EDGE_CURVE('',#8060,#8061,#140,.T.);
#9909=EDGE_CURVE('',#8061,#8062,#7027,.T.);
#9910=EDGE_CURVE('',#8062,#8063,#141,.T.);
#9911=EDGE_CURVE('',#8063,#8064,#4995,.T.);
#9912=EDGE_CURVE('',#8064,#8065,#142,.T.);
#9913=EDGE_CURVE('',#8065,#8066,#7028,.T.);
#9914=EDGE_CURVE('',#8066,#8067,#143,.T.);
#9915=EDGE_CURVE('',#8067,#8068,#4996,.T.);
#9916=EDGE_CURVE('',#8068,#8069,#144,.T.);
#9917=EDGE_CURVE('',#8069,#8070,#7029,.T.);
#9918=EDGE_CURVE('',#8070,#8071,#145,.T.);
#9919=EDGE_CURVE('',#8071,#8072,#4997,.T.);
#9920=EDGE_CURVE('',#8072,#8073,#146,.T.);
#9921=EDGE_CURVE('',#8073,#8074,#7030,.T.);
#9922=EDGE_CURVE('',#8074,#8075,#147,.T.);
#9923=EDGE_CURVE('',#8075,#8076,#4998,.T.);
#9924=EDGE_CURVE('',#8076,#8077,#148,.T.);
#9925=EDGE_CURVE('',#8077,#8078,#7031,.T.);
#9926=EDGE_CURVE('',#8078,#8079,#149,.T.);
#9927=EDGE_CURVE('',#8079,#8080,#4999,.T.);
#9928=EDGE_CURVE('',#8080,#8081,#150,.T.);
#9929=EDGE_CURVE('',#8081,#8082,#7032,.T.);
#9930=EDGE_CURVE('',#8082,#8083,#151,.T.);
#9931=EDGE_CURVE('',#8083,#8084,#5000,.T.);
#9932=EDGE_CURVE('',#8084,#8085,#152,.T.);
#9933=EDGE_CURVE('',#8085,#8086,#7033,.T.);
#9934=EDGE_CURVE('',#8086,#8087,#153,.T.);
#9935=EDGE_CURVE('',#8087,#8088,#5001,.T.);
#9936=EDGE_CURVE('',#8088,#8089,#154,.T.);
#9937=EDGE_CURVE('',#8089,#8090,#7034,.T.);
#9938=EDGE_CURVE('',#8090,#8091,#155,.T.);
#9939=EDGE_CURVE('',#8091,#8092,#5002,.T.);
#9940=EDGE_CURVE('',#8092,#8093,#156,.T.);
#9941=EDGE_CURVE('',#8093,#8094,#7035,.T.);
#9942=EDGE_CURVE('',#8094,#8095,#157,.T.);
#9943=EDGE_CURVE('',#8095,#8096,#5003,.T.);
#9944=EDGE_CURVE('',#8096,#8097,#158,.T.);
#9945=EDGE_CURVE('',#8097,#8098,#7036,.T.);
#9946=EDGE_CURVE('',#8098,#8099,#159,.T.);
#9947=EDGE_CURVE('',#8099,#8100,#5004,.T.);
#9948=EDGE_CURVE('',#8100,#8101,#160,.T.);
#9949=EDGE_CURVE('',#8101,#8102,#7037,.T.);
#9950=EDGE_CURVE('',#8102,#8103,#161,.T.);
#9951=EDGE_CURVE('',#8103,#8104,#5005,.T.);
#9952=EDGE_CURVE('',#8104,#8105,#162,.T.);
#9953=EDGE_CURVE('',#8105,#8106,#7038,.T.);
#9954=EDGE_CURVE('',#8106,#8107,#163,.T.);
#9955=EDGE_CURVE('',#8107,#8108,#5006,.T.);
#9956=EDGE_CURVE('',#8108,#8109,#164,.T.);
#9957=EDGE_CURVE('',#8109,#8110,#7039,.T.);
#9958=EDGE_CURVE('',#8110,#8111,#165,.T.);
#9959=EDGE_CURVE('',#8111,#8112,#5007,.T.);
#9960=EDGE_CURVE('',#8112,#8113,#166,.T.);
#9961=EDGE_CURVE('',#8113,#8114,#7040,.T.);
#9962=EDGE_CURVE('',#8114,#8115,#167,.T.);
#9963=EDGE_CURVE('',#8115,#8116,#5008,.T.);
#9964=EDGE_CURVE('',#8116,#8117,#168,.T.);
#9965=EDGE_CURVE('',#8117,#8118,#7041,.T.);
#9966=EDGE_CURVE('',#8118,#8119,#169,.T.);
#9967=EDGE_CURVE('',#8119,#8120,#5009,.T.);
#9968=EDGE_CURVE('',#8120,#8041,#170,.T.);
#9969=EDGE_CURVE('',#8040,#8036,#7042,.T.);
#9970=EDGE_CURVE('',#8034,#8039,#7043,.T.);
#9971=EDGE_CURVE('',#8121,#8121,#7044,.T.);
#9972=EDGE_CURVE('',#8121,#8122,#5010,.T.);
#9973=EDGE_CURVE('',#8122,#8122,#7045,.T.);
#9974=EDGE_CURVE('',#8123,#8118,#5011,.T.);
#9975=EDGE_CURVE('',#8124,#8123,#171,.T.);
#9976=EDGE_CURVE('',#8119,#8124,#5012,.T.);
#9977=EDGE_CURVE('',#8125,#8124,#5013,.T.);
#9978=EDGE_CURVE('',#8120,#8125,#5014,.T.);
#9979=EDGE_CURVE('',#8126,#8125,#172,.T.);
#9980=EDGE_CURVE('',#8041,#8126,#5015,.T.);
#9981=EDGE_CURVE('',#8127,#8126,#7046,.T.);
#9982=EDGE_CURVE('',#8127,#8042,#5016,.T.);
#9983=EDGE_CURVE('',#8128,#8127,#173,.T.);
#9984=EDGE_CURVE('',#8043,#8128,#5017,.T.);
#9985=EDGE_CURVE('',#8129,#8128,#5018,.T.);
#9986=EDGE_CURVE('',#8044,#8129,#5019,.T.);
#9987=EDGE_CURVE('',#8130,#8129,#174,.T.);
#9988=EDGE_CURVE('',#8045,#8130,#5020,.T.);
#9989=EDGE_CURVE('',#8131,#8130,#7047,.T.);
#9990=EDGE_CURVE('',#8131,#8046,#5021,.T.);
#9991=EDGE_CURVE('',#8132,#8131,#175,.T.);
#9992=EDGE_CURVE('',#8047,#8132,#5022,.T.);
#9993=EDGE_CURVE('',#8133,#8132,#5023,.T.);
#9994=EDGE_CURVE('',#8048,#8133,#5024,.T.);
#9995=EDGE_CURVE('',#8134,#8133,#176,.T.);
#9996=EDGE_CURVE('',#8049,#8134,#5025,.T.);
#9997=EDGE_CURVE('',#8135,#8134,#7048,.T.);
#9998=EDGE_CURVE('',#8135,#8050,#5026,.T.);
#9999=EDGE_CURVE('',#8136,#8135,#177,.T.);
#10000=EDGE_CURVE('',#8051,#8136,#5027,.T.);
#10001=EDGE_CURVE('',#8137,#8136,#5028,.T.);
#10002=EDGE_CURVE('',#8052,#8137,#5029,.T.);
#10003=EDGE_CURVE('',#8138,#8137,#178,.T.);
#10004=EDGE_CURVE('',#8053,#8138,#5030,.T.);
#10005=EDGE_CURVE('',#8139,#8138,#7049,.T.);
#10006=EDGE_CURVE('',#8139,#8054,#5031,.T.);
#10007=EDGE_CURVE('',#8140,#8139,#179,.T.);
#10008=EDGE_CURVE('',#8055,#8140,#5032,.T.);
#10009=EDGE_CURVE('',#8141,#8140,#5033,.T.);
#10010=EDGE_CURVE('',#8056,#8141,#5034,.T.);
#10011=EDGE_CURVE('',#8142,#8141,#180,.T.);
#10012=EDGE_CURVE('',#8057,#8142,#5035,.T.);
#10013=EDGE_CURVE('',#8143,#8142,#7050,.T.);
#10014=EDGE_CURVE('',#8143,#8058,#5036,.T.);
#10015=EDGE_CURVE('',#8144,#8143,#181,.T.);
#10016=EDGE_CURVE('',#8059,#8144,#5037,.T.);
#10017=EDGE_CURVE('',#8145,#8144,#5038,.T.);
#10018=EDGE_CURVE('',#8060,#8145,#5039,.T.);
#10019=EDGE_CURVE('',#8146,#8145,#182,.T.);
#10020=EDGE_CURVE('',#8061,#8146,#5040,.T.);
#10021=EDGE_CURVE('',#8147,#8146,#7051,.T.);
#10022=EDGE_CURVE('',#8147,#8062,#5041,.T.);
#10023=EDGE_CURVE('',#8148,#8147,#183,.T.);
#10024=EDGE_CURVE('',#8063,#8148,#5042,.T.);
#10025=EDGE_CURVE('',#8149,#8148,#5043,.T.);
#10026=EDGE_CURVE('',#8064,#8149,#5044,.T.);
#10027=EDGE_CURVE('',#8150,#8149,#184,.T.);
#10028=EDGE_CURVE('',#8065,#8150,#5045,.T.);
#10029=EDGE_CURVE('',#8151,#8150,#7052,.T.);
#10030=EDGE_CURVE('',#8151,#8066,#5046,.T.);
#10031=EDGE_CURVE('',#8152,#8151,#185,.T.);
#10032=EDGE_CURVE('',#8067,#8152,#5047,.T.);
#10033=EDGE_CURVE('',#8153,#8152,#5048,.T.);
#10034=EDGE_CURVE('',#8068,#8153,#5049,.T.);
#10035=EDGE_CURVE('',#8154,#8153,#186,.T.);
#10036=EDGE_CURVE('',#8069,#8154,#5050,.T.);
#10037=EDGE_CURVE('',#8155,#8154,#7053,.T.);
#10038=EDGE_CURVE('',#8155,#8070,#5051,.T.);
#10039=EDGE_CURVE('',#8156,#8155,#187,.T.);
#10040=EDGE_CURVE('',#8071,#8156,#5052,.T.);
#10041=EDGE_CURVE('',#8157,#8156,#5053,.T.);
#10042=EDGE_CURVE('',#8072,#8157,#5054,.T.);
#10043=EDGE_CURVE('',#8158,#8157,#188,.T.);
#10044=EDGE_CURVE('',#8073,#8158,#5055,.T.);
#10045=EDGE_CURVE('',#8159,#8158,#7054,.T.);
#10046=EDGE_CURVE('',#8159,#8074,#5056,.T.);
#10047=EDGE_CURVE('',#8160,#8159,#189,.T.);
#10048=EDGE_CURVE('',#8075,#8160,#5057,.T.);
#10049=EDGE_CURVE('',#8161,#8160,#5058,.T.);
#10050=EDGE_CURVE('',#8076,#8161,#5059,.T.);
#10051=EDGE_CURVE('',#8162,#8161,#190,.T.);
#10052=EDGE_CURVE('',#8077,#8162,#5060,.T.);
#10053=EDGE_CURVE('',#8163,#8162,#7055,.T.);
#10054=EDGE_CURVE('',#8163,#8078,#5061,.T.);
#10055=EDGE_CURVE('',#8164,#8163,#191,.T.);
#10056=EDGE_CURVE('',#8079,#8164,#5062,.T.);
#10057=EDGE_CURVE('',#8165,#8164,#5063,.T.);
#10058=EDGE_CURVE('',#8080,#8165,#5064,.T.);
#10059=EDGE_CURVE('',#8166,#8165,#192,.T.);
#10060=EDGE_CURVE('',#8081,#8166,#5065,.T.);
#10061=EDGE_CURVE('',#8167,#8166,#7056,.T.);
#10062=EDGE_CURVE('',#8167,#8082,#5066,.T.);
#10063=EDGE_CURVE('',#8168,#8167,#193,.T.);
#10064=EDGE_CURVE('',#8083,#8168,#5067,.T.);
#10065=EDGE_CURVE('',#8169,#8168,#5068,.T.);
#10066=EDGE_CURVE('',#8084,#8169,#5069,.T.);
#10067=EDGE_CURVE('',#8170,#8169,#194,.T.);
#10068=EDGE_CURVE('',#8085,#8170,#5070,.T.);
#10069=EDGE_CURVE('',#8171,#8170,#7057,.T.);
#10070=EDGE_CURVE('',#8171,#8086,#5071,.T.);
#10071=EDGE_CURVE('',#8172,#8171,#195,.T.);
#10072=EDGE_CURVE('',#8087,#8172,#5072,.T.);
#10073=EDGE_CURVE('',#8173,#8172,#5073,.T.);
#10074=EDGE_CURVE('',#8088,#8173,#5074,.T.);
#10075=EDGE_CURVE('',#8174,#8173,#196,.T.);
#10076=EDGE_CURVE('',#8089,#8174,#5075,.T.);
#10077=EDGE_CURVE('',#8175,#8174,#7058,.T.);
#10078=EDGE_CURVE('',#8175,#8090,#5076,.T.);
#10079=EDGE_CURVE('',#8176,#8175,#197,.T.);
#10080=EDGE_CURVE('',#8091,#8176,#5077,.T.);
#10081=EDGE_CURVE('',#8177,#8176,#5078,.T.);
#10082=EDGE_CURVE('',#8092,#8177,#5079,.T.);
#10083=EDGE_CURVE('',#8178,#8177,#198,.T.);
#10084=EDGE_CURVE('',#8093,#8178,#5080,.T.);
#10085=EDGE_CURVE('',#8179,#8178,#7059,.T.);
#10086=EDGE_CURVE('',#8179,#8094,#5081,.T.);
#10087=EDGE_CURVE('',#8180,#8179,#199,.T.);
#10088=EDGE_CURVE('',#8095,#8180,#5082,.T.);
#10089=EDGE_CURVE('',#8181,#8180,#5083,.T.);
#10090=EDGE_CURVE('',#8096,#8181,#5084,.T.);
#10091=EDGE_CURVE('',#8182,#8181,#200,.T.);
#10092=EDGE_CURVE('',#8097,#8182,#5085,.T.);
#10093=EDGE_CURVE('',#8183,#8182,#7060,.T.);
#10094=EDGE_CURVE('',#8183,#8098,#5086,.T.);
#10095=EDGE_CURVE('',#8184,#8183,#201,.T.);
#10096=EDGE_CURVE('',#8099,#8184,#5087,.T.);
#10097=EDGE_CURVE('',#8185,#8184,#5088,.T.);
#10098=EDGE_CURVE('',#8100,#8185,#5089,.T.);
#10099=EDGE_CURVE('',#8186,#8185,#202,.T.);
#10100=EDGE_CURVE('',#8101,#8186,#5090,.T.);
#10101=EDGE_CURVE('',#8187,#8186,#7061,.T.);
#10102=EDGE_CURVE('',#8187,#8102,#5091,.T.);
#10103=EDGE_CURVE('',#8188,#8187,#203,.T.);
#10104=EDGE_CURVE('',#8103,#8188,#5092,.T.);
#10105=EDGE_CURVE('',#8189,#8188,#5093,.T.);
#10106=EDGE_CURVE('',#8104,#8189,#5094,.T.);
#10107=EDGE_CURVE('',#8190,#8189,#204,.T.);
#10108=EDGE_CURVE('',#8105,#8190,#5095,.T.);
#10109=EDGE_CURVE('',#8191,#8190,#7062,.T.);
#10110=EDGE_CURVE('',#8191,#8106,#5096,.T.);
#10111=EDGE_CURVE('',#8192,#8191,#205,.T.);
#10112=EDGE_CURVE('',#8107,#8192,#5097,.T.);
#10113=EDGE_CURVE('',#8193,#8192,#5098,.T.);
#10114=EDGE_CURVE('',#8108,#8193,#5099,.T.);
#10115=EDGE_CURVE('',#8194,#8193,#206,.T.);
#10116=EDGE_CURVE('',#8109,#8194,#5100,.T.);
#10117=EDGE_CURVE('',#8195,#8194,#7063,.T.);
#10118=EDGE_CURVE('',#8195,#8110,#5101,.T.);
#10119=EDGE_CURVE('',#8196,#8195,#207,.T.);
#10120=EDGE_CURVE('',#8111,#8196,#5102,.T.);
#10121=EDGE_CURVE('',#8197,#8196,#5103,.T.);
#10122=EDGE_CURVE('',#8112,#8197,#5104,.T.);
#10123=EDGE_CURVE('',#8198,#8197,#208,.T.);
#10124=EDGE_CURVE('',#8113,#8198,#5105,.T.);
#10125=EDGE_CURVE('',#8199,#8198,#7064,.T.);
#10126=EDGE_CURVE('',#8199,#8114,#5106,.T.);
#10127=EDGE_CURVE('',#8200,#8199,#209,.T.);
#10128=EDGE_CURVE('',#8115,#8200,#5107,.T.);
#10129=EDGE_CURVE('',#8201,#8200,#5108,.T.);
#10130=EDGE_CURVE('',#8116,#8201,#5109,.T.);
#10131=EDGE_CURVE('',#8202,#8201,#210,.T.);
#10132=EDGE_CURVE('',#8117,#8202,#5110,.T.);
#10133=EDGE_CURVE('',#8123,#8202,#7065,.T.);
#10134=EDGE_CURVE('',#8203,#8204,#5111,.T.);
#10135=EDGE_CURVE('',#8205,#8203,#5112,.T.);
#10136=EDGE_CURVE('',#8206,#8205,#5113,.T.);
#10137=EDGE_CURVE('',#8207,#8206,#5114,.T.);
#10138=EDGE_CURVE('',#8208,#8207,#5115,.T.);
#10139=EDGE_CURVE('',#8209,#8208,#5116,.T.);
#10140=EDGE_CURVE('',#8210,#8209,#5117,.T.);
#10141=EDGE_CURVE('',#8204,#8210,#5118,.T.);
#10142=EDGE_CURVE('',#8207,#8211,#5119,.T.);
#10143=EDGE_CURVE('',#8211,#8212,#5120,.T.);
#10144=EDGE_CURVE('',#8212,#8208,#5121,.T.);
#10145=EDGE_CURVE('',#8213,#8206,#5122,.T.);
#10146=EDGE_CURVE('',#8213,#8211,#5123,.T.);
#10147=EDGE_CURVE('',#8205,#8214,#5124,.T.);
#10148=EDGE_CURVE('',#8214,#8213,#5125,.T.);
#10149=EDGE_CURVE('',#8215,#8203,#5126,.T.);
#10150=EDGE_CURVE('',#8215,#8214,#5127,.T.);
#10151=EDGE_CURVE('',#8216,#8215,#5128,.T.);
#10152=EDGE_CURVE('',#8217,#8216,#5129,.T.);
#10153=EDGE_CURVE('',#8218,#8217,#5130,.T.);
#10154=EDGE_CURVE('',#8212,#8218,#5131,.T.);
#10155=EDGE_CURVE('',#8204,#8216,#5132,.T.);
#10156=EDGE_CURVE('',#8217,#8210,#5133,.T.);
#10157=EDGE_CURVE('',#8209,#8218,#5134,.T.);
#10158=EDGE_CURVE('',#8219,#8219,#7066,.T.);
#10159=EDGE_CURVE('',#8219,#8220,#5135,.T.);
#10160=EDGE_CURVE('',#8220,#8220,#7067,.T.);
#10161=EDGE_CURVE('',#8221,#8222,#5136,.T.);
#10162=EDGE_CURVE('',#8221,#8223,#5137,.T.);
#10163=EDGE_CURVE('',#8224,#8223,#5138,.T.);
#10164=EDGE_CURVE('',#8224,#8222,#5139,.T.);
#10165=EDGE_CURVE('',#8222,#8225,#7068,.T.);
#10166=EDGE_CURVE('',#8226,#8224,#5140,.T.);
#10167=EDGE_CURVE('',#8225,#8226,#5141,.T.);
#10168=EDGE_CURVE('',#8225,#8227,#5142,.T.);
#10169=EDGE_CURVE('',#8226,#8228,#5143,.T.);
#10170=EDGE_CURVE('',#8228,#8227,#5144,.T.);
#10171=EDGE_CURVE('',#8223,#8228,#5145,.T.);
#10172=EDGE_CURVE('',#8227,#8221,#7069,.T.);
#10173=EDGE_CURVE('',#8229,#8229,#7070,.T.);
#10174=EDGE_CURVE('',#8230,#8230,#7071,.T.);
#10175=EDGE_CURVE('',#8231,#8231,#7072,.T.);
#10176=EDGE_CURVE('',#8232,#8232,#7073,.T.);
#10177=EDGE_CURVE('',#8229,#8231,#5146,.T.);
#10178=EDGE_CURVE('',#8232,#8233,#5147,.T.);
#10179=EDGE_CURVE('',#8233,#8233,#7074,.T.);
#10180=EDGE_CURVE('',#8234,#8234,#7075,.T.);
#10181=EDGE_CURVE('',#8234,#8230,#5148,.T.);
#10182=EDGE_CURVE('',#8235,#8235,#7076,.T.);
#10183=EDGE_CURVE('',#8235,#8236,#5149,.T.);
#10184=EDGE_CURVE('',#8236,#8236,#7077,.T.);
#10185=EDGE_CURVE('',#8237,#8237,#7078,.T.);
#10186=EDGE_CURVE('',#8237,#8238,#5150,.T.);
#10187=EDGE_CURVE('',#8238,#8238,#7079,.T.);
#10188=EDGE_CURVE('',#8239,#8239,#7080,.T.);
#10189=EDGE_CURVE('',#8239,#8240,#5151,.T.);
#10190=EDGE_CURVE('',#8240,#8240,#7081,.T.);
#10191=EDGE_CURVE('',#8241,#8241,#7082,.T.);
#10192=EDGE_CURVE('',#8241,#8242,#5152,.T.);
#10193=EDGE_CURVE('',#8242,#8242,#7083,.T.);
#10194=EDGE_CURVE('',#8243,#8244,#5153,.T.);
#10195=EDGE_CURVE('',#8243,#8244,#7084,.T.);
#10196=EDGE_CURVE('',#8245,#8243,#903,.T.);
#10197=EDGE_CURVE('',#8246,#8245,#7085,.T.);
#10198=EDGE_CURVE('',#8246,#8247,#5154,.T.);
#10199=EDGE_CURVE('',#8248,#8247,#904,.T.);
#10200=EDGE_CURVE('',#8247,#8248,#905,.T.);
#10201=EDGE_CURVE('',#8249,#8246,#7086,.T.);
#10202=EDGE_CURVE('',#8244,#8249,#906,.T.);
#10203=EDGE_CURVE('',#8249,#8245,#5155,.T.);
#10204=EDGE_CURVE('',#8250,#8250,#7087,.T.);
#10205=EDGE_CURVE('',#8250,#8251,#5156,.T.);
#10206=EDGE_CURVE('',#8251,#8251,#7088,.T.);
#10207=EDGE_CURVE('',#8252,#8252,#7089,.T.);
#10208=EDGE_CURVE('',#8252,#8253,#5157,.T.);
#10209=EDGE_CURVE('',#8253,#8253,#7090,.T.);
#10210=EDGE_CURVE('',#8254,#8254,#7091,.T.);
#10211=EDGE_CURVE('',#8254,#8255,#5158,.T.);
#10212=EDGE_CURVE('',#8255,#8255,#7092,.T.);
#10213=EDGE_CURVE('',#8256,#8256,#7093,.T.);
#10214=EDGE_CURVE('',#8256,#8257,#5159,.T.);
#10215=EDGE_CURVE('',#8257,#8257,#7094,.T.);
#10216=EDGE_CURVE('',#8258,#8258,#7095,.T.);
#10217=EDGE_CURVE('',#8258,#8259,#5160,.T.);
#10218=EDGE_CURVE('',#8259,#8259,#7096,.T.);
#10219=EDGE_CURVE('',#8260,#8260,#7097,.T.);
#10220=EDGE_CURVE('',#8260,#8261,#5161,.T.);
#10221=EDGE_CURVE('',#8261,#8261,#7098,.T.);
#10222=EDGE_CURVE('',#8262,#8263,#5162,.T.);
#10223=EDGE_CURVE('',#8262,#8263,#7099,.T.);
#10224=EDGE_CURVE('',#8264,#8262,#907,.T.);
#10225=EDGE_CURVE('',#8265,#8264,#7100,.T.);
#10226=EDGE_CURVE('',#8265,#8266,#5163,.T.);
#10227=EDGE_CURVE('',#8267,#8266,#908,.T.);
#10228=EDGE_CURVE('',#8266,#8267,#909,.T.);
#10229=EDGE_CURVE('',#8268,#8265,#7101,.T.);
#10230=EDGE_CURVE('',#8263,#8268,#910,.T.);
#10231=EDGE_CURVE('',#8268,#8264,#5164,.T.);
#10232=EDGE_CURVE('',#8269,#8270,#5165,.T.);
#10233=EDGE_CURVE('',#8269,#8271,#5166,.T.);
#10234=EDGE_CURVE('',#8271,#8272,#5167,.T.);
#10235=EDGE_CURVE('',#8270,#8272,#5168,.T.);
#10236=EDGE_CURVE('',#8273,#8269,#7102,.T.);
#10237=EDGE_CURVE('',#8271,#8273,#5169,.T.);
#10238=EDGE_CURVE('',#8270,#8274,#7103,.T.);
#10239=EDGE_CURVE('',#8272,#8274,#5170,.T.);
#10240=EDGE_CURVE('',#8274,#8273,#5171,.T.);
#10241=EDGE_CURVE('',#8275,#8275,#7104,.T.);
#10242=EDGE_CURVE('',#8275,#8276,#5172,.T.);
#10243=EDGE_CURVE('',#8276,#8276,#7105,.T.);
#10244=EDGE_CURVE('',#8277,#8277,#7106,.T.);
#10245=EDGE_CURVE('',#8277,#8278,#5173,.T.);
#10246=EDGE_CURVE('',#8278,#8278,#7107,.T.);
#10247=EDGE_CURVE('',#8279,#8279,#7108,.T.);
#10248=EDGE_CURVE('',#8279,#8280,#5174,.T.);
#10249=EDGE_CURVE('',#8280,#8280,#7109,.T.);
#10250=EDGE_CURVE('',#8281,#8281,#7110,.T.);
#10251=EDGE_CURVE('',#8281,#8282,#5175,.T.);
#10252=EDGE_CURVE('',#8282,#8282,#7111,.T.);
#10253=EDGE_CURVE('',#8283,#8284,#5176,.T.);
#10254=EDGE_CURVE('',#8285,#8283,#5177,.T.);
#10255=EDGE_CURVE('',#8286,#8285,#5178,.T.);
#10256=EDGE_CURVE('',#8284,#8286,#5179,.T.);
#10257=EDGE_CURVE('',#8287,#8283,#5180,.T.);
#10258=EDGE_CURVE('',#8287,#8288,#5181,.T.);
#10259=EDGE_CURVE('',#8285,#8288,#5182,.T.);
#10260=EDGE_CURVE('',#8289,#8287,#5183,.T.);
#10261=EDGE_CURVE('',#8290,#8289,#5184,.T.);
#10262=EDGE_CURVE('',#8288,#8290,#5185,.T.);
#10263=EDGE_CURVE('',#8291,#8292,#7112,.T.);
#10264=EDGE_CURVE('',#8292,#8293,#211,.T.);
#10265=EDGE_CURVE('',#8293,#8294,#5186,.T.);
#10266=EDGE_CURVE('',#8294,#8295,#212,.T.);
#10267=EDGE_CURVE('',#8295,#8296,#7113,.T.);
#10268=EDGE_CURVE('',#8296,#8297,#213,.T.);
#10269=EDGE_CURVE('',#8297,#8298,#5187,.T.);
#10270=EDGE_CURVE('',#8298,#8299,#214,.T.);
#10271=EDGE_CURVE('',#8299,#8300,#7114,.T.);
#10272=EDGE_CURVE('',#8300,#8301,#215,.T.);
#10273=EDGE_CURVE('',#8301,#8302,#5188,.T.);
#10274=EDGE_CURVE('',#8302,#8303,#216,.T.);
#10275=EDGE_CURVE('',#8303,#8304,#7115,.T.);
#10276=EDGE_CURVE('',#8304,#8305,#217,.T.);
#10277=EDGE_CURVE('',#8305,#8306,#5189,.T.);
#10278=EDGE_CURVE('',#8306,#8307,#218,.T.);
#10279=EDGE_CURVE('',#8307,#8308,#7116,.T.);
#10280=EDGE_CURVE('',#8308,#8309,#219,.T.);
#10281=EDGE_CURVE('',#8309,#8310,#5190,.T.);
#10282=EDGE_CURVE('',#8310,#8311,#220,.T.);
#10283=EDGE_CURVE('',#8311,#8312,#7117,.T.);
#10284=EDGE_CURVE('',#8312,#8313,#221,.T.);
#10285=EDGE_CURVE('',#8313,#8314,#5191,.T.);
#10286=EDGE_CURVE('',#8314,#8315,#222,.T.);
#10287=EDGE_CURVE('',#8315,#8316,#7118,.T.);
#10288=EDGE_CURVE('',#8316,#8317,#223,.T.);
#10289=EDGE_CURVE('',#8317,#8318,#5192,.T.);
#10290=EDGE_CURVE('',#8318,#8319,#224,.T.);
#10291=EDGE_CURVE('',#8319,#8320,#7119,.T.);
#10292=EDGE_CURVE('',#8320,#8321,#225,.T.);
#10293=EDGE_CURVE('',#8321,#8322,#5193,.T.);
#10294=EDGE_CURVE('',#8322,#8323,#226,.T.);
#10295=EDGE_CURVE('',#8323,#8324,#7120,.T.);
#10296=EDGE_CURVE('',#8324,#8325,#227,.T.);
#10297=EDGE_CURVE('',#8325,#8326,#5194,.T.);
#10298=EDGE_CURVE('',#8326,#8327,#228,.T.);
#10299=EDGE_CURVE('',#8327,#8328,#7121,.T.);
#10300=EDGE_CURVE('',#8328,#8329,#229,.T.);
#10301=EDGE_CURVE('',#8329,#8330,#5195,.T.);
#10302=EDGE_CURVE('',#8330,#8331,#230,.T.);
#10303=EDGE_CURVE('',#8331,#8332,#7122,.T.);
#10304=EDGE_CURVE('',#8332,#8333,#231,.T.);
#10305=EDGE_CURVE('',#8333,#8334,#5196,.T.);
#10306=EDGE_CURVE('',#8334,#8335,#232,.T.);
#10307=EDGE_CURVE('',#8335,#8336,#7123,.T.);
#10308=EDGE_CURVE('',#8336,#8337,#233,.T.);
#10309=EDGE_CURVE('',#8337,#8338,#5197,.T.);
#10310=EDGE_CURVE('',#8338,#8339,#234,.T.);
#10311=EDGE_CURVE('',#8339,#8340,#7124,.T.);
#10312=EDGE_CURVE('',#8340,#8341,#235,.T.);
#10313=EDGE_CURVE('',#8341,#8342,#5198,.T.);
#10314=EDGE_CURVE('',#8342,#8343,#236,.T.);
#10315=EDGE_CURVE('',#8343,#8344,#7125,.T.);
#10316=EDGE_CURVE('',#8344,#8345,#237,.T.);
#10317=EDGE_CURVE('',#8345,#8346,#5199,.T.);
#10318=EDGE_CURVE('',#8346,#8347,#238,.T.);
#10319=EDGE_CURVE('',#8347,#8348,#7126,.T.);
#10320=EDGE_CURVE('',#8348,#8349,#239,.T.);
#10321=EDGE_CURVE('',#8349,#8350,#5200,.T.);
#10322=EDGE_CURVE('',#8350,#8351,#240,.T.);
#10323=EDGE_CURVE('',#8351,#8352,#7127,.T.);
#10324=EDGE_CURVE('',#8352,#8353,#241,.T.);
#10325=EDGE_CURVE('',#8353,#8354,#5201,.T.);
#10326=EDGE_CURVE('',#8354,#8355,#242,.T.);
#10327=EDGE_CURVE('',#8355,#8356,#7128,.T.);
#10328=EDGE_CURVE('',#8356,#8357,#243,.T.);
#10329=EDGE_CURVE('',#8357,#8358,#5202,.T.);
#10330=EDGE_CURVE('',#8358,#8359,#244,.T.);
#10331=EDGE_CURVE('',#8359,#8360,#7129,.T.);
#10332=EDGE_CURVE('',#8360,#8361,#245,.T.);
#10333=EDGE_CURVE('',#8361,#8362,#5203,.T.);
#10334=EDGE_CURVE('',#8362,#8363,#246,.T.);
#10335=EDGE_CURVE('',#8363,#8364,#7130,.T.);
#10336=EDGE_CURVE('',#8364,#8365,#247,.T.);
#10337=EDGE_CURVE('',#8365,#8366,#5204,.T.);
#10338=EDGE_CURVE('',#8366,#8367,#248,.T.);
#10339=EDGE_CURVE('',#8367,#8368,#7131,.T.);
#10340=EDGE_CURVE('',#8368,#8369,#249,.T.);
#10341=EDGE_CURVE('',#8369,#8370,#5205,.T.);
#10342=EDGE_CURVE('',#8370,#8371,#250,.T.);
#10343=EDGE_CURVE('',#8371,#8372,#7132,.T.);
#10344=EDGE_CURVE('',#8372,#8373,#251,.T.);
#10345=EDGE_CURVE('',#8373,#8374,#5206,.T.);
#10346=EDGE_CURVE('',#8374,#8375,#252,.T.);
#10347=EDGE_CURVE('',#8375,#8376,#7133,.T.);
#10348=EDGE_CURVE('',#8376,#8377,#253,.T.);
#10349=EDGE_CURVE('',#8377,#8378,#5207,.T.);
#10350=EDGE_CURVE('',#8378,#8379,#254,.T.);
#10351=EDGE_CURVE('',#8379,#8380,#7134,.T.);
#10352=EDGE_CURVE('',#8380,#8381,#255,.T.);
#10353=EDGE_CURVE('',#8381,#8382,#5208,.T.);
#10354=EDGE_CURVE('',#8382,#8383,#256,.T.);
#10355=EDGE_CURVE('',#8383,#8384,#7135,.T.);
#10356=EDGE_CURVE('',#8384,#8385,#257,.T.);
#10357=EDGE_CURVE('',#8385,#8386,#5209,.T.);
#10358=EDGE_CURVE('',#8386,#8387,#258,.T.);
#10359=EDGE_CURVE('',#8387,#8388,#7136,.T.);
#10360=EDGE_CURVE('',#8388,#8389,#259,.T.);
#10361=EDGE_CURVE('',#8389,#8390,#5210,.T.);
#10362=EDGE_CURVE('',#8390,#8391,#260,.T.);
#10363=EDGE_CURVE('',#8391,#8392,#7137,.T.);
#10364=EDGE_CURVE('',#8392,#8393,#261,.T.);
#10365=EDGE_CURVE('',#8393,#8394,#5211,.T.);
#10366=EDGE_CURVE('',#8394,#8395,#262,.T.);
#10367=EDGE_CURVE('',#8395,#8396,#7138,.T.);
#10368=EDGE_CURVE('',#8396,#8397,#263,.T.);
#10369=EDGE_CURVE('',#8397,#8398,#5212,.T.);
#10370=EDGE_CURVE('',#8398,#8399,#264,.T.);
#10371=EDGE_CURVE('',#8399,#8400,#7139,.T.);
#10372=EDGE_CURVE('',#8400,#8401,#265,.T.);
#10373=EDGE_CURVE('',#8401,#8402,#5213,.T.);
#10374=EDGE_CURVE('',#8402,#8403,#266,.T.);
#10375=EDGE_CURVE('',#8403,#8404,#7140,.T.);
#10376=EDGE_CURVE('',#8404,#8405,#267,.T.);
#10377=EDGE_CURVE('',#8405,#8406,#5214,.T.);
#10378=EDGE_CURVE('',#8406,#8407,#268,.T.);
#10379=EDGE_CURVE('',#8407,#8408,#7141,.T.);
#10380=EDGE_CURVE('',#8408,#8409,#269,.T.);
#10381=EDGE_CURVE('',#8409,#8410,#5215,.T.);
#10382=EDGE_CURVE('',#8410,#8411,#270,.T.);
#10383=EDGE_CURVE('',#8411,#8412,#7142,.T.);
#10384=EDGE_CURVE('',#8412,#8413,#271,.T.);
#10385=EDGE_CURVE('',#8413,#8414,#5216,.T.);
#10386=EDGE_CURVE('',#8414,#8415,#272,.T.);
#10387=EDGE_CURVE('',#8415,#8416,#7143,.T.);
#10388=EDGE_CURVE('',#8416,#8417,#273,.T.);
#10389=EDGE_CURVE('',#8417,#8418,#5217,.T.);
#10390=EDGE_CURVE('',#8418,#8419,#274,.T.);
#10391=EDGE_CURVE('',#8419,#8420,#7144,.T.);
#10392=EDGE_CURVE('',#8420,#8421,#275,.T.);
#10393=EDGE_CURVE('',#8421,#8422,#5218,.T.);
#10394=EDGE_CURVE('',#8422,#8423,#276,.T.);
#10395=EDGE_CURVE('',#8423,#8424,#7145,.T.);
#10396=EDGE_CURVE('',#8424,#8425,#277,.T.);
#10397=EDGE_CURVE('',#8425,#8426,#5219,.T.);
#10398=EDGE_CURVE('',#8426,#8427,#278,.T.);
#10399=EDGE_CURVE('',#8427,#8428,#7146,.T.);
#10400=EDGE_CURVE('',#8428,#8429,#279,.T.);
#10401=EDGE_CURVE('',#8429,#8430,#5220,.T.);
#10402=EDGE_CURVE('',#8430,#8431,#280,.T.);
#10403=EDGE_CURVE('',#8431,#8432,#7147,.T.);
#10404=EDGE_CURVE('',#8432,#8433,#281,.T.);
#10405=EDGE_CURVE('',#8433,#8434,#5221,.T.);
#10406=EDGE_CURVE('',#8434,#8435,#282,.T.);
#10407=EDGE_CURVE('',#8435,#8436,#7148,.T.);
#10408=EDGE_CURVE('',#8436,#8437,#283,.T.);
#10409=EDGE_CURVE('',#8437,#8438,#5222,.T.);
#10410=EDGE_CURVE('',#8438,#8439,#284,.T.);
#10411=EDGE_CURVE('',#8439,#8440,#7149,.T.);
#10412=EDGE_CURVE('',#8440,#8441,#285,.T.);
#10413=EDGE_CURVE('',#8441,#8442,#5223,.T.);
#10414=EDGE_CURVE('',#8442,#8443,#286,.T.);
#10415=EDGE_CURVE('',#8443,#8444,#7150,.T.);
#10416=EDGE_CURVE('',#8444,#8445,#287,.T.);
#10417=EDGE_CURVE('',#8445,#8446,#5224,.T.);
#10418=EDGE_CURVE('',#8446,#8447,#288,.T.);
#10419=EDGE_CURVE('',#8447,#8448,#7151,.T.);
#10420=EDGE_CURVE('',#8448,#8449,#289,.T.);
#10421=EDGE_CURVE('',#8449,#8450,#5225,.T.);
#10422=EDGE_CURVE('',#8450,#8291,#290,.T.);
#10423=EDGE_CURVE('',#8290,#8286,#7152,.T.);
#10424=EDGE_CURVE('',#8284,#8289,#7153,.T.);
#10425=EDGE_CURVE('',#8451,#8451,#7154,.T.);
#10426=EDGE_CURVE('',#8451,#8452,#5226,.T.);
#10427=EDGE_CURVE('',#8452,#8452,#7155,.T.);
#10428=EDGE_CURVE('',#8453,#8448,#911,.T.);
#10429=EDGE_CURVE('',#8454,#8453,#291,.T.);
#10430=EDGE_CURVE('',#8449,#8454,#5227,.T.);
#10431=EDGE_CURVE('',#8291,#8455,#912,.T.);
#10432=EDGE_CURVE('',#8450,#8456,#5228,.T.);
#10433=EDGE_CURVE('',#8455,#8456,#292,.T.);
#10434=EDGE_CURVE('',#8456,#8454,#5229,.T.);
#10435=EDGE_CURVE('',#8457,#8455,#7156,.T.);
#10436=EDGE_CURVE('',#8457,#8292,#913,.T.);
#10437=EDGE_CURVE('',#8458,#8457,#293,.T.);
#10438=EDGE_CURVE('',#8293,#8458,#5230,.T.);
#10439=EDGE_CURVE('',#8295,#8459,#914,.T.);
#10440=EDGE_CURVE('',#8294,#8460,#5231,.T.);
#10441=EDGE_CURVE('',#8459,#8460,#294,.T.);
#10442=EDGE_CURVE('',#8460,#8458,#5232,.T.);
#10443=EDGE_CURVE('',#8461,#8459,#7157,.T.);
#10444=EDGE_CURVE('',#8461,#8296,#915,.T.);
#10445=EDGE_CURVE('',#8462,#8461,#295,.T.);
#10446=EDGE_CURVE('',#8297,#8462,#5233,.T.);
#10447=EDGE_CURVE('',#8299,#8463,#916,.T.);
#10448=EDGE_CURVE('',#8298,#8464,#5234,.T.);
#10449=EDGE_CURVE('',#8463,#8464,#296,.T.);
#10450=EDGE_CURVE('',#8464,#8462,#5235,.T.);
#10451=EDGE_CURVE('',#8465,#8463,#7158,.T.);
#10452=EDGE_CURVE('',#8465,#8300,#917,.T.);
#10453=EDGE_CURVE('',#8466,#8465,#297,.T.);
#10454=EDGE_CURVE('',#8301,#8466,#5236,.T.);
#10455=EDGE_CURVE('',#8303,#8467,#918,.T.);
#10456=EDGE_CURVE('',#8302,#8468,#5237,.T.);
#10457=EDGE_CURVE('',#8467,#8468,#298,.T.);
#10458=EDGE_CURVE('',#8468,#8466,#5238,.T.);
#10459=EDGE_CURVE('',#8469,#8467,#7159,.T.);
#10460=EDGE_CURVE('',#8469,#8304,#919,.T.);
#10461=EDGE_CURVE('',#8470,#8469,#299,.T.);
#10462=EDGE_CURVE('',#8305,#8470,#5239,.T.);
#10463=EDGE_CURVE('',#8307,#8471,#920,.T.);
#10464=EDGE_CURVE('',#8306,#8472,#5240,.T.);
#10465=EDGE_CURVE('',#8471,#8472,#300,.T.);
#10466=EDGE_CURVE('',#8472,#8470,#5241,.T.);
#10467=EDGE_CURVE('',#8473,#8471,#7160,.T.);
#10468=EDGE_CURVE('',#8473,#8308,#921,.T.);
#10469=EDGE_CURVE('',#8474,#8473,#301,.T.);
#10470=EDGE_CURVE('',#8309,#8474,#5242,.T.);
#10471=EDGE_CURVE('',#8311,#8475,#922,.T.);
#10472=EDGE_CURVE('',#8310,#8476,#5243,.T.);
#10473=EDGE_CURVE('',#8475,#8476,#302,.T.);
#10474=EDGE_CURVE('',#8476,#8474,#5244,.T.);
#10475=EDGE_CURVE('',#8477,#8475,#7161,.T.);
#10476=EDGE_CURVE('',#8477,#8312,#923,.T.);
#10477=EDGE_CURVE('',#8478,#8477,#303,.T.);
#10478=EDGE_CURVE('',#8313,#8478,#5245,.T.);
#10479=EDGE_CURVE('',#8315,#8479,#924,.T.);
#10480=EDGE_CURVE('',#8314,#8480,#5246,.T.);
#10481=EDGE_CURVE('',#8479,#8480,#304,.T.);
#10482=EDGE_CURVE('',#8480,#8478,#5247,.T.);
#10483=EDGE_CURVE('',#8481,#8479,#7162,.T.);
#10484=EDGE_CURVE('',#8481,#8316,#925,.T.);
#10485=EDGE_CURVE('',#8482,#8481,#305,.T.);
#10486=EDGE_CURVE('',#8317,#8482,#5248,.T.);
#10487=EDGE_CURVE('',#8319,#8483,#926,.T.);
#10488=EDGE_CURVE('',#8318,#8484,#5249,.T.);
#10489=EDGE_CURVE('',#8483,#8484,#306,.T.);
#10490=EDGE_CURVE('',#8484,#8482,#5250,.T.);
#10491=EDGE_CURVE('',#8485,#8483,#7163,.T.);
#10492=EDGE_CURVE('',#8485,#8320,#927,.T.);
#10493=EDGE_CURVE('',#8486,#8485,#307,.T.);
#10494=EDGE_CURVE('',#8321,#8486,#5251,.T.);
#10495=EDGE_CURVE('',#8323,#8487,#928,.T.);
#10496=EDGE_CURVE('',#8322,#8488,#5252,.T.);
#10497=EDGE_CURVE('',#8487,#8488,#308,.T.);
#10498=EDGE_CURVE('',#8488,#8486,#5253,.T.);
#10499=EDGE_CURVE('',#8489,#8487,#7164,.T.);
#10500=EDGE_CURVE('',#8489,#8324,#929,.T.);
#10501=EDGE_CURVE('',#8490,#8489,#309,.T.);
#10502=EDGE_CURVE('',#8325,#8490,#5254,.T.);
#10503=EDGE_CURVE('',#8327,#8491,#930,.T.);
#10504=EDGE_CURVE('',#8326,#8492,#5255,.T.);
#10505=EDGE_CURVE('',#8491,#8492,#310,.T.);
#10506=EDGE_CURVE('',#8492,#8490,#5256,.T.);
#10507=EDGE_CURVE('',#8493,#8491,#7165,.T.);
#10508=EDGE_CURVE('',#8493,#8328,#931,.T.);
#10509=EDGE_CURVE('',#8494,#8493,#311,.T.);
#10510=EDGE_CURVE('',#8329,#8494,#5257,.T.);
#10511=EDGE_CURVE('',#8331,#8495,#932,.T.);
#10512=EDGE_CURVE('',#8330,#8496,#5258,.T.);
#10513=EDGE_CURVE('',#8495,#8496,#312,.T.);
#10514=EDGE_CURVE('',#8496,#8494,#5259,.T.);
#10515=EDGE_CURVE('',#8497,#8495,#7166,.T.);
#10516=EDGE_CURVE('',#8497,#8332,#933,.T.);
#10517=EDGE_CURVE('',#8498,#8497,#313,.T.);
#10518=EDGE_CURVE('',#8333,#8498,#5260,.T.);
#10519=EDGE_CURVE('',#8335,#8499,#934,.T.);
#10520=EDGE_CURVE('',#8334,#8500,#5261,.T.);
#10521=EDGE_CURVE('',#8499,#8500,#314,.T.);
#10522=EDGE_CURVE('',#8500,#8498,#5262,.T.);
#10523=EDGE_CURVE('',#8501,#8499,#7167,.T.);
#10524=EDGE_CURVE('',#8501,#8336,#935,.T.);
#10525=EDGE_CURVE('',#8502,#8501,#315,.T.);
#10526=EDGE_CURVE('',#8337,#8502,#5263,.T.);
#10527=EDGE_CURVE('',#8339,#8503,#936,.T.);
#10528=EDGE_CURVE('',#8338,#8504,#5264,.T.);
#10529=EDGE_CURVE('',#8503,#8504,#316,.T.);
#10530=EDGE_CURVE('',#8504,#8502,#5265,.T.);
#10531=EDGE_CURVE('',#8505,#8503,#7168,.T.);
#10532=EDGE_CURVE('',#8505,#8340,#937,.T.);
#10533=EDGE_CURVE('',#8506,#8505,#317,.T.);
#10534=EDGE_CURVE('',#8341,#8506,#5266,.T.);
#10535=EDGE_CURVE('',#8343,#8507,#938,.T.);
#10536=EDGE_CURVE('',#8342,#8508,#5267,.T.);
#10537=EDGE_CURVE('',#8507,#8508,#318,.T.);
#10538=EDGE_CURVE('',#8508,#8506,#5268,.T.);
#10539=EDGE_CURVE('',#8509,#8507,#7169,.T.);
#10540=EDGE_CURVE('',#8509,#8344,#939,.T.);
#10541=EDGE_CURVE('',#8510,#8509,#319,.T.);
#10542=EDGE_CURVE('',#8345,#8510,#5269,.T.);
#10543=EDGE_CURVE('',#8347,#8511,#940,.T.);
#10544=EDGE_CURVE('',#8346,#8512,#5270,.T.);
#10545=EDGE_CURVE('',#8511,#8512,#320,.T.);
#10546=EDGE_CURVE('',#8512,#8510,#5271,.T.);
#10547=EDGE_CURVE('',#8513,#8511,#7170,.T.);
#10548=EDGE_CURVE('',#8513,#8348,#941,.T.);
#10549=EDGE_CURVE('',#8514,#8513,#321,.T.);
#10550=EDGE_CURVE('',#8349,#8514,#5272,.T.);
#10551=EDGE_CURVE('',#8351,#8515,#942,.T.);
#10552=EDGE_CURVE('',#8350,#8516,#5273,.T.);
#10553=EDGE_CURVE('',#8515,#8516,#322,.T.);
#10554=EDGE_CURVE('',#8516,#8514,#5274,.T.);
#10555=EDGE_CURVE('',#8517,#8515,#7171,.T.);
#10556=EDGE_CURVE('',#8517,#8352,#943,.T.);
#10557=EDGE_CURVE('',#8518,#8517,#323,.T.);
#10558=EDGE_CURVE('',#8353,#8518,#5275,.T.);
#10559=EDGE_CURVE('',#8355,#8519,#944,.T.);
#10560=EDGE_CURVE('',#8354,#8520,#5276,.T.);
#10561=EDGE_CURVE('',#8519,#8520,#324,.T.);
#10562=EDGE_CURVE('',#8520,#8518,#5277,.T.);
#10563=EDGE_CURVE('',#8521,#8519,#7172,.T.);
#10564=EDGE_CURVE('',#8521,#8356,#945,.T.);
#10565=EDGE_CURVE('',#8522,#8521,#325,.T.);
#10566=EDGE_CURVE('',#8357,#8522,#5278,.T.);
#10567=EDGE_CURVE('',#8359,#8523,#946,.T.);
#10568=EDGE_CURVE('',#8358,#8524,#5279,.T.);
#10569=EDGE_CURVE('',#8523,#8524,#326,.T.);
#10570=EDGE_CURVE('',#8524,#8522,#5280,.T.);
#10571=EDGE_CURVE('',#8525,#8523,#7173,.T.);
#10572=EDGE_CURVE('',#8525,#8360,#947,.T.);
#10573=EDGE_CURVE('',#8526,#8525,#327,.T.);
#10574=EDGE_CURVE('',#8361,#8526,#5281,.T.);
#10575=EDGE_CURVE('',#8363,#8527,#948,.T.);
#10576=EDGE_CURVE('',#8362,#8528,#5282,.T.);
#10577=EDGE_CURVE('',#8527,#8528,#328,.T.);
#10578=EDGE_CURVE('',#8528,#8526,#5283,.T.);
#10579=EDGE_CURVE('',#8529,#8527,#7174,.T.);
#10580=EDGE_CURVE('',#8529,#8364,#949,.T.);
#10581=EDGE_CURVE('',#8530,#8529,#329,.T.);
#10582=EDGE_CURVE('',#8365,#8530,#5284,.T.);
#10583=EDGE_CURVE('',#8367,#8531,#950,.T.);
#10584=EDGE_CURVE('',#8366,#8532,#5285,.T.);
#10585=EDGE_CURVE('',#8531,#8532,#330,.T.);
#10586=EDGE_CURVE('',#8532,#8530,#5286,.T.);
#10587=EDGE_CURVE('',#8533,#8531,#7175,.T.);
#10588=EDGE_CURVE('',#8533,#8368,#951,.T.);
#10589=EDGE_CURVE('',#8534,#8533,#331,.T.);
#10590=EDGE_CURVE('',#8369,#8534,#5287,.T.);
#10591=EDGE_CURVE('',#8371,#8535,#952,.T.);
#10592=EDGE_CURVE('',#8370,#8536,#5288,.T.);
#10593=EDGE_CURVE('',#8535,#8536,#332,.T.);
#10594=EDGE_CURVE('',#8536,#8534,#5289,.T.);
#10595=EDGE_CURVE('',#8537,#8535,#7176,.T.);
#10596=EDGE_CURVE('',#8537,#8372,#953,.T.);
#10597=EDGE_CURVE('',#8538,#8537,#333,.T.);
#10598=EDGE_CURVE('',#8373,#8538,#5290,.T.);
#10599=EDGE_CURVE('',#8375,#8539,#954,.T.);
#10600=EDGE_CURVE('',#8374,#8540,#5291,.T.);
#10601=EDGE_CURVE('',#8539,#8540,#334,.T.);
#10602=EDGE_CURVE('',#8540,#8538,#5292,.T.);
#10603=EDGE_CURVE('',#8541,#8539,#7177,.T.);
#10604=EDGE_CURVE('',#8541,#8376,#955,.T.);
#10605=EDGE_CURVE('',#8542,#8541,#335,.T.);
#10606=EDGE_CURVE('',#8377,#8542,#5293,.T.);
#10607=EDGE_CURVE('',#8379,#8543,#956,.T.);
#10608=EDGE_CURVE('',#8378,#8544,#5294,.T.);
#10609=EDGE_CURVE('',#8543,#8544,#336,.T.);
#10610=EDGE_CURVE('',#8544,#8542,#5295,.T.);
#10611=EDGE_CURVE('',#8545,#8543,#7178,.T.);
#10612=EDGE_CURVE('',#8545,#8380,#957,.T.);
#10613=EDGE_CURVE('',#8546,#8545,#337,.T.);
#10614=EDGE_CURVE('',#8381,#8546,#5296,.T.);
#10615=EDGE_CURVE('',#8383,#8547,#958,.T.);
#10616=EDGE_CURVE('',#8382,#8548,#5297,.T.);
#10617=EDGE_CURVE('',#8547,#8548,#338,.T.);
#10618=EDGE_CURVE('',#8548,#8546,#5298,.T.);
#10619=EDGE_CURVE('',#8549,#8547,#7179,.T.);
#10620=EDGE_CURVE('',#8549,#8384,#959,.T.);
#10621=EDGE_CURVE('',#8550,#8549,#339,.T.);
#10622=EDGE_CURVE('',#8385,#8550,#5299,.T.);
#10623=EDGE_CURVE('',#8387,#8551,#960,.T.);
#10624=EDGE_CURVE('',#8386,#8552,#5300,.T.);
#10625=EDGE_CURVE('',#8551,#8552,#340,.T.);
#10626=EDGE_CURVE('',#8552,#8550,#5301,.T.);
#10627=EDGE_CURVE('',#8553,#8551,#7180,.T.);
#10628=EDGE_CURVE('',#8553,#8388,#961,.T.);
#10629=EDGE_CURVE('',#8554,#8553,#341,.T.);
#10630=EDGE_CURVE('',#8389,#8554,#5302,.T.);
#10631=EDGE_CURVE('',#8391,#8555,#962,.T.);
#10632=EDGE_CURVE('',#8390,#8556,#5303,.T.);
#10633=EDGE_CURVE('',#8555,#8556,#342,.T.);
#10634=EDGE_CURVE('',#8556,#8554,#5304,.T.);
#10635=EDGE_CURVE('',#8557,#8555,#7181,.T.);
#10636=EDGE_CURVE('',#8557,#8392,#963,.T.);
#10637=EDGE_CURVE('',#8558,#8557,#343,.T.);
#10638=EDGE_CURVE('',#8393,#8558,#5305,.T.);
#10639=EDGE_CURVE('',#8395,#8559,#964,.T.);
#10640=EDGE_CURVE('',#8394,#8560,#5306,.T.);
#10641=EDGE_CURVE('',#8559,#8560,#344,.T.);
#10642=EDGE_CURVE('',#8560,#8558,#5307,.T.);
#10643=EDGE_CURVE('',#8561,#8559,#7182,.T.);
#10644=EDGE_CURVE('',#8561,#8396,#965,.T.);
#10645=EDGE_CURVE('',#8562,#8561,#345,.T.);
#10646=EDGE_CURVE('',#8397,#8562,#5308,.T.);
#10647=EDGE_CURVE('',#8399,#8563,#966,.T.);
#10648=EDGE_CURVE('',#8398,#8564,#5309,.T.);
#10649=EDGE_CURVE('',#8563,#8564,#346,.T.);
#10650=EDGE_CURVE('',#8564,#8562,#5310,.T.);
#10651=EDGE_CURVE('',#8565,#8563,#7183,.T.);
#10652=EDGE_CURVE('',#8565,#8400,#967,.T.);
#10653=EDGE_CURVE('',#8566,#8565,#347,.T.);
#10654=EDGE_CURVE('',#8401,#8566,#5311,.T.);
#10655=EDGE_CURVE('',#8403,#8567,#968,.T.);
#10656=EDGE_CURVE('',#8402,#8568,#5312,.T.);
#10657=EDGE_CURVE('',#8567,#8568,#348,.T.);
#10658=EDGE_CURVE('',#8568,#8566,#5313,.T.);
#10659=EDGE_CURVE('',#8569,#8567,#7184,.T.);
#10660=EDGE_CURVE('',#8569,#8404,#969,.T.);
#10661=EDGE_CURVE('',#8570,#8569,#349,.T.);
#10662=EDGE_CURVE('',#8405,#8570,#5314,.T.);
#10663=EDGE_CURVE('',#8407,#8571,#970,.T.);
#10664=EDGE_CURVE('',#8406,#8572,#5315,.T.);
#10665=EDGE_CURVE('',#8571,#8572,#350,.T.);
#10666=EDGE_CURVE('',#8572,#8570,#5316,.T.);
#10667=EDGE_CURVE('',#8573,#8571,#7185,.T.);
#10668=EDGE_CURVE('',#8573,#8408,#971,.T.);
#10669=EDGE_CURVE('',#8574,#8573,#351,.T.);
#10670=EDGE_CURVE('',#8409,#8574,#5317,.T.);
#10671=EDGE_CURVE('',#8411,#8575,#972,.T.);
#10672=EDGE_CURVE('',#8410,#8576,#5318,.T.);
#10673=EDGE_CURVE('',#8575,#8576,#352,.T.);
#10674=EDGE_CURVE('',#8576,#8574,#5319,.T.);
#10675=EDGE_CURVE('',#8577,#8575,#7186,.T.);
#10676=EDGE_CURVE('',#8577,#8412,#973,.T.);
#10677=EDGE_CURVE('',#8578,#8577,#353,.T.);
#10678=EDGE_CURVE('',#8413,#8578,#5320,.T.);
#10679=EDGE_CURVE('',#8415,#8579,#974,.T.);
#10680=EDGE_CURVE('',#8414,#8580,#5321,.T.);
#10681=EDGE_CURVE('',#8579,#8580,#354,.T.);
#10682=EDGE_CURVE('',#8580,#8578,#5322,.T.);
#10683=EDGE_CURVE('',#8581,#8579,#7187,.T.);
#10684=EDGE_CURVE('',#8581,#8416,#975,.T.);
#10685=EDGE_CURVE('',#8582,#8581,#355,.T.);
#10686=EDGE_CURVE('',#8417,#8582,#5323,.T.);
#10687=EDGE_CURVE('',#8419,#8583,#976,.T.);
#10688=EDGE_CURVE('',#8418,#8584,#5324,.T.);
#10689=EDGE_CURVE('',#8583,#8584,#356,.T.);
#10690=EDGE_CURVE('',#8584,#8582,#5325,.T.);
#10691=EDGE_CURVE('',#8585,#8583,#7188,.T.);
#10692=EDGE_CURVE('',#8585,#8420,#977,.T.);
#10693=EDGE_CURVE('',#8586,#8585,#357,.T.);
#10694=EDGE_CURVE('',#8421,#8586,#5326,.T.);
#10695=EDGE_CURVE('',#8423,#8587,#978,.T.);
#10696=EDGE_CURVE('',#8422,#8588,#5327,.T.);
#10697=EDGE_CURVE('',#8587,#8588,#358,.T.);
#10698=EDGE_CURVE('',#8588,#8586,#5328,.T.);
#10699=EDGE_CURVE('',#8589,#8587,#7189,.T.);
#10700=EDGE_CURVE('',#8589,#8424,#979,.T.);
#10701=EDGE_CURVE('',#8590,#8589,#359,.T.);
#10702=EDGE_CURVE('',#8425,#8590,#5329,.T.);
#10703=EDGE_CURVE('',#8427,#8591,#980,.T.);
#10704=EDGE_CURVE('',#8426,#8592,#5330,.T.);
#10705=EDGE_CURVE('',#8591,#8592,#360,.T.);
#10706=EDGE_CURVE('',#8592,#8590,#5331,.T.);
#10707=EDGE_CURVE('',#8593,#8591,#7190,.T.);
#10708=EDGE_CURVE('',#8593,#8428,#981,.T.);
#10709=EDGE_CURVE('',#8594,#8593,#361,.T.);
#10710=EDGE_CURVE('',#8429,#8594,#5332,.T.);
#10711=EDGE_CURVE('',#8431,#8595,#982,.T.);
#10712=EDGE_CURVE('',#8430,#8596,#5333,.T.);
#10713=EDGE_CURVE('',#8595,#8596,#362,.T.);
#10714=EDGE_CURVE('',#8596,#8594,#5334,.T.);
#10715=EDGE_CURVE('',#8597,#8595,#7191,.T.);
#10716=EDGE_CURVE('',#8597,#8432,#983,.T.);
#10717=EDGE_CURVE('',#8598,#8597,#363,.T.);
#10718=EDGE_CURVE('',#8433,#8598,#5335,.T.);
#10719=EDGE_CURVE('',#8435,#8599,#984,.T.);
#10720=EDGE_CURVE('',#8434,#8600,#5336,.T.);
#10721=EDGE_CURVE('',#8599,#8600,#364,.T.);
#10722=EDGE_CURVE('',#8600,#8598,#5337,.T.);
#10723=EDGE_CURVE('',#8601,#8599,#7192,.T.);
#10724=EDGE_CURVE('',#8601,#8436,#985,.T.);
#10725=EDGE_CURVE('',#8602,#8601,#365,.T.);
#10726=EDGE_CURVE('',#8437,#8602,#5338,.T.);
#10727=EDGE_CURVE('',#8439,#8603,#986,.T.);
#10728=EDGE_CURVE('',#8438,#8604,#5339,.T.);
#10729=EDGE_CURVE('',#8603,#8604,#366,.T.);
#10730=EDGE_CURVE('',#8604,#8602,#5340,.T.);
#10731=EDGE_CURVE('',#8605,#8603,#7193,.T.);
#10732=EDGE_CURVE('',#8605,#8440,#987,.T.);
#10733=EDGE_CURVE('',#8606,#8605,#367,.T.);
#10734=EDGE_CURVE('',#8441,#8606,#5341,.T.);
#10735=EDGE_CURVE('',#8607,#8606,#5342,.T.);
#10736=EDGE_CURVE('',#8442,#8607,#5343,.T.);
#10737=EDGE_CURVE('',#8443,#8608,#988,.T.);
#10738=EDGE_CURVE('',#8608,#8607,#368,.T.);
#10739=EDGE_CURVE('',#8609,#8608,#7194,.T.);
#10740=EDGE_CURVE('',#8609,#8444,#989,.T.);
#10741=EDGE_CURVE('',#8447,#8610,#990,.T.);
#10742=EDGE_CURVE('',#8446,#8611,#5344,.T.);
#10743=EDGE_CURVE('',#8610,#8611,#369,.T.);
#10744=EDGE_CURVE('',#8612,#8609,#370,.T.);
#10745=EDGE_CURVE('',#8445,#8612,#5345,.T.);
#10746=EDGE_CURVE('',#8611,#8612,#5346,.T.);
#10747=EDGE_CURVE('',#8453,#8610,#7195,.T.);
#10748=EDGE_CURVE('',#8613,#8614,#5347,.T.);
#10749=EDGE_CURVE('',#8615,#8613,#5348,.T.);
#10750=EDGE_CURVE('',#8616,#8615,#5349,.T.);
#10751=EDGE_CURVE('',#8617,#8616,#5350,.T.);
#10752=EDGE_CURVE('',#8618,#8617,#5351,.T.);
#10753=EDGE_CURVE('',#8619,#8618,#5352,.T.);
#10754=EDGE_CURVE('',#8620,#8619,#5353,.T.);
#10755=EDGE_CURVE('',#8614,#8620,#5354,.T.);
#10756=EDGE_CURVE('',#8617,#8621,#5355,.T.);
#10757=EDGE_CURVE('',#8621,#8622,#5356,.T.);
#10758=EDGE_CURVE('',#8622,#8618,#5357,.T.);
#10759=EDGE_CURVE('',#8623,#8616,#5358,.T.);
#10760=EDGE_CURVE('',#8623,#8621,#5359,.T.);
#10761=EDGE_CURVE('',#8615,#8624,#5360,.T.);
#10762=EDGE_CURVE('',#8624,#8623,#5361,.T.);
#10763=EDGE_CURVE('',#8625,#8613,#5362,.T.);
#10764=EDGE_CURVE('',#8625,#8624,#5363,.T.);
#10765=EDGE_CURVE('',#8626,#8627,#5364,.T.);
#10766=EDGE_CURVE('',#8622,#8626,#5365,.T.);
#10767=EDGE_CURVE('',#8628,#8625,#5366,.T.);
#10768=EDGE_CURVE('',#8627,#8628,#5367,.T.);
#10769=EDGE_CURVE('',#8619,#8626,#5368,.T.);
#10770=EDGE_CURVE('',#8614,#8628,#5369,.T.);
#10771=EDGE_CURVE('',#8627,#8620,#5370,.T.);
#10772=EDGE_CURVE('',#8629,#8630,#5371,.T.);
#10773=EDGE_CURVE('',#8629,#8631,#5372,.T.);
#10774=EDGE_CURVE('',#8631,#8632,#5373,.T.);
#10775=EDGE_CURVE('',#8630,#8632,#5374,.T.);
#10776=EDGE_CURVE('',#8633,#8629,#5375,.T.);
#10777=EDGE_CURVE('',#8633,#8634,#5376,.T.);
#10778=EDGE_CURVE('',#8634,#8631,#5377,.T.);
#10779=EDGE_CURVE('',#8635,#8633,#5378,.T.);
#10780=EDGE_CURVE('',#8635,#8636,#5379,.T.);
#10781=EDGE_CURVE('',#8636,#8634,#5380,.T.);
#10782=EDGE_CURVE('',#8637,#8635,#5381,.T.);
#10783=EDGE_CURVE('',#8637,#8638,#5382,.T.);
#10784=EDGE_CURVE('',#8638,#8636,#5383,.T.);
#10785=EDGE_CURVE('',#8639,#8637,#5384,.T.);
#10786=EDGE_CURVE('',#8639,#8640,#5385,.T.);
#10787=EDGE_CURVE('',#8640,#8638,#5386,.T.);
#10788=EDGE_CURVE('',#8630,#8639,#5387,.T.);
#10789=EDGE_CURVE('',#8632,#8640,#5388,.T.);
#10790=EDGE_CURVE('',#8641,#8641,#7196,.T.);
#10791=EDGE_CURVE('',#8642,#8642,#7197,.T.);
#10792=EDGE_CURVE('',#8642,#8641,#5389,.T.);
#10793=EDGE_CURVE('',#8643,#8643,#7198,.F.);
#10794=EDGE_CURVE('',#8643,#8642,#5390,.T.);
#10795=EDGE_CURVE('',#8644,#8644,#7199,.T.);
#10796=EDGE_CURVE('',#8644,#8643,#5391,.T.);
#10797=EDGE_CURVE('',#8645,#8645,#7200,.T.);
#10798=EDGE_CURVE('',#8646,#8646,#7201,.T.);
#10799=EDGE_CURVE('',#8646,#8645,#5392,.T.);
#10800=EDGE_CURVE('',#8647,#8647,#7202,.T.);
#10801=EDGE_CURVE('',#8647,#8646,#5393,.T.);
#10802=EDGE_CURVE('',#8648,#8648,#7203,.T.);
#10803=EDGE_CURVE('',#8648,#8647,#5394,.T.);
#10804=EDGE_CURVE('',#8649,#8649,#7204,.T.);
#10805=EDGE_CURVE('',#8650,#8650,#7205,.F.);
#10806=EDGE_CURVE('',#8650,#8649,#5395,.T.);
#10807=EDGE_CURVE('',#8651,#8651,#7206,.F.);
#10808=EDGE_CURVE('',#8651,#8650,#5396,.T.);
#10809=EDGE_CURVE('',#8652,#8652,#7207,.T.);
#10810=EDGE_CURVE('',#8652,#8651,#5397,.T.);
#10811=EDGE_CURVE('',#8653,#8654,#5398,.T.);
#10812=EDGE_CURVE('',#8654,#8655,#5399,.T.);
#10813=EDGE_CURVE('',#8655,#8656,#5400,.T.);
#10814=EDGE_CURVE('',#8653,#8656,#5401,.T.);
#10815=EDGE_CURVE('',#8654,#8657,#5402,.T.);
#10816=EDGE_CURVE('',#8657,#8658,#5403,.T.);
#10817=EDGE_CURVE('',#8658,#8655,#5404,.T.);
#10818=EDGE_CURVE('',#8657,#8659,#5405,.T.);
#10819=EDGE_CURVE('',#8659,#8660,#5406,.T.);
#10820=EDGE_CURVE('',#8660,#8658,#5407,.T.);
#10821=EDGE_CURVE('',#8659,#8661,#5408,.T.);
#10822=EDGE_CURVE('',#8661,#8662,#5409,.T.);
#10823=EDGE_CURVE('',#8662,#8660,#5410,.T.);
#10824=EDGE_CURVE('',#8661,#8663,#5411,.T.);
#10825=EDGE_CURVE('',#8663,#8664,#5412,.T.);
#10826=EDGE_CURVE('',#8664,#8662,#5413,.T.);
#10827=EDGE_CURVE('',#8663,#8653,#5414,.T.);
#10828=EDGE_CURVE('',#8656,#8664,#5415,.T.);
#10829=EDGE_CURVE('',#8665,#8665,#7208,.T.);
#10830=EDGE_CURVE('',#8665,#8666,#5416,.T.);
#10831=EDGE_CURVE('',#8666,#8666,#7209,.T.);
#10832=EDGE_CURVE('',#8667,#8667,#7210,.T.);
#10833=EDGE_CURVE('',#8667,#8668,#5417,.T.);
#10834=EDGE_CURVE('',#8668,#8668,#7211,.T.);
#10835=ORIENTED_EDGE('',*,*,#8669,.F.);
#10836=ORIENTED_EDGE('',*,*,#8670,.T.);
#10837=ORIENTED_EDGE('',*,*,#8671,.F.);
#10838=ORIENTED_EDGE('',*,*,#8670,.F.);
#10839=ORIENTED_EDGE('',*,*,#8672,.F.);
#10840=ORIENTED_EDGE('',*,*,#8673,.T.);
#10841=ORIENTED_EDGE('',*,*,#8674,.F.);
#10842=ORIENTED_EDGE('',*,*,#8673,.F.);
#10843=ORIENTED_EDGE('',*,*,#8675,.F.);
#10844=ORIENTED_EDGE('',*,*,#8676,.T.);
#10845=ORIENTED_EDGE('',*,*,#8677,.F.);
#10846=ORIENTED_EDGE('',*,*,#8676,.F.);
#10847=ORIENTED_EDGE('',*,*,#8678,.T.);
#10848=ORIENTED_EDGE('',*,*,#8679,.T.);
#10849=ORIENTED_EDGE('',*,*,#8680,.F.);
#10850=ORIENTED_EDGE('',*,*,#8681,.F.);
#10851=ORIENTED_EDGE('',*,*,#8682,.T.);
#10852=ORIENTED_EDGE('',*,*,#8681,.T.);
#10853=ORIENTED_EDGE('',*,*,#8683,.F.);
#10854=ORIENTED_EDGE('',*,*,#8684,.F.);
#10855=ORIENTED_EDGE('',*,*,#8685,.T.);
#10856=ORIENTED_EDGE('',*,*,#8684,.T.);
#10857=ORIENTED_EDGE('',*,*,#8686,.F.);
#10858=ORIENTED_EDGE('',*,*,#8687,.F.);
#10859=ORIENTED_EDGE('',*,*,#8688,.T.);
#10860=ORIENTED_EDGE('',*,*,#8687,.T.);
#10861=ORIENTED_EDGE('',*,*,#8689,.F.);
#10862=ORIENTED_EDGE('',*,*,#8679,.F.);
#10863=ORIENTED_EDGE('',*,*,#8689,.T.);
#10864=ORIENTED_EDGE('',*,*,#8686,.T.);
#10865=ORIENTED_EDGE('',*,*,#8683,.T.);
#10866=ORIENTED_EDGE('',*,*,#8680,.T.);
#10867=ORIENTED_EDGE('',*,*,#8671,.T.);
#10868=ORIENTED_EDGE('',*,*,#8674,.T.);
#10869=ORIENTED_EDGE('',*,*,#8677,.T.);
#10870=ORIENTED_EDGE('',*,*,#8688,.F.);
#10871=ORIENTED_EDGE('',*,*,#8678,.F.);
#10872=ORIENTED_EDGE('',*,*,#8682,.F.);
#10873=ORIENTED_EDGE('',*,*,#8685,.F.);
#10874=ORIENTED_EDGE('',*,*,#8669,.T.);
#10875=ORIENTED_EDGE('',*,*,#8672,.T.);
#10876=ORIENTED_EDGE('',*,*,#8675,.T.);
#10877=ORIENTED_EDGE('',*,*,#8690,.F.);
#10878=ORIENTED_EDGE('',*,*,#8691,.T.);
#10879=ORIENTED_EDGE('',*,*,#8692,.F.);
#10880=ORIENTED_EDGE('',*,*,#8691,.F.);
#10881=ORIENTED_EDGE('',*,*,#8693,.F.);
#10882=ORIENTED_EDGE('',*,*,#8694,.T.);
#10883=ORIENTED_EDGE('',*,*,#8695,.F.);
#10884=ORIENTED_EDGE('',*,*,#8694,.F.);
#10885=ORIENTED_EDGE('',*,*,#8696,.F.);
#10886=ORIENTED_EDGE('',*,*,#8697,.T.);
#10887=ORIENTED_EDGE('',*,*,#8698,.F.);
#10888=ORIENTED_EDGE('',*,*,#8697,.F.);
#10889=ORIENTED_EDGE('',*,*,#8699,.F.);
#10890=ORIENTED_EDGE('',*,*,#8700,.T.);
#10891=ORIENTED_EDGE('',*,*,#8701,.F.);
#10892=ORIENTED_EDGE('',*,*,#8700,.F.);
#10893=ORIENTED_EDGE('',*,*,#8702,.F.);
#10894=ORIENTED_EDGE('',*,*,#8703,.T.);
#10895=ORIENTED_EDGE('',*,*,#8704,.F.);
#10896=ORIENTED_EDGE('',*,*,#8703,.F.);
#10897=ORIENTED_EDGE('',*,*,#8705,.F.);
#10898=ORIENTED_EDGE('',*,*,#8706,.T.);
#10899=ORIENTED_EDGE('',*,*,#8707,.F.);
#10900=ORIENTED_EDGE('',*,*,#8706,.F.);
#10901=ORIENTED_EDGE('',*,*,#8708,.F.);
#10902=ORIENTED_EDGE('',*,*,#8709,.T.);
#10903=ORIENTED_EDGE('',*,*,#8710,.F.);
#10904=ORIENTED_EDGE('',*,*,#8709,.F.);
#10905=ORIENTED_EDGE('',*,*,#8711,.F.);
#10906=ORIENTED_EDGE('',*,*,#8712,.T.);
#10907=ORIENTED_EDGE('',*,*,#8713,.F.);
#10908=ORIENTED_EDGE('',*,*,#8712,.F.);
#10909=ORIENTED_EDGE('',*,*,#8714,.F.);
#10910=ORIENTED_EDGE('',*,*,#8715,.T.);
#10911=ORIENTED_EDGE('',*,*,#8716,.F.);
#10912=ORIENTED_EDGE('',*,*,#8715,.F.);
#10913=ORIENTED_EDGE('',*,*,#8717,.F.);
#10914=ORIENTED_EDGE('',*,*,#8718,.T.);
#10915=ORIENTED_EDGE('',*,*,#8719,.F.);
#10916=ORIENTED_EDGE('',*,*,#8718,.F.);
#10917=ORIENTED_EDGE('',*,*,#8720,.F.);
#10918=ORIENTED_EDGE('',*,*,#8721,.T.);
#10919=ORIENTED_EDGE('',*,*,#8722,.F.);
#10920=ORIENTED_EDGE('',*,*,#8721,.F.);
#10921=ORIENTED_EDGE('',*,*,#8723,.F.);
#10922=ORIENTED_EDGE('',*,*,#8724,.T.);
#10923=ORIENTED_EDGE('',*,*,#8725,.F.);
#10924=ORIENTED_EDGE('',*,*,#8724,.F.);
#10925=ORIENTED_EDGE('',*,*,#8726,.F.);
#10926=ORIENTED_EDGE('',*,*,#8727,.T.);
#10927=ORIENTED_EDGE('',*,*,#8728,.F.);
#10928=ORIENTED_EDGE('',*,*,#8727,.F.);
#10929=ORIENTED_EDGE('',*,*,#8729,.F.);
#10930=ORIENTED_EDGE('',*,*,#8730,.T.);
#10931=ORIENTED_EDGE('',*,*,#8731,.F.);
#10932=ORIENTED_EDGE('',*,*,#8730,.F.);
#10933=ORIENTED_EDGE('',*,*,#8732,.F.);
#10934=ORIENTED_EDGE('',*,*,#8733,.T.);
#10935=ORIENTED_EDGE('',*,*,#8734,.F.);
#10936=ORIENTED_EDGE('',*,*,#8733,.F.);
#10937=ORIENTED_EDGE('',*,*,#8735,.F.);
#10938=ORIENTED_EDGE('',*,*,#8736,.T.);
#10939=ORIENTED_EDGE('',*,*,#8737,.F.);
#10940=ORIENTED_EDGE('',*,*,#8736,.F.);
#10941=ORIENTED_EDGE('',*,*,#8738,.F.);
#10942=ORIENTED_EDGE('',*,*,#8739,.T.);
#10943=ORIENTED_EDGE('',*,*,#8740,.F.);
#10944=ORIENTED_EDGE('',*,*,#8739,.F.);
#10945=ORIENTED_EDGE('',*,*,#8741,.F.);
#10946=ORIENTED_EDGE('',*,*,#8742,.T.);
#10947=ORIENTED_EDGE('',*,*,#8743,.F.);
#10948=ORIENTED_EDGE('',*,*,#8742,.F.);
#10949=ORIENTED_EDGE('',*,*,#8744,.F.);
#10950=ORIENTED_EDGE('',*,*,#8745,.T.);
#10951=ORIENTED_EDGE('',*,*,#8746,.F.);
#10952=ORIENTED_EDGE('',*,*,#8745,.F.);
#10953=ORIENTED_EDGE('',*,*,#8747,.F.);
#10954=ORIENTED_EDGE('',*,*,#8748,.T.);
#10955=ORIENTED_EDGE('',*,*,#8749,.F.);
#10956=ORIENTED_EDGE('',*,*,#8748,.F.);
#10957=ORIENTED_EDGE('',*,*,#8750,.F.);
#10958=ORIENTED_EDGE('',*,*,#8751,.T.);
#10959=ORIENTED_EDGE('',*,*,#8752,.F.);
#10960=ORIENTED_EDGE('',*,*,#8751,.F.);
#10961=ORIENTED_EDGE('',*,*,#8753,.F.);
#10962=ORIENTED_EDGE('',*,*,#8754,.T.);
#10963=ORIENTED_EDGE('',*,*,#8755,.F.);
#10964=ORIENTED_EDGE('',*,*,#8754,.F.);
#10965=ORIENTED_EDGE('',*,*,#8756,.F.);
#10966=ORIENTED_EDGE('',*,*,#8757,.T.);
#10967=ORIENTED_EDGE('',*,*,#8758,.F.);
#10968=ORIENTED_EDGE('',*,*,#8757,.F.);
#10969=ORIENTED_EDGE('',*,*,#8759,.F.);
#10970=ORIENTED_EDGE('',*,*,#8760,.T.);
#10971=ORIENTED_EDGE('',*,*,#8761,.F.);
#10972=ORIENTED_EDGE('',*,*,#8760,.F.);
#10973=ORIENTED_EDGE('',*,*,#8762,.F.);
#10974=ORIENTED_EDGE('',*,*,#8763,.T.);
#10975=ORIENTED_EDGE('',*,*,#8764,.F.);
#10976=ORIENTED_EDGE('',*,*,#8763,.F.);
#10977=ORIENTED_EDGE('',*,*,#8765,.F.);
#10978=ORIENTED_EDGE('',*,*,#8766,.T.);
#10979=ORIENTED_EDGE('',*,*,#8767,.F.);
#10980=ORIENTED_EDGE('',*,*,#8768,.F.);
#10981=ORIENTED_EDGE('',*,*,#8758,.T.);
#10982=ORIENTED_EDGE('',*,*,#8761,.T.);
#10983=ORIENTED_EDGE('',*,*,#8764,.T.);
#10984=ORIENTED_EDGE('',*,*,#8765,.T.);
#10985=ORIENTED_EDGE('',*,*,#8769,.T.);
#10986=ORIENTED_EDGE('',*,*,#8770,.T.);
#10987=ORIENTED_EDGE('',*,*,#8771,.T.);
#10988=ORIENTED_EDGE('',*,*,#8772,.T.);
#10989=ORIENTED_EDGE('',*,*,#8773,.T.);
#10990=ORIENTED_EDGE('',*,*,#8774,.F.);
#10991=ORIENTED_EDGE('',*,*,#8775,.F.);
#10992=ORIENTED_EDGE('',*,*,#8695,.T.);
#10993=ORIENTED_EDGE('',*,*,#8710,.T.);
#10994=ORIENTED_EDGE('',*,*,#8725,.T.);
#10995=ORIENTED_EDGE('',*,*,#8743,.T.);
#10996=ORIENTED_EDGE('',*,*,#8746,.T.);
#10997=ORIENTED_EDGE('',*,*,#8749,.T.);
#10998=ORIENTED_EDGE('',*,*,#8752,.T.);
#10999=ORIENTED_EDGE('',*,*,#8755,.T.);
#11000=ORIENTED_EDGE('',*,*,#8740,.T.);
#11001=ORIENTED_EDGE('',*,*,#8737,.T.);
#11002=ORIENTED_EDGE('',*,*,#8734,.T.);
#11003=ORIENTED_EDGE('',*,*,#8731,.T.);
#11004=ORIENTED_EDGE('',*,*,#8728,.T.);
#11005=ORIENTED_EDGE('',*,*,#8722,.T.);
#11006=ORIENTED_EDGE('',*,*,#8719,.T.);
#11007=ORIENTED_EDGE('',*,*,#8716,.T.);
#11008=ORIENTED_EDGE('',*,*,#8713,.T.);
#11009=ORIENTED_EDGE('',*,*,#8707,.T.);
#11010=ORIENTED_EDGE('',*,*,#8704,.T.);
#11011=ORIENTED_EDGE('',*,*,#8701,.T.);
#11012=ORIENTED_EDGE('',*,*,#8698,.T.);
#11013=ORIENTED_EDGE('',*,*,#8692,.T.);
#11014=ORIENTED_EDGE('',*,*,#8776,.T.);
#11015=ORIENTED_EDGE('',*,*,#8775,.T.);
#11016=ORIENTED_EDGE('',*,*,#8777,.F.);
#11017=ORIENTED_EDGE('',*,*,#8778,.F.);
#11018=ORIENTED_EDGE('',*,*,#8766,.F.);
#11019=ORIENTED_EDGE('',*,*,#8771,.F.);
#11020=ORIENTED_EDGE('',*,*,#8767,.T.);
#11021=ORIENTED_EDGE('',*,*,#8778,.T.);
#11022=ORIENTED_EDGE('',*,*,#8779,.F.);
#11023=ORIENTED_EDGE('',*,*,#8780,.F.);
#11024=ORIENTED_EDGE('',*,*,#8693,.T.);
#11025=ORIENTED_EDGE('',*,*,#8708,.T.);
#11026=ORIENTED_EDGE('',*,*,#8723,.T.);
#11027=ORIENTED_EDGE('',*,*,#8741,.T.);
#11028=ORIENTED_EDGE('',*,*,#8744,.T.);
#11029=ORIENTED_EDGE('',*,*,#8747,.T.);
#11030=ORIENTED_EDGE('',*,*,#8750,.T.);
#11031=ORIENTED_EDGE('',*,*,#8753,.T.);
#11032=ORIENTED_EDGE('',*,*,#8738,.T.);
#11033=ORIENTED_EDGE('',*,*,#8735,.T.);
#11034=ORIENTED_EDGE('',*,*,#8732,.T.);
#11035=ORIENTED_EDGE('',*,*,#8729,.T.);
#11036=ORIENTED_EDGE('',*,*,#8726,.T.);
#11037=ORIENTED_EDGE('',*,*,#8720,.T.);
#11038=ORIENTED_EDGE('',*,*,#8717,.T.);
#11039=ORIENTED_EDGE('',*,*,#8714,.T.);
#11040=ORIENTED_EDGE('',*,*,#8711,.T.);
#11041=ORIENTED_EDGE('',*,*,#8705,.T.);
#11042=ORIENTED_EDGE('',*,*,#8702,.T.);
#11043=ORIENTED_EDGE('',*,*,#8699,.T.);
#11044=ORIENTED_EDGE('',*,*,#8696,.T.);
#11045=ORIENTED_EDGE('',*,*,#8690,.T.);
#11046=ORIENTED_EDGE('',*,*,#8781,.T.);
#11047=ORIENTED_EDGE('',*,*,#8769,.F.);
#11048=ORIENTED_EDGE('',*,*,#8768,.T.);
#11049=ORIENTED_EDGE('',*,*,#8780,.T.);
#11050=ORIENTED_EDGE('',*,*,#8782,.F.);
#11051=ORIENTED_EDGE('',*,*,#8773,.F.);
#11052=ORIENTED_EDGE('',*,*,#8782,.T.);
#11053=ORIENTED_EDGE('',*,*,#8779,.T.);
#11054=ORIENTED_EDGE('',*,*,#8777,.T.);
#11055=ORIENTED_EDGE('',*,*,#8774,.T.);
#11056=ORIENTED_EDGE('',*,*,#8781,.F.);
#11057=ORIENTED_EDGE('',*,*,#8772,.F.);
#11058=ORIENTED_EDGE('',*,*,#8776,.F.);
#11059=ORIENTED_EDGE('',*,*,#8770,.F.);
#11060=ORIENTED_EDGE('',*,*,#8756,.T.);
#11061=ORIENTED_EDGE('',*,*,#8759,.T.);
#11062=ORIENTED_EDGE('',*,*,#8762,.T.);
#11063=ORIENTED_EDGE('',*,*,#8783,.F.);
#11064=ORIENTED_EDGE('',*,*,#8784,.T.);
#11065=ORIENTED_EDGE('',*,*,#8785,.F.);
#11066=ORIENTED_EDGE('',*,*,#8784,.F.);
#11067=ORIENTED_EDGE('',*,*,#8786,.F.);
#11068=ORIENTED_EDGE('',*,*,#8787,.T.);
#11069=ORIENTED_EDGE('',*,*,#8788,.F.);
#11070=ORIENTED_EDGE('',*,*,#8787,.F.);
#11071=ORIENTED_EDGE('',*,*,#8789,.F.);
#11072=ORIENTED_EDGE('',*,*,#8790,.T.);
#11073=ORIENTED_EDGE('',*,*,#8791,.F.);
#11074=ORIENTED_EDGE('',*,*,#8790,.F.);
#11075=ORIENTED_EDGE('',*,*,#8792,.F.);
#11076=ORIENTED_EDGE('',*,*,#8793,.T.);
#11077=ORIENTED_EDGE('',*,*,#8794,.F.);
#11078=ORIENTED_EDGE('',*,*,#8793,.F.);
#11079=ORIENTED_EDGE('',*,*,#8795,.F.);
#11080=ORIENTED_EDGE('',*,*,#8796,.T.);
#11081=ORIENTED_EDGE('',*,*,#8797,.F.);
#11082=ORIENTED_EDGE('',*,*,#8796,.F.);
#11083=ORIENTED_EDGE('',*,*,#8795,.T.);
#11084=ORIENTED_EDGE('',*,*,#8798,.T.);
#11085=ORIENTED_EDGE('',*,*,#8798,.F.);
#11086=ORIENTED_EDGE('',*,*,#8799,.T.);
#11087=ORIENTED_EDGE('',*,*,#8800,.T.);
#11088=ORIENTED_EDGE('',*,*,#8799,.F.);
#11089=ORIENTED_EDGE('',*,*,#8801,.F.);
#11090=ORIENTED_EDGE('',*,*,#8802,.T.);
#11091=ORIENTED_EDGE('',*,*,#8803,.T.);
#11092=ORIENTED_EDGE('',*,*,#8802,.F.);
#11093=ORIENTED_EDGE('',*,*,#8801,.T.);
#11094=ORIENTED_EDGE('',*,*,#8797,.T.);
#11095=ORIENTED_EDGE('',*,*,#8794,.T.);
#11096=ORIENTED_EDGE('',*,*,#8791,.T.);
#11097=ORIENTED_EDGE('',*,*,#8788,.T.);
#11098=ORIENTED_EDGE('',*,*,#8785,.T.);
#11099=ORIENTED_EDGE('',*,*,#8803,.F.);
#11100=ORIENTED_EDGE('',*,*,#8800,.F.);
#11101=ORIENTED_EDGE('',*,*,#8792,.T.);
#11102=ORIENTED_EDGE('',*,*,#8789,.T.);
#11103=ORIENTED_EDGE('',*,*,#8786,.T.);
#11104=ORIENTED_EDGE('',*,*,#8783,.T.);
#11105=ORIENTED_EDGE('',*,*,#8804,.F.);
#11106=ORIENTED_EDGE('',*,*,#8805,.T.);
#11107=ORIENTED_EDGE('',*,*,#8806,.F.);
#11108=ORIENTED_EDGE('',*,*,#8805,.F.);
#11109=ORIENTED_EDGE('',*,*,#8807,.F.);
#11110=ORIENTED_EDGE('',*,*,#8808,.T.);
#11111=ORIENTED_EDGE('',*,*,#8809,.F.);
#11112=ORIENTED_EDGE('',*,*,#8808,.F.);
#11113=ORIENTED_EDGE('',*,*,#8810,.F.);
#11114=ORIENTED_EDGE('',*,*,#8811,.T.);
#11115=ORIENTED_EDGE('',*,*,#8812,.F.);
#11116=ORIENTED_EDGE('',*,*,#8811,.F.);
#11117=ORIENTED_EDGE('',*,*,#8813,.F.);
#11118=ORIENTED_EDGE('',*,*,#8814,.T.);
#11119=ORIENTED_EDGE('',*,*,#8815,.F.);
#11120=ORIENTED_EDGE('',*,*,#8814,.F.);
#11121=ORIENTED_EDGE('',*,*,#8816,.F.);
#11122=ORIENTED_EDGE('',*,*,#8817,.T.);
#11123=ORIENTED_EDGE('',*,*,#8818,.T.);
#11124=ORIENTED_EDGE('',*,*,#8817,.F.);
#11125=ORIENTED_EDGE('',*,*,#8818,.F.);
#11126=ORIENTED_EDGE('',*,*,#8819,.F.);
#11127=ORIENTED_EDGE('',*,*,#8820,.F.);
#11128=ORIENTED_EDGE('',*,*,#8821,.T.);
#11129=ORIENTED_EDGE('',*,*,#8819,.T.);
#11130=ORIENTED_EDGE('',*,*,#8821,.F.);
#11131=ORIENTED_EDGE('',*,*,#8822,.F.);
#11132=ORIENTED_EDGE('',*,*,#8823,.T.);
#11133=ORIENTED_EDGE('',*,*,#8824,.T.);
#11134=ORIENTED_EDGE('',*,*,#8823,.F.);
#11135=ORIENTED_EDGE('',*,*,#8822,.T.);
#11136=ORIENTED_EDGE('',*,*,#8820,.T.);
#11137=ORIENTED_EDGE('',*,*,#8815,.T.);
#11138=ORIENTED_EDGE('',*,*,#8812,.T.);
#11139=ORIENTED_EDGE('',*,*,#8809,.T.);
#11140=ORIENTED_EDGE('',*,*,#8806,.T.);
#11141=ORIENTED_EDGE('',*,*,#8824,.F.);
#11142=ORIENTED_EDGE('',*,*,#8816,.T.);
#11143=ORIENTED_EDGE('',*,*,#8813,.T.);
#11144=ORIENTED_EDGE('',*,*,#8810,.T.);
#11145=ORIENTED_EDGE('',*,*,#8807,.T.);
#11146=ORIENTED_EDGE('',*,*,#8804,.T.);
#11147=ORIENTED_EDGE('',*,*,#8825,.F.);
#11148=ORIENTED_EDGE('',*,*,#8826,.T.);
#11149=ORIENTED_EDGE('',*,*,#8827,.F.);
#11150=ORIENTED_EDGE('',*,*,#8826,.F.);
#11151=ORIENTED_EDGE('',*,*,#8828,.F.);
#11152=ORIENTED_EDGE('',*,*,#8829,.T.);
#11153=ORIENTED_EDGE('',*,*,#8830,.F.);
#11154=ORIENTED_EDGE('',*,*,#8829,.F.);
#11155=ORIENTED_EDGE('',*,*,#8831,.F.);
#11156=ORIENTED_EDGE('',*,*,#8832,.T.);
#11157=ORIENTED_EDGE('',*,*,#8833,.F.);
#11158=ORIENTED_EDGE('',*,*,#8832,.F.);
#11159=ORIENTED_EDGE('',*,*,#8834,.F.);
#11160=ORIENTED_EDGE('',*,*,#8835,.T.);
#11161=ORIENTED_EDGE('',*,*,#8836,.F.);
#11162=ORIENTED_EDGE('',*,*,#8835,.F.);
#11163=ORIENTED_EDGE('',*,*,#8837,.F.);
#11164=ORIENTED_EDGE('',*,*,#8838,.T.);
#11165=ORIENTED_EDGE('',*,*,#8839,.F.);
#11166=ORIENTED_EDGE('',*,*,#8838,.F.);
#11167=ORIENTED_EDGE('',*,*,#8837,.T.);
#11168=ORIENTED_EDGE('',*,*,#8840,.T.);
#11169=ORIENTED_EDGE('',*,*,#8840,.F.);
#11170=ORIENTED_EDGE('',*,*,#8841,.T.);
#11171=ORIENTED_EDGE('',*,*,#8842,.T.);
#11172=ORIENTED_EDGE('',*,*,#8841,.F.);
#11173=ORIENTED_EDGE('',*,*,#8843,.F.);
#11174=ORIENTED_EDGE('',*,*,#8844,.T.);
#11175=ORIENTED_EDGE('',*,*,#8845,.T.);
#11176=ORIENTED_EDGE('',*,*,#8844,.F.);
#11177=ORIENTED_EDGE('',*,*,#8843,.T.);
#11178=ORIENTED_EDGE('',*,*,#8839,.T.);
#11179=ORIENTED_EDGE('',*,*,#8836,.T.);
#11180=ORIENTED_EDGE('',*,*,#8833,.T.);
#11181=ORIENTED_EDGE('',*,*,#8830,.T.);
#11182=ORIENTED_EDGE('',*,*,#8827,.T.);
#11183=ORIENTED_EDGE('',*,*,#8845,.F.);
#11184=ORIENTED_EDGE('',*,*,#8842,.F.);
#11185=ORIENTED_EDGE('',*,*,#8834,.T.);
#11186=ORIENTED_EDGE('',*,*,#8831,.T.);
#11187=ORIENTED_EDGE('',*,*,#8828,.T.);
#11188=ORIENTED_EDGE('',*,*,#8825,.T.);
#11189=ORIENTED_EDGE('',*,*,#8846,.F.);
#11190=ORIENTED_EDGE('',*,*,#8847,.T.);
#11191=ORIENTED_EDGE('',*,*,#8848,.F.);
#11192=ORIENTED_EDGE('',*,*,#8847,.F.);
#11193=ORIENTED_EDGE('',*,*,#8849,.F.);
#11194=ORIENTED_EDGE('',*,*,#8850,.T.);
#11195=ORIENTED_EDGE('',*,*,#8851,.F.);
#11196=ORIENTED_EDGE('',*,*,#8850,.F.);
#11197=ORIENTED_EDGE('',*,*,#8852,.F.);
#11198=ORIENTED_EDGE('',*,*,#8853,.T.);
#11199=ORIENTED_EDGE('',*,*,#8854,.F.);
#11200=ORIENTED_EDGE('',*,*,#8853,.F.);
#11201=ORIENTED_EDGE('',*,*,#8855,.F.);
#11202=ORIENTED_EDGE('',*,*,#8856,.T.);
#11203=ORIENTED_EDGE('',*,*,#8857,.F.);
#11204=ORIENTED_EDGE('',*,*,#8856,.F.);
#11205=ORIENTED_EDGE('',*,*,#8858,.F.);
#11206=ORIENTED_EDGE('',*,*,#8859,.T.);
#11207=ORIENTED_EDGE('',*,*,#8860,.T.);
#11208=ORIENTED_EDGE('',*,*,#8859,.F.);
#11209=ORIENTED_EDGE('',*,*,#8860,.F.);
#11210=ORIENTED_EDGE('',*,*,#8861,.F.);
#11211=ORIENTED_EDGE('',*,*,#8862,.F.);
#11212=ORIENTED_EDGE('',*,*,#8863,.T.);
#11213=ORIENTED_EDGE('',*,*,#8861,.T.);
#11214=ORIENTED_EDGE('',*,*,#8863,.F.);
#11215=ORIENTED_EDGE('',*,*,#8864,.F.);
#11216=ORIENTED_EDGE('',*,*,#8865,.T.);
#11217=ORIENTED_EDGE('',*,*,#8866,.T.);
#11218=ORIENTED_EDGE('',*,*,#8865,.F.);
#11219=ORIENTED_EDGE('',*,*,#8864,.T.);
#11220=ORIENTED_EDGE('',*,*,#8862,.T.);
#11221=ORIENTED_EDGE('',*,*,#8857,.T.);
#11222=ORIENTED_EDGE('',*,*,#8854,.T.);
#11223=ORIENTED_EDGE('',*,*,#8851,.T.);
#11224=ORIENTED_EDGE('',*,*,#8848,.T.);
#11225=ORIENTED_EDGE('',*,*,#8866,.F.);
#11226=ORIENTED_EDGE('',*,*,#8858,.T.);
#11227=ORIENTED_EDGE('',*,*,#8855,.T.);
#11228=ORIENTED_EDGE('',*,*,#8852,.T.);
#11229=ORIENTED_EDGE('',*,*,#8849,.T.);
#11230=ORIENTED_EDGE('',*,*,#8846,.T.);
#11231=ORIENTED_EDGE('',*,*,#8867,.T.);
#11232=ORIENTED_EDGE('',*,*,#8868,.T.);
#11233=ORIENTED_EDGE('',*,*,#8869,.T.);
#11234=ORIENTED_EDGE('',*,*,#8870,.F.);
#11235=ORIENTED_EDGE('',*,*,#8871,.T.);
#11236=ORIENTED_EDGE('',*,*,#8872,.T.);
#11237=ORIENTED_EDGE('',*,*,#8873,.T.);
#11238=ORIENTED_EDGE('',*,*,#8868,.F.);
#11239=ORIENTED_EDGE('',*,*,#8874,.T.);
#11240=ORIENTED_EDGE('',*,*,#8875,.T.);
#11241=ORIENTED_EDGE('',*,*,#8876,.T.);
#11242=ORIENTED_EDGE('',*,*,#8872,.F.);
#11243=ORIENTED_EDGE('',*,*,#8877,.T.);
#11244=ORIENTED_EDGE('',*,*,#8878,.T.);
#11245=ORIENTED_EDGE('',*,*,#8879,.T.);
#11246=ORIENTED_EDGE('',*,*,#8875,.F.);
#11247=ORIENTED_EDGE('',*,*,#8880,.T.);
#11248=ORIENTED_EDGE('',*,*,#8881,.T.);
#11249=ORIENTED_EDGE('',*,*,#8882,.T.);
#11250=ORIENTED_EDGE('',*,*,#8878,.F.);
#11251=ORIENTED_EDGE('',*,*,#8883,.T.);
#11252=ORIENTED_EDGE('',*,*,#8870,.T.);
#11253=ORIENTED_EDGE('',*,*,#8884,.T.);
#11254=ORIENTED_EDGE('',*,*,#8881,.F.);
#11255=ORIENTED_EDGE('',*,*,#8883,.F.);
#11256=ORIENTED_EDGE('',*,*,#8880,.F.);
#11257=ORIENTED_EDGE('',*,*,#8877,.F.);
#11258=ORIENTED_EDGE('',*,*,#8874,.F.);
#11259=ORIENTED_EDGE('',*,*,#8871,.F.);
#11260=ORIENTED_EDGE('',*,*,#8867,.F.);
#11261=ORIENTED_EDGE('',*,*,#8884,.F.);
#11262=ORIENTED_EDGE('',*,*,#8869,.F.);
#11263=ORIENTED_EDGE('',*,*,#8873,.F.);
#11264=ORIENTED_EDGE('',*,*,#8876,.F.);
#11265=ORIENTED_EDGE('',*,*,#8879,.F.);
#11266=ORIENTED_EDGE('',*,*,#8882,.F.);
#11267=ORIENTED_EDGE('',*,*,#8885,.F.);
#11268=ORIENTED_EDGE('',*,*,#8886,.F.);
#11269=ORIENTED_EDGE('',*,*,#8887,.F.);
#11270=ORIENTED_EDGE('',*,*,#8888,.T.);
#11271=ORIENTED_EDGE('',*,*,#8886,.T.);
#11272=ORIENTED_EDGE('',*,*,#8888,.F.);
#11273=ORIENTED_EDGE('',*,*,#8889,.F.);
#11274=ORIENTED_EDGE('',*,*,#8890,.T.);
#11275=ORIENTED_EDGE('',*,*,#8887,.T.);
#11276=ORIENTED_EDGE('',*,*,#8890,.F.);
#11277=ORIENTED_EDGE('',*,*,#8891,.F.);
#11278=ORIENTED_EDGE('',*,*,#8892,.T.);
#11279=ORIENTED_EDGE('',*,*,#8889,.T.);
#11280=ORIENTED_EDGE('',*,*,#8892,.F.);
#11281=ORIENTED_EDGE('',*,*,#8891,.T.);
#11282=ORIENTED_EDGE('',*,*,#8893,.F.);
#11283=ORIENTED_EDGE('',*,*,#8894,.F.);
#11284=ORIENTED_EDGE('',*,*,#8895,.T.);
#11285=ORIENTED_EDGE('',*,*,#8893,.T.);
#11286=ORIENTED_EDGE('',*,*,#8895,.F.);
#11287=ORIENTED_EDGE('',*,*,#8885,.T.);
#11288=ORIENTED_EDGE('',*,*,#8896,.T.);
#11289=ORIENTED_EDGE('',*,*,#8894,.T.);
#11290=ORIENTED_EDGE('',*,*,#8896,.F.);
#11291=ORIENTED_EDGE('',*,*,#8897,.F.);
#11292=ORIENTED_EDGE('',*,*,#8898,.T.);
#11293=ORIENTED_EDGE('',*,*,#8899,.F.);
#11294=ORIENTED_EDGE('',*,*,#8898,.F.);
#11295=ORIENTED_EDGE('',*,*,#8900,.F.);
#11296=ORIENTED_EDGE('',*,*,#8901,.T.);
#11297=ORIENTED_EDGE('',*,*,#8902,.F.);
#11298=ORIENTED_EDGE('',*,*,#8901,.F.);
#11299=ORIENTED_EDGE('',*,*,#8903,.F.);
#11300=ORIENTED_EDGE('',*,*,#8904,.T.);
#11301=ORIENTED_EDGE('',*,*,#8905,.F.);
#11302=ORIENTED_EDGE('',*,*,#8904,.F.);
#11303=ORIENTED_EDGE('',*,*,#8906,.F.);
#11304=ORIENTED_EDGE('',*,*,#8907,.T.);
#11305=ORIENTED_EDGE('',*,*,#8908,.F.);
#11306=ORIENTED_EDGE('',*,*,#8907,.F.);
#11307=ORIENTED_EDGE('',*,*,#8909,.F.);
#11308=ORIENTED_EDGE('',*,*,#8910,.T.);
#11309=ORIENTED_EDGE('',*,*,#8911,.F.);
#11310=ORIENTED_EDGE('',*,*,#8910,.F.);
#11311=ORIENTED_EDGE('',*,*,#8909,.T.);
#11312=ORIENTED_EDGE('',*,*,#8912,.T.);
#11313=ORIENTED_EDGE('',*,*,#8912,.F.);
#11314=ORIENTED_EDGE('',*,*,#8913,.T.);
#11315=ORIENTED_EDGE('',*,*,#8914,.T.);
#11316=ORIENTED_EDGE('',*,*,#8913,.F.);
#11317=ORIENTED_EDGE('',*,*,#8915,.F.);
#11318=ORIENTED_EDGE('',*,*,#8916,.T.);
#11319=ORIENTED_EDGE('',*,*,#8917,.T.);
#11320=ORIENTED_EDGE('',*,*,#8916,.F.);
#11321=ORIENTED_EDGE('',*,*,#8915,.T.);
#11322=ORIENTED_EDGE('',*,*,#8911,.T.);
#11323=ORIENTED_EDGE('',*,*,#8908,.T.);
#11324=ORIENTED_EDGE('',*,*,#8905,.T.);
#11325=ORIENTED_EDGE('',*,*,#8902,.T.);
#11326=ORIENTED_EDGE('',*,*,#8899,.T.);
#11327=ORIENTED_EDGE('',*,*,#8917,.F.);
#11328=ORIENTED_EDGE('',*,*,#8914,.F.);
#11329=ORIENTED_EDGE('',*,*,#8906,.T.);
#11330=ORIENTED_EDGE('',*,*,#8903,.T.);
#11331=ORIENTED_EDGE('',*,*,#8900,.T.);
#11332=ORIENTED_EDGE('',*,*,#8897,.T.);
#11333=ORIENTED_EDGE('',*,*,#8918,.F.);
#11334=ORIENTED_EDGE('',*,*,#8919,.T.);
#11335=ORIENTED_EDGE('',*,*,#8920,.F.);
#11336=ORIENTED_EDGE('',*,*,#8919,.F.);
#11337=ORIENTED_EDGE('',*,*,#8921,.F.);
#11338=ORIENTED_EDGE('',*,*,#8922,.T.);
#11339=ORIENTED_EDGE('',*,*,#8923,.F.);
#11340=ORIENTED_EDGE('',*,*,#8922,.F.);
#11341=ORIENTED_EDGE('',*,*,#8924,.F.);
#11342=ORIENTED_EDGE('',*,*,#8925,.T.);
#11343=ORIENTED_EDGE('',*,*,#8926,.F.);
#11344=ORIENTED_EDGE('',*,*,#8925,.F.);
#11345=ORIENTED_EDGE('',*,*,#8927,.F.);
#11346=ORIENTED_EDGE('',*,*,#8928,.T.);
#11347=ORIENTED_EDGE('',*,*,#8929,.F.);
#11348=ORIENTED_EDGE('',*,*,#8928,.F.);
#11349=ORIENTED_EDGE('',*,*,#8930,.F.);
#11350=ORIENTED_EDGE('',*,*,#8931,.T.);
#11351=ORIENTED_EDGE('',*,*,#8932,.T.);
#11352=ORIENTED_EDGE('',*,*,#8931,.F.);
#11353=ORIENTED_EDGE('',*,*,#8932,.F.);
#11354=ORIENTED_EDGE('',*,*,#8933,.F.);
#11355=ORIENTED_EDGE('',*,*,#8934,.F.);
#11356=ORIENTED_EDGE('',*,*,#8935,.T.);
#11357=ORIENTED_EDGE('',*,*,#8933,.T.);
#11358=ORIENTED_EDGE('',*,*,#8935,.F.);
#11359=ORIENTED_EDGE('',*,*,#8936,.F.);
#11360=ORIENTED_EDGE('',*,*,#8937,.T.);
#11361=ORIENTED_EDGE('',*,*,#8938,.T.);
#11362=ORIENTED_EDGE('',*,*,#8937,.F.);
#11363=ORIENTED_EDGE('',*,*,#8936,.T.);
#11364=ORIENTED_EDGE('',*,*,#8934,.T.);
#11365=ORIENTED_EDGE('',*,*,#8929,.T.);
#11366=ORIENTED_EDGE('',*,*,#8926,.T.);
#11367=ORIENTED_EDGE('',*,*,#8923,.T.);
#11368=ORIENTED_EDGE('',*,*,#8920,.T.);
#11369=ORIENTED_EDGE('',*,*,#8938,.F.);
#11370=ORIENTED_EDGE('',*,*,#8930,.T.);
#11371=ORIENTED_EDGE('',*,*,#8927,.T.);
#11372=ORIENTED_EDGE('',*,*,#8924,.T.);
#11373=ORIENTED_EDGE('',*,*,#8921,.T.);
#11374=ORIENTED_EDGE('',*,*,#8918,.T.);
#11375=ORIENTED_EDGE('',*,*,#8939,.F.);
#11376=ORIENTED_EDGE('',*,*,#8940,.T.);
#11377=ORIENTED_EDGE('',*,*,#8941,.F.);
#11378=ORIENTED_EDGE('',*,*,#8940,.F.);
#11379=ORIENTED_EDGE('',*,*,#8942,.F.);
#11380=ORIENTED_EDGE('',*,*,#8943,.T.);
#11381=ORIENTED_EDGE('',*,*,#8944,.F.);
#11382=ORIENTED_EDGE('',*,*,#8943,.F.);
#11383=ORIENTED_EDGE('',*,*,#8945,.F.);
#11384=ORIENTED_EDGE('',*,*,#8946,.T.);
#11385=ORIENTED_EDGE('',*,*,#8947,.F.);
#11386=ORIENTED_EDGE('',*,*,#8946,.F.);
#11387=ORIENTED_EDGE('',*,*,#8948,.F.);
#11388=ORIENTED_EDGE('',*,*,#8949,.T.);
#11389=ORIENTED_EDGE('',*,*,#8950,.F.);
#11390=ORIENTED_EDGE('',*,*,#8949,.F.);
#11391=ORIENTED_EDGE('',*,*,#8951,.F.);
#11392=ORIENTED_EDGE('',*,*,#8952,.T.);
#11393=ORIENTED_EDGE('',*,*,#8953,.F.);
#11394=ORIENTED_EDGE('',*,*,#8952,.F.);
#11395=ORIENTED_EDGE('',*,*,#8951,.T.);
#11396=ORIENTED_EDGE('',*,*,#8954,.T.);
#11397=ORIENTED_EDGE('',*,*,#8954,.F.);
#11398=ORIENTED_EDGE('',*,*,#8955,.T.);
#11399=ORIENTED_EDGE('',*,*,#8956,.T.);
#11400=ORIENTED_EDGE('',*,*,#8955,.F.);
#11401=ORIENTED_EDGE('',*,*,#8957,.F.);
#11402=ORIENTED_EDGE('',*,*,#8958,.T.);
#11403=ORIENTED_EDGE('',*,*,#8959,.T.);
#11404=ORIENTED_EDGE('',*,*,#8958,.F.);
#11405=ORIENTED_EDGE('',*,*,#8957,.T.);
#11406=ORIENTED_EDGE('',*,*,#8953,.T.);
#11407=ORIENTED_EDGE('',*,*,#8950,.T.);
#11408=ORIENTED_EDGE('',*,*,#8947,.T.);
#11409=ORIENTED_EDGE('',*,*,#8944,.T.);
#11410=ORIENTED_EDGE('',*,*,#8941,.T.);
#11411=ORIENTED_EDGE('',*,*,#8959,.F.);
#11412=ORIENTED_EDGE('',*,*,#8956,.F.);
#11413=ORIENTED_EDGE('',*,*,#8948,.T.);
#11414=ORIENTED_EDGE('',*,*,#8945,.T.);
#11415=ORIENTED_EDGE('',*,*,#8942,.T.);
#11416=ORIENTED_EDGE('',*,*,#8939,.T.);
#11417=ORIENTED_EDGE('',*,*,#8960,.F.);
#11418=ORIENTED_EDGE('',*,*,#8961,.T.);
#11419=ORIENTED_EDGE('',*,*,#8962,.F.);
#11420=ORIENTED_EDGE('',*,*,#8961,.F.);
#11421=ORIENTED_EDGE('',*,*,#8963,.F.);
#11422=ORIENTED_EDGE('',*,*,#8964,.T.);
#11423=ORIENTED_EDGE('',*,*,#8965,.F.);
#11424=ORIENTED_EDGE('',*,*,#8964,.F.);
#11425=ORIENTED_EDGE('',*,*,#8966,.F.);
#11426=ORIENTED_EDGE('',*,*,#8967,.T.);
#11427=ORIENTED_EDGE('',*,*,#8968,.F.);
#11428=ORIENTED_EDGE('',*,*,#8967,.F.);
#11429=ORIENTED_EDGE('',*,*,#8969,.F.);
#11430=ORIENTED_EDGE('',*,*,#8970,.T.);
#11431=ORIENTED_EDGE('',*,*,#8971,.F.);
#11432=ORIENTED_EDGE('',*,*,#8970,.F.);
#11433=ORIENTED_EDGE('',*,*,#8972,.F.);
#11434=ORIENTED_EDGE('',*,*,#8973,.T.);
#11435=ORIENTED_EDGE('',*,*,#8974,.T.);
#11436=ORIENTED_EDGE('',*,*,#8973,.F.);
#11437=ORIENTED_EDGE('',*,*,#8974,.F.);
#11438=ORIENTED_EDGE('',*,*,#8975,.F.);
#11439=ORIENTED_EDGE('',*,*,#8976,.F.);
#11440=ORIENTED_EDGE('',*,*,#8977,.T.);
#11441=ORIENTED_EDGE('',*,*,#8975,.T.);
#11442=ORIENTED_EDGE('',*,*,#8977,.F.);
#11443=ORIENTED_EDGE('',*,*,#8978,.F.);
#11444=ORIENTED_EDGE('',*,*,#8979,.T.);
#11445=ORIENTED_EDGE('',*,*,#8980,.T.);
#11446=ORIENTED_EDGE('',*,*,#8979,.F.);
#11447=ORIENTED_EDGE('',*,*,#8978,.T.);
#11448=ORIENTED_EDGE('',*,*,#8976,.T.);
#11449=ORIENTED_EDGE('',*,*,#8971,.T.);
#11450=ORIENTED_EDGE('',*,*,#8968,.T.);
#11451=ORIENTED_EDGE('',*,*,#8965,.T.);
#11452=ORIENTED_EDGE('',*,*,#8962,.T.);
#11453=ORIENTED_EDGE('',*,*,#8980,.F.);
#11454=ORIENTED_EDGE('',*,*,#8972,.T.);
#11455=ORIENTED_EDGE('',*,*,#8969,.T.);
#11456=ORIENTED_EDGE('',*,*,#8966,.T.);
#11457=ORIENTED_EDGE('',*,*,#8963,.T.);
#11458=ORIENTED_EDGE('',*,*,#8960,.T.);
#11459=ORIENTED_EDGE('',*,*,#8981,.F.);
#11460=ORIENTED_EDGE('',*,*,#8982,.F.);
#11461=ORIENTED_EDGE('',*,*,#8983,.T.);
#11462=ORIENTED_EDGE('',*,*,#8984,.F.);
#11463=ORIENTED_EDGE('',*,*,#8985,.F.);
#11464=ORIENTED_EDGE('',*,*,#8983,.F.);
#11465=ORIENTED_EDGE('',*,*,#8984,.T.);
#11466=ORIENTED_EDGE('',*,*,#8985,.T.);
#11467=ORIENTED_EDGE('',*,*,#8986,.T.);
#11468=ORIENTED_EDGE('',*,*,#8987,.T.);
#11469=ORIENTED_EDGE('',*,*,#8986,.F.);
#11470=ORIENTED_EDGE('',*,*,#8988,.T.);
#11471=ORIENTED_EDGE('',*,*,#8989,.T.);
#11472=ORIENTED_EDGE('',*,*,#8990,.F.);
#11473=ORIENTED_EDGE('',*,*,#8989,.F.);
#11474=ORIENTED_EDGE('',*,*,#8990,.T.);
#11475=ORIENTED_EDGE('',*,*,#8991,.T.);
#11476=ORIENTED_EDGE('',*,*,#8992,.F.);
#11477=ORIENTED_EDGE('',*,*,#8991,.F.);
#11478=ORIENTED_EDGE('',*,*,#8987,.F.);
#11479=ORIENTED_EDGE('',*,*,#8992,.T.);
#11480=ORIENTED_EDGE('',*,*,#8993,.F.);
#11481=ORIENTED_EDGE('',*,*,#8994,.T.);
#11482=ORIENTED_EDGE('',*,*,#8981,.T.);
#11483=ORIENTED_EDGE('',*,*,#8982,.T.);
#11484=ORIENTED_EDGE('',*,*,#8994,.F.);
#11485=ORIENTED_EDGE('',*,*,#8993,.T.);
#11486=ORIENTED_EDGE('',*,*,#8995,.F.);
#11487=ORIENTED_EDGE('',*,*,#8995,.T.);
#11488=ORIENTED_EDGE('',*,*,#8996,.T.);
#11489=ORIENTED_EDGE('',*,*,#8988,.F.);
#11490=ORIENTED_EDGE('',*,*,#8996,.F.);
#11491=ORIENTED_EDGE('',*,*,#8997,.F.);
#11492=ORIENTED_EDGE('',*,*,#8998,.F.);
#11493=ORIENTED_EDGE('',*,*,#8999,.T.);
#11494=ORIENTED_EDGE('',*,*,#9000,.F.);
#11495=ORIENTED_EDGE('',*,*,#9001,.F.);
#11496=ORIENTED_EDGE('',*,*,#8999,.F.);
#11497=ORIENTED_EDGE('',*,*,#9002,.T.);
#11498=ORIENTED_EDGE('',*,*,#9003,.T.);
#11499=ORIENTED_EDGE('',*,*,#9000,.T.);
#11500=ORIENTED_EDGE('',*,*,#9001,.T.);
#11501=ORIENTED_EDGE('',*,*,#9003,.F.);
#11502=ORIENTED_EDGE('',*,*,#9004,.F.);
#11503=ORIENTED_EDGE('',*,*,#9005,.T.);
#11504=ORIENTED_EDGE('',*,*,#9006,.F.);
#11505=ORIENTED_EDGE('',*,*,#9007,.T.);
#11506=ORIENTED_EDGE('',*,*,#9004,.T.);
#11507=ORIENTED_EDGE('',*,*,#9007,.F.);
#11508=ORIENTED_EDGE('',*,*,#9008,.F.);
#11509=ORIENTED_EDGE('',*,*,#9009,.T.);
#11510=ORIENTED_EDGE('',*,*,#9006,.T.);
#11511=ORIENTED_EDGE('',*,*,#9009,.F.);
#11512=ORIENTED_EDGE('',*,*,#9010,.F.);
#11513=ORIENTED_EDGE('',*,*,#9011,.T.);
#11514=ORIENTED_EDGE('',*,*,#9008,.T.);
#11515=ORIENTED_EDGE('',*,*,#9011,.F.);
#11516=ORIENTED_EDGE('',*,*,#9010,.T.);
#11517=ORIENTED_EDGE('',*,*,#9002,.F.);
#11518=ORIENTED_EDGE('',*,*,#8997,.T.);
#11519=ORIENTED_EDGE('',*,*,#8998,.T.);
#11520=ORIENTED_EDGE('',*,*,#9012,.T.);
#11521=ORIENTED_EDGE('',*,*,#9005,.F.);
#11522=ORIENTED_EDGE('',*,*,#9012,.F.);
#11523=ORIENTED_EDGE('',*,*,#9013,.T.);
#11524=ORIENTED_EDGE('',*,*,#9013,.F.);
#11525=ORIENTED_EDGE('',*,*,#9014,.T.);
#11526=ORIENTED_EDGE('',*,*,#9014,.F.);
#11527=ORIENTED_EDGE('',*,*,#9015,.T.);
#11528=ORIENTED_EDGE('',*,*,#9015,.F.);
#11529=ORIENTED_EDGE('',*,*,#9016,.T.);
#11530=ORIENTED_EDGE('',*,*,#9016,.F.);
#11531=ORIENTED_EDGE('',*,*,#9017,.T.);
#11532=ORIENTED_EDGE('',*,*,#9017,.F.);
#11533=ORIENTED_EDGE('',*,*,#9018,.T.);
#11534=ORIENTED_EDGE('',*,*,#9018,.F.);
#11535=ORIENTED_EDGE('',*,*,#9019,.T.);
#11536=ORIENTED_EDGE('',*,*,#9019,.F.);
#11537=ORIENTED_EDGE('',*,*,#9020,.F.);
#11538=ORIENTED_EDGE('',*,*,#9021,.F.);
#11539=ORIENTED_EDGE('',*,*,#9022,.F.);
#11540=ORIENTED_EDGE('',*,*,#9023,.F.);
#11541=ORIENTED_EDGE('',*,*,#9022,.T.);
#11542=ORIENTED_EDGE('',*,*,#9024,.F.);
#11543=ORIENTED_EDGE('',*,*,#9025,.T.);
#11544=ORIENTED_EDGE('',*,*,#9026,.F.);
#11545=ORIENTED_EDGE('',*,*,#9027,.T.);
#11546=ORIENTED_EDGE('',*,*,#9028,.F.);
#11547=ORIENTED_EDGE('',*,*,#9029,.T.);
#11548=ORIENTED_EDGE('',*,*,#9030,.F.);
#11549=ORIENTED_EDGE('',*,*,#9029,.F.);
#11550=ORIENTED_EDGE('',*,*,#9031,.F.);
#11551=ORIENTED_EDGE('',*,*,#9032,.T.);
#11552=ORIENTED_EDGE('',*,*,#9033,.F.);
#11553=ORIENTED_EDGE('',*,*,#9034,.T.);
#11554=ORIENTED_EDGE('',*,*,#9035,.F.);
#11555=ORIENTED_EDGE('',*,*,#9036,.T.);
#11556=ORIENTED_EDGE('',*,*,#9037,.F.);
#11557=ORIENTED_EDGE('',*,*,#9038,.T.);
#11558=ORIENTED_EDGE('',*,*,#9039,.F.);
#11559=ORIENTED_EDGE('',*,*,#9021,.T.);
#11560=ORIENTED_EDGE('',*,*,#9040,.T.);
#11561=ORIENTED_EDGE('',*,*,#9041,.T.);
#11562=ORIENTED_EDGE('',*,*,#9024,.T.);
#11563=ORIENTED_EDGE('',*,*,#9042,.F.);
#11564=ORIENTED_EDGE('',*,*,#9043,.F.);
#11565=ORIENTED_EDGE('',*,*,#9025,.F.);
#11566=ORIENTED_EDGE('',*,*,#9041,.F.);
#11567=ORIENTED_EDGE('',*,*,#9043,.T.);
#11568=ORIENTED_EDGE('',*,*,#9044,.T.);
#11569=ORIENTED_EDGE('',*,*,#9045,.T.);
#11570=ORIENTED_EDGE('',*,*,#9026,.T.);
#11571=ORIENTED_EDGE('',*,*,#9046,.F.);
#11572=ORIENTED_EDGE('',*,*,#9047,.F.);
#11573=ORIENTED_EDGE('',*,*,#9027,.F.);
#11574=ORIENTED_EDGE('',*,*,#9045,.F.);
#11575=ORIENTED_EDGE('',*,*,#9047,.T.);
#11576=ORIENTED_EDGE('',*,*,#9048,.T.);
#11577=ORIENTED_EDGE('',*,*,#9049,.T.);
#11578=ORIENTED_EDGE('',*,*,#9050,.T.);
#11579=ORIENTED_EDGE('',*,*,#9031,.T.);
#11580=ORIENTED_EDGE('',*,*,#9028,.T.);
#11581=ORIENTED_EDGE('',*,*,#9051,.F.);
#11582=ORIENTED_EDGE('',*,*,#9052,.F.);
#11583=ORIENTED_EDGE('',*,*,#9032,.F.);
#11584=ORIENTED_EDGE('',*,*,#9050,.F.);
#11585=ORIENTED_EDGE('',*,*,#9052,.T.);
#11586=ORIENTED_EDGE('',*,*,#9053,.T.);
#11587=ORIENTED_EDGE('',*,*,#9054,.T.);
#11588=ORIENTED_EDGE('',*,*,#9033,.T.);
#11589=ORIENTED_EDGE('',*,*,#9055,.F.);
#11590=ORIENTED_EDGE('',*,*,#9056,.F.);
#11591=ORIENTED_EDGE('',*,*,#9034,.F.);
#11592=ORIENTED_EDGE('',*,*,#9054,.F.);
#11593=ORIENTED_EDGE('',*,*,#9056,.T.);
#11594=ORIENTED_EDGE('',*,*,#9057,.T.);
#11595=ORIENTED_EDGE('',*,*,#9058,.T.);
#11596=ORIENTED_EDGE('',*,*,#9035,.T.);
#11597=ORIENTED_EDGE('',*,*,#9036,.F.);
#11598=ORIENTED_EDGE('',*,*,#9058,.F.);
#11599=ORIENTED_EDGE('',*,*,#9059,.F.);
#11600=ORIENTED_EDGE('',*,*,#9060,.F.);
#11601=ORIENTED_EDGE('',*,*,#9061,.F.);
#11602=ORIENTED_EDGE('',*,*,#9062,.T.);
#11603=ORIENTED_EDGE('',*,*,#9048,.F.);
#11604=ORIENTED_EDGE('',*,*,#9046,.T.);
#11605=ORIENTED_EDGE('',*,*,#9044,.F.);
#11606=ORIENTED_EDGE('',*,*,#9042,.T.);
#11607=ORIENTED_EDGE('',*,*,#9040,.F.);
#11608=ORIENTED_EDGE('',*,*,#9020,.T.);
#11609=ORIENTED_EDGE('',*,*,#9063,.F.);
#11610=ORIENTED_EDGE('',*,*,#9064,.T.);
#11611=ORIENTED_EDGE('',*,*,#9065,.F.);
#11612=ORIENTED_EDGE('',*,*,#9059,.T.);
#11613=ORIENTED_EDGE('',*,*,#9057,.F.);
#11614=ORIENTED_EDGE('',*,*,#9055,.T.);
#11615=ORIENTED_EDGE('',*,*,#9053,.F.);
#11616=ORIENTED_EDGE('',*,*,#9051,.T.);
#11617=ORIENTED_EDGE('',*,*,#9049,.F.);
#11618=ORIENTED_EDGE('',*,*,#9062,.F.);
#11619=ORIENTED_EDGE('',*,*,#9023,.T.);
#11620=ORIENTED_EDGE('',*,*,#9039,.T.);
#11621=ORIENTED_EDGE('',*,*,#9066,.T.);
#11622=ORIENTED_EDGE('',*,*,#9063,.T.);
#11623=ORIENTED_EDGE('',*,*,#9038,.F.);
#11624=ORIENTED_EDGE('',*,*,#9067,.F.);
#11625=ORIENTED_EDGE('',*,*,#9064,.F.);
#11626=ORIENTED_EDGE('',*,*,#9066,.F.);
#11627=ORIENTED_EDGE('',*,*,#9030,.T.);
#11628=ORIENTED_EDGE('',*,*,#9061,.T.);
#11629=ORIENTED_EDGE('',*,*,#9060,.T.);
#11630=ORIENTED_EDGE('',*,*,#9065,.T.);
#11631=ORIENTED_EDGE('',*,*,#9067,.T.);
#11632=ORIENTED_EDGE('',*,*,#9037,.T.);
#11633=ORIENTED_EDGE('',*,*,#9068,.F.);
#11634=ORIENTED_EDGE('',*,*,#9069,.T.);
#11635=ORIENTED_EDGE('',*,*,#9070,.F.);
#11636=ORIENTED_EDGE('',*,*,#9071,.T.);
#11637=ORIENTED_EDGE('',*,*,#9068,.T.);
#11638=ORIENTED_EDGE('',*,*,#9071,.F.);
#11639=ORIENTED_EDGE('',*,*,#9070,.T.);
#11640=ORIENTED_EDGE('',*,*,#9072,.F.);
#11641=ORIENTED_EDGE('',*,*,#9072,.T.);
#11642=ORIENTED_EDGE('',*,*,#9073,.T.);
#11643=ORIENTED_EDGE('',*,*,#9069,.F.);
#11644=ORIENTED_EDGE('',*,*,#9073,.F.);
#11645=ORIENTED_EDGE('',*,*,#9074,.F.);
#11646=ORIENTED_EDGE('',*,*,#9075,.T.);
#11647=ORIENTED_EDGE('',*,*,#9076,.F.);
#11648=ORIENTED_EDGE('',*,*,#9077,.T.);
#11649=ORIENTED_EDGE('',*,*,#9074,.T.);
#11650=ORIENTED_EDGE('',*,*,#9077,.F.);
#11651=ORIENTED_EDGE('',*,*,#9076,.T.);
#11652=ORIENTED_EDGE('',*,*,#9078,.F.);
#11653=ORIENTED_EDGE('',*,*,#9078,.T.);
#11654=ORIENTED_EDGE('',*,*,#9079,.T.);
#11655=ORIENTED_EDGE('',*,*,#9075,.F.);
#11656=ORIENTED_EDGE('',*,*,#9079,.F.);
#11657=ORIENTED_EDGE('',*,*,#9080,.F.);
#11658=ORIENTED_EDGE('',*,*,#9081,.F.);
#11659=ORIENTED_EDGE('',*,*,#9082,.T.);
#11660=ORIENTED_EDGE('',*,*,#9083,.F.);
#11661=ORIENTED_EDGE('',*,*,#9084,.F.);
#11662=ORIENTED_EDGE('',*,*,#9082,.F.);
#11663=ORIENTED_EDGE('',*,*,#9083,.T.);
#11664=ORIENTED_EDGE('',*,*,#9084,.T.);
#11665=ORIENTED_EDGE('',*,*,#9085,.T.);
#11666=ORIENTED_EDGE('',*,*,#9086,.T.);
#11667=ORIENTED_EDGE('',*,*,#9085,.F.);
#11668=ORIENTED_EDGE('',*,*,#9087,.T.);
#11669=ORIENTED_EDGE('',*,*,#9088,.T.);
#11670=ORIENTED_EDGE('',*,*,#9089,.F.);
#11671=ORIENTED_EDGE('',*,*,#9088,.F.);
#11672=ORIENTED_EDGE('',*,*,#9089,.T.);
#11673=ORIENTED_EDGE('',*,*,#9090,.T.);
#11674=ORIENTED_EDGE('',*,*,#9091,.F.);
#11675=ORIENTED_EDGE('',*,*,#9090,.F.);
#11676=ORIENTED_EDGE('',*,*,#9086,.F.);
#11677=ORIENTED_EDGE('',*,*,#9091,.T.);
#11678=ORIENTED_EDGE('',*,*,#9092,.F.);
#11679=ORIENTED_EDGE('',*,*,#9093,.T.);
#11680=ORIENTED_EDGE('',*,*,#9080,.T.);
#11681=ORIENTED_EDGE('',*,*,#9081,.T.);
#11682=ORIENTED_EDGE('',*,*,#9093,.F.);
#11683=ORIENTED_EDGE('',*,*,#9092,.T.);
#11684=ORIENTED_EDGE('',*,*,#9094,.F.);
#11685=ORIENTED_EDGE('',*,*,#9094,.T.);
#11686=ORIENTED_EDGE('',*,*,#9095,.T.);
#11687=ORIENTED_EDGE('',*,*,#9087,.F.);
#11688=ORIENTED_EDGE('',*,*,#9095,.F.);
#11689=ORIENTED_EDGE('',*,*,#9096,.F.);
#11690=ORIENTED_EDGE('',*,*,#9097,.F.);
#11691=ORIENTED_EDGE('',*,*,#9098,.T.);
#11692=ORIENTED_EDGE('',*,*,#9099,.F.);
#11693=ORIENTED_EDGE('',*,*,#9100,.F.);
#11694=ORIENTED_EDGE('',*,*,#9098,.F.);
#11695=ORIENTED_EDGE('',*,*,#9101,.T.);
#11696=ORIENTED_EDGE('',*,*,#9102,.T.);
#11697=ORIENTED_EDGE('',*,*,#9099,.T.);
#11698=ORIENTED_EDGE('',*,*,#9100,.T.);
#11699=ORIENTED_EDGE('',*,*,#9102,.F.);
#11700=ORIENTED_EDGE('',*,*,#9103,.F.);
#11701=ORIENTED_EDGE('',*,*,#9104,.T.);
#11702=ORIENTED_EDGE('',*,*,#9105,.F.);
#11703=ORIENTED_EDGE('',*,*,#9106,.T.);
#11704=ORIENTED_EDGE('',*,*,#9103,.T.);
#11705=ORIENTED_EDGE('',*,*,#9106,.F.);
#11706=ORIENTED_EDGE('',*,*,#9107,.F.);
#11707=ORIENTED_EDGE('',*,*,#9108,.T.);
#11708=ORIENTED_EDGE('',*,*,#9105,.T.);
#11709=ORIENTED_EDGE('',*,*,#9108,.F.);
#11710=ORIENTED_EDGE('',*,*,#9109,.F.);
#11711=ORIENTED_EDGE('',*,*,#9110,.T.);
#11712=ORIENTED_EDGE('',*,*,#9107,.T.);
#11713=ORIENTED_EDGE('',*,*,#9110,.F.);
#11714=ORIENTED_EDGE('',*,*,#9109,.T.);
#11715=ORIENTED_EDGE('',*,*,#9101,.F.);
#11716=ORIENTED_EDGE('',*,*,#9096,.T.);
#11717=ORIENTED_EDGE('',*,*,#9097,.T.);
#11718=ORIENTED_EDGE('',*,*,#9111,.T.);
#11719=ORIENTED_EDGE('',*,*,#9104,.F.);
#11720=ORIENTED_EDGE('',*,*,#9111,.F.);
#11721=ORIENTED_EDGE('',*,*,#9112,.T.);
#11722=ORIENTED_EDGE('',*,*,#9112,.F.);
#11723=ORIENTED_EDGE('',*,*,#9113,.T.);
#11724=ORIENTED_EDGE('',*,*,#9113,.F.);
#11725=ORIENTED_EDGE('',*,*,#9114,.T.);
#11726=ORIENTED_EDGE('',*,*,#9114,.F.);
#11727=ORIENTED_EDGE('',*,*,#9115,.T.);
#11728=ORIENTED_EDGE('',*,*,#9115,.F.);
#11729=ORIENTED_EDGE('',*,*,#9116,.T.);
#11730=ORIENTED_EDGE('',*,*,#9116,.F.);
#11731=ORIENTED_EDGE('',*,*,#9117,.T.);
#11732=ORIENTED_EDGE('',*,*,#9117,.F.);
#11733=ORIENTED_EDGE('',*,*,#9118,.T.);
#11734=ORIENTED_EDGE('',*,*,#9118,.F.);
#11735=ORIENTED_EDGE('',*,*,#9119,.T.);
#11736=ORIENTED_EDGE('',*,*,#9119,.F.);
#11737=ORIENTED_EDGE('',*,*,#9120,.F.);
#11738=ORIENTED_EDGE('',*,*,#9121,.F.);
#11739=ORIENTED_EDGE('',*,*,#9122,.F.);
#11740=ORIENTED_EDGE('',*,*,#9123,.F.);
#11741=ORIENTED_EDGE('',*,*,#9122,.T.);
#11742=ORIENTED_EDGE('',*,*,#9124,.F.);
#11743=ORIENTED_EDGE('',*,*,#9125,.T.);
#11744=ORIENTED_EDGE('',*,*,#9126,.F.);
#11745=ORIENTED_EDGE('',*,*,#9127,.T.);
#11746=ORIENTED_EDGE('',*,*,#9128,.F.);
#11747=ORIENTED_EDGE('',*,*,#9129,.T.);
#11748=ORIENTED_EDGE('',*,*,#9130,.T.);
#11749=ORIENTED_EDGE('',*,*,#9131,.F.);
#11750=ORIENTED_EDGE('',*,*,#9130,.F.);
#11751=ORIENTED_EDGE('',*,*,#9132,.T.);
#11752=ORIENTED_EDGE('',*,*,#9133,.F.);
#11753=ORIENTED_EDGE('',*,*,#9134,.T.);
#11754=ORIENTED_EDGE('',*,*,#9135,.F.);
#11755=ORIENTED_EDGE('',*,*,#9136,.T.);
#11756=ORIENTED_EDGE('',*,*,#9137,.F.);
#11757=ORIENTED_EDGE('',*,*,#9138,.T.);
#11758=ORIENTED_EDGE('',*,*,#9139,.F.);
#11759=ORIENTED_EDGE('',*,*,#9140,.T.);
#11760=ORIENTED_EDGE('',*,*,#9141,.F.);
#11761=ORIENTED_EDGE('',*,*,#9121,.T.);
#11762=ORIENTED_EDGE('',*,*,#9142,.T.);
#11763=ORIENTED_EDGE('',*,*,#9143,.T.);
#11764=ORIENTED_EDGE('',*,*,#9124,.T.);
#11765=ORIENTED_EDGE('',*,*,#9144,.F.);
#11766=ORIENTED_EDGE('',*,*,#9145,.F.);
#11767=ORIENTED_EDGE('',*,*,#9125,.F.);
#11768=ORIENTED_EDGE('',*,*,#9143,.F.);
#11769=ORIENTED_EDGE('',*,*,#9145,.T.);
#11770=ORIENTED_EDGE('',*,*,#9146,.T.);
#11771=ORIENTED_EDGE('',*,*,#9147,.T.);
#11772=ORIENTED_EDGE('',*,*,#9126,.T.);
#11773=ORIENTED_EDGE('',*,*,#9148,.F.);
#11774=ORIENTED_EDGE('',*,*,#9149,.F.);
#11775=ORIENTED_EDGE('',*,*,#9127,.F.);
#11776=ORIENTED_EDGE('',*,*,#9147,.F.);
#11777=ORIENTED_EDGE('',*,*,#9149,.T.);
#11778=ORIENTED_EDGE('',*,*,#9150,.T.);
#11779=ORIENTED_EDGE('',*,*,#9151,.T.);
#11780=ORIENTED_EDGE('',*,*,#9128,.T.);
#11781=ORIENTED_EDGE('',*,*,#9152,.F.);
#11782=ORIENTED_EDGE('',*,*,#9153,.F.);
#11783=ORIENTED_EDGE('',*,*,#9132,.F.);
#11784=ORIENTED_EDGE('',*,*,#9129,.F.);
#11785=ORIENTED_EDGE('',*,*,#9151,.F.);
#11786=ORIENTED_EDGE('',*,*,#9154,.F.);
#11787=ORIENTED_EDGE('',*,*,#9153,.T.);
#11788=ORIENTED_EDGE('',*,*,#9155,.T.);
#11789=ORIENTED_EDGE('',*,*,#9156,.T.);
#11790=ORIENTED_EDGE('',*,*,#9133,.T.);
#11791=ORIENTED_EDGE('',*,*,#9157,.F.);
#11792=ORIENTED_EDGE('',*,*,#9158,.F.);
#11793=ORIENTED_EDGE('',*,*,#9134,.F.);
#11794=ORIENTED_EDGE('',*,*,#9156,.F.);
#11795=ORIENTED_EDGE('',*,*,#9158,.T.);
#11796=ORIENTED_EDGE('',*,*,#9159,.T.);
#11797=ORIENTED_EDGE('',*,*,#9160,.T.);
#11798=ORIENTED_EDGE('',*,*,#9135,.T.);
#11799=ORIENTED_EDGE('',*,*,#9161,.F.);
#11800=ORIENTED_EDGE('',*,*,#9162,.F.);
#11801=ORIENTED_EDGE('',*,*,#9136,.F.);
#11802=ORIENTED_EDGE('',*,*,#9160,.F.);
#11803=ORIENTED_EDGE('',*,*,#9162,.T.);
#11804=ORIENTED_EDGE('',*,*,#9163,.T.);
#11805=ORIENTED_EDGE('',*,*,#9164,.T.);
#11806=ORIENTED_EDGE('',*,*,#9137,.T.);
#11807=ORIENTED_EDGE('',*,*,#9138,.F.);
#11808=ORIENTED_EDGE('',*,*,#9164,.F.);
#11809=ORIENTED_EDGE('',*,*,#9165,.F.);
#11810=ORIENTED_EDGE('',*,*,#9166,.F.);
#11811=ORIENTED_EDGE('',*,*,#9167,.F.);
#11812=ORIENTED_EDGE('',*,*,#9168,.T.);
#11813=ORIENTED_EDGE('',*,*,#9154,.T.);
#11814=ORIENTED_EDGE('',*,*,#9150,.F.);
#11815=ORIENTED_EDGE('',*,*,#9148,.T.);
#11816=ORIENTED_EDGE('',*,*,#9146,.F.);
#11817=ORIENTED_EDGE('',*,*,#9144,.T.);
#11818=ORIENTED_EDGE('',*,*,#9142,.F.);
#11819=ORIENTED_EDGE('',*,*,#9120,.T.);
#11820=ORIENTED_EDGE('',*,*,#9169,.F.);
#11821=ORIENTED_EDGE('',*,*,#9170,.T.);
#11822=ORIENTED_EDGE('',*,*,#9171,.F.);
#11823=ORIENTED_EDGE('',*,*,#9165,.T.);
#11824=ORIENTED_EDGE('',*,*,#9163,.F.);
#11825=ORIENTED_EDGE('',*,*,#9161,.T.);
#11826=ORIENTED_EDGE('',*,*,#9159,.F.);
#11827=ORIENTED_EDGE('',*,*,#9157,.T.);
#11828=ORIENTED_EDGE('',*,*,#9155,.F.);
#11829=ORIENTED_EDGE('',*,*,#9152,.T.);
#11830=ORIENTED_EDGE('',*,*,#9168,.F.);
#11831=ORIENTED_EDGE('',*,*,#9123,.T.);
#11832=ORIENTED_EDGE('',*,*,#9141,.T.);
#11833=ORIENTED_EDGE('',*,*,#9172,.T.);
#11834=ORIENTED_EDGE('',*,*,#9169,.T.);
#11835=ORIENTED_EDGE('',*,*,#9140,.F.);
#11836=ORIENTED_EDGE('',*,*,#9173,.F.);
#11837=ORIENTED_EDGE('',*,*,#9170,.F.);
#11838=ORIENTED_EDGE('',*,*,#9172,.F.);
#11839=ORIENTED_EDGE('',*,*,#9131,.T.);
#11840=ORIENTED_EDGE('',*,*,#9167,.T.);
#11841=ORIENTED_EDGE('',*,*,#9166,.T.);
#11842=ORIENTED_EDGE('',*,*,#9171,.T.);
#11843=ORIENTED_EDGE('',*,*,#9173,.T.);
#11844=ORIENTED_EDGE('',*,*,#9139,.T.);
#11845=ORIENTED_EDGE('',*,*,#9174,.F.);
#11846=ORIENTED_EDGE('',*,*,#9175,.T.);
#11847=ORIENTED_EDGE('',*,*,#9176,.F.);
#11848=ORIENTED_EDGE('',*,*,#9177,.T.);
#11849=ORIENTED_EDGE('',*,*,#9174,.T.);
#11850=ORIENTED_EDGE('',*,*,#9177,.F.);
#11851=ORIENTED_EDGE('',*,*,#9176,.T.);
#11852=ORIENTED_EDGE('',*,*,#9178,.F.);
#11853=ORIENTED_EDGE('',*,*,#9178,.T.);
#11854=ORIENTED_EDGE('',*,*,#9179,.T.);
#11855=ORIENTED_EDGE('',*,*,#9175,.F.);
#11856=ORIENTED_EDGE('',*,*,#9179,.F.);
#11857=ORIENTED_EDGE('',*,*,#9180,.F.);
#11858=ORIENTED_EDGE('',*,*,#9181,.T.);
#11859=ORIENTED_EDGE('',*,*,#9182,.F.);
#11860=ORIENTED_EDGE('',*,*,#9183,.T.);
#11861=ORIENTED_EDGE('',*,*,#9180,.T.);
#11862=ORIENTED_EDGE('',*,*,#9183,.F.);
#11863=ORIENTED_EDGE('',*,*,#9182,.T.);
#11864=ORIENTED_EDGE('',*,*,#9184,.F.);
#11865=ORIENTED_EDGE('',*,*,#9184,.T.);
#11866=ORIENTED_EDGE('',*,*,#9185,.T.);
#11867=ORIENTED_EDGE('',*,*,#9181,.F.);
#11868=ORIENTED_EDGE('',*,*,#9185,.F.);
#11869=ORIENTED_EDGE('',*,*,#9186,.T.);
#11870=ORIENTED_EDGE('',*,*,#9187,.T.);
#11871=ORIENTED_EDGE('',*,*,#9188,.T.);
#11872=ORIENTED_EDGE('',*,*,#9189,.F.);
#11873=ORIENTED_EDGE('',*,*,#9190,.T.);
#11874=ORIENTED_EDGE('',*,*,#9191,.T.);
#11875=ORIENTED_EDGE('',*,*,#9192,.T.);
#11876=ORIENTED_EDGE('',*,*,#9187,.F.);
#11877=ORIENTED_EDGE('',*,*,#9193,.T.);
#11878=ORIENTED_EDGE('',*,*,#9194,.T.);
#11879=ORIENTED_EDGE('',*,*,#9195,.T.);
#11880=ORIENTED_EDGE('',*,*,#9191,.F.);
#11881=ORIENTED_EDGE('',*,*,#9196,.T.);
#11882=ORIENTED_EDGE('',*,*,#9197,.T.);
#11883=ORIENTED_EDGE('',*,*,#9198,.T.);
#11884=ORIENTED_EDGE('',*,*,#9194,.F.);
#11885=ORIENTED_EDGE('',*,*,#9199,.T.);
#11886=ORIENTED_EDGE('',*,*,#9200,.T.);
#11887=ORIENTED_EDGE('',*,*,#9201,.T.);
#11888=ORIENTED_EDGE('',*,*,#9197,.F.);
#11889=ORIENTED_EDGE('',*,*,#9202,.T.);
#11890=ORIENTED_EDGE('',*,*,#9189,.T.);
#11891=ORIENTED_EDGE('',*,*,#9203,.T.);
#11892=ORIENTED_EDGE('',*,*,#9200,.F.);
#11893=ORIENTED_EDGE('',*,*,#9202,.F.);
#11894=ORIENTED_EDGE('',*,*,#9199,.F.);
#11895=ORIENTED_EDGE('',*,*,#9196,.F.);
#11896=ORIENTED_EDGE('',*,*,#9193,.F.);
#11897=ORIENTED_EDGE('',*,*,#9190,.F.);
#11898=ORIENTED_EDGE('',*,*,#9186,.F.);
#11899=ORIENTED_EDGE('',*,*,#9203,.F.);
#11900=ORIENTED_EDGE('',*,*,#9188,.F.);
#11901=ORIENTED_EDGE('',*,*,#9192,.F.);
#11902=ORIENTED_EDGE('',*,*,#9195,.F.);
#11903=ORIENTED_EDGE('',*,*,#9198,.F.);
#11904=ORIENTED_EDGE('',*,*,#9201,.F.);
#11905=ORIENTED_EDGE('',*,*,#9204,.F.);
#11906=ORIENTED_EDGE('',*,*,#9205,.F.);
#11907=ORIENTED_EDGE('',*,*,#9206,.F.);
#11908=ORIENTED_EDGE('',*,*,#9207,.T.);
#11909=ORIENTED_EDGE('',*,*,#9205,.T.);
#11910=ORIENTED_EDGE('',*,*,#9207,.F.);
#11911=ORIENTED_EDGE('',*,*,#9208,.F.);
#11912=ORIENTED_EDGE('',*,*,#9209,.T.);
#11913=ORIENTED_EDGE('',*,*,#9206,.T.);
#11914=ORIENTED_EDGE('',*,*,#9209,.F.);
#11915=ORIENTED_EDGE('',*,*,#9210,.F.);
#11916=ORIENTED_EDGE('',*,*,#9211,.T.);
#11917=ORIENTED_EDGE('',*,*,#9208,.T.);
#11918=ORIENTED_EDGE('',*,*,#9211,.F.);
#11919=ORIENTED_EDGE('',*,*,#9210,.T.);
#11920=ORIENTED_EDGE('',*,*,#9212,.F.);
#11921=ORIENTED_EDGE('',*,*,#9213,.F.);
#11922=ORIENTED_EDGE('',*,*,#9214,.T.);
#11923=ORIENTED_EDGE('',*,*,#9212,.T.);
#11924=ORIENTED_EDGE('',*,*,#9214,.F.);
#11925=ORIENTED_EDGE('',*,*,#9204,.T.);
#11926=ORIENTED_EDGE('',*,*,#9215,.T.);
#11927=ORIENTED_EDGE('',*,*,#9213,.T.);
#11928=ORIENTED_EDGE('',*,*,#9215,.F.);
#11929=ORIENTED_EDGE('',*,*,#9216,.F.);
#11930=ORIENTED_EDGE('',*,*,#9217,.F.);
#11931=ORIENTED_EDGE('',*,*,#9218,.T.);
#11932=ORIENTED_EDGE('',*,*,#9219,.T.);
#11933=ORIENTED_EDGE('',*,*,#9220,.F.);
#11934=ORIENTED_EDGE('',*,*,#9219,.F.);
#11935=ORIENTED_EDGE('',*,*,#9221,.T.);
#11936=ORIENTED_EDGE('',*,*,#9222,.T.);
#11937=ORIENTED_EDGE('',*,*,#9223,.F.);
#11938=ORIENTED_EDGE('',*,*,#9222,.F.);
#11939=ORIENTED_EDGE('',*,*,#9224,.T.);
#11940=ORIENTED_EDGE('',*,*,#9225,.T.);
#11941=ORIENTED_EDGE('',*,*,#9226,.F.);
#11942=ORIENTED_EDGE('',*,*,#9225,.F.);
#11943=ORIENTED_EDGE('',*,*,#9227,.T.);
#11944=ORIENTED_EDGE('',*,*,#9217,.T.);
#11945=ORIENTED_EDGE('',*,*,#9221,.F.);
#11946=ORIENTED_EDGE('',*,*,#9218,.F.);
#11947=ORIENTED_EDGE('',*,*,#9227,.F.);
#11948=ORIENTED_EDGE('',*,*,#9224,.F.);
#11949=ORIENTED_EDGE('',*,*,#9228,.F.);
#11950=ORIENTED_EDGE('',*,*,#9229,.F.);
#11951=ORIENTED_EDGE('',*,*,#9230,.T.);
#11952=ORIENTED_EDGE('',*,*,#9231,.T.);
#11953=ORIENTED_EDGE('',*,*,#9232,.F.);
#11954=ORIENTED_EDGE('',*,*,#9231,.F.);
#11955=ORIENTED_EDGE('',*,*,#9233,.T.);
#11956=ORIENTED_EDGE('',*,*,#9234,.T.);
#11957=ORIENTED_EDGE('',*,*,#9235,.F.);
#11958=ORIENTED_EDGE('',*,*,#9234,.F.);
#11959=ORIENTED_EDGE('',*,*,#9236,.T.);
#11960=ORIENTED_EDGE('',*,*,#9237,.T.);
#11961=ORIENTED_EDGE('',*,*,#9238,.F.);
#11962=ORIENTED_EDGE('',*,*,#9237,.F.);
#11963=ORIENTED_EDGE('',*,*,#9239,.T.);
#11964=ORIENTED_EDGE('',*,*,#9229,.T.);
#11965=ORIENTED_EDGE('',*,*,#9233,.F.);
#11966=ORIENTED_EDGE('',*,*,#9230,.F.);
#11967=ORIENTED_EDGE('',*,*,#9239,.F.);
#11968=ORIENTED_EDGE('',*,*,#9236,.F.);
#11969=ORIENTED_EDGE('',*,*,#9240,.F.);
#11970=ORIENTED_EDGE('',*,*,#9241,.F.);
#11971=ORIENTED_EDGE('',*,*,#9242,.T.);
#11972=ORIENTED_EDGE('',*,*,#9243,.T.);
#11973=ORIENTED_EDGE('',*,*,#9244,.F.);
#11974=ORIENTED_EDGE('',*,*,#9243,.F.);
#11975=ORIENTED_EDGE('',*,*,#9245,.T.);
#11976=ORIENTED_EDGE('',*,*,#9246,.T.);
#11977=ORIENTED_EDGE('',*,*,#9247,.F.);
#11978=ORIENTED_EDGE('',*,*,#9246,.F.);
#11979=ORIENTED_EDGE('',*,*,#9248,.T.);
#11980=ORIENTED_EDGE('',*,*,#9249,.T.);
#11981=ORIENTED_EDGE('',*,*,#9250,.F.);
#11982=ORIENTED_EDGE('',*,*,#9249,.F.);
#11983=ORIENTED_EDGE('',*,*,#9251,.T.);
#11984=ORIENTED_EDGE('',*,*,#9241,.T.);
#11985=ORIENTED_EDGE('',*,*,#9245,.F.);
#11986=ORIENTED_EDGE('',*,*,#9242,.F.);
#11987=ORIENTED_EDGE('',*,*,#9251,.F.);
#11988=ORIENTED_EDGE('',*,*,#9248,.F.);
#11989=ORIENTED_EDGE('',*,*,#9252,.F.);
#11990=ORIENTED_EDGE('',*,*,#9253,.F.);
#11991=ORIENTED_EDGE('',*,*,#9254,.T.);
#11992=ORIENTED_EDGE('',*,*,#9255,.T.);
#11993=ORIENTED_EDGE('',*,*,#9256,.F.);
#11994=ORIENTED_EDGE('',*,*,#9255,.F.);
#11995=ORIENTED_EDGE('',*,*,#9257,.T.);
#11996=ORIENTED_EDGE('',*,*,#9258,.T.);
#11997=ORIENTED_EDGE('',*,*,#9259,.F.);
#11998=ORIENTED_EDGE('',*,*,#9258,.F.);
#11999=ORIENTED_EDGE('',*,*,#9260,.T.);
#12000=ORIENTED_EDGE('',*,*,#9261,.T.);
#12001=ORIENTED_EDGE('',*,*,#9262,.F.);
#12002=ORIENTED_EDGE('',*,*,#9261,.F.);
#12003=ORIENTED_EDGE('',*,*,#9263,.T.);
#12004=ORIENTED_EDGE('',*,*,#9253,.T.);
#12005=ORIENTED_EDGE('',*,*,#9257,.F.);
#12006=ORIENTED_EDGE('',*,*,#9254,.F.);
#12007=ORIENTED_EDGE('',*,*,#9263,.F.);
#12008=ORIENTED_EDGE('',*,*,#9260,.F.);
#12009=ORIENTED_EDGE('',*,*,#9264,.F.);
#12010=ORIENTED_EDGE('',*,*,#9265,.F.);
#12011=ORIENTED_EDGE('',*,*,#9266,.T.);
#12012=ORIENTED_EDGE('',*,*,#9267,.T.);
#12013=ORIENTED_EDGE('',*,*,#9268,.F.);
#12014=ORIENTED_EDGE('',*,*,#9267,.F.);
#12015=ORIENTED_EDGE('',*,*,#9269,.T.);
#12016=ORIENTED_EDGE('',*,*,#9270,.T.);
#12017=ORIENTED_EDGE('',*,*,#9271,.F.);
#12018=ORIENTED_EDGE('',*,*,#9270,.F.);
#12019=ORIENTED_EDGE('',*,*,#9272,.T.);
#12020=ORIENTED_EDGE('',*,*,#9273,.T.);
#12021=ORIENTED_EDGE('',*,*,#9274,.F.);
#12022=ORIENTED_EDGE('',*,*,#9273,.F.);
#12023=ORIENTED_EDGE('',*,*,#9275,.T.);
#12024=ORIENTED_EDGE('',*,*,#9265,.T.);
#12025=ORIENTED_EDGE('',*,*,#9269,.F.);
#12026=ORIENTED_EDGE('',*,*,#9266,.F.);
#12027=ORIENTED_EDGE('',*,*,#9275,.F.);
#12028=ORIENTED_EDGE('',*,*,#9272,.F.);
#12029=ORIENTED_EDGE('',*,*,#9276,.F.);
#12030=ORIENTED_EDGE('',*,*,#9277,.F.);
#12031=ORIENTED_EDGE('',*,*,#9278,.T.);
#12032=ORIENTED_EDGE('',*,*,#9279,.T.);
#12033=ORIENTED_EDGE('',*,*,#9280,.F.);
#12034=ORIENTED_EDGE('',*,*,#9279,.F.);
#12035=ORIENTED_EDGE('',*,*,#9281,.T.);
#12036=ORIENTED_EDGE('',*,*,#9282,.T.);
#12037=ORIENTED_EDGE('',*,*,#9283,.F.);
#12038=ORIENTED_EDGE('',*,*,#9282,.F.);
#12039=ORIENTED_EDGE('',*,*,#9284,.T.);
#12040=ORIENTED_EDGE('',*,*,#9285,.T.);
#12041=ORIENTED_EDGE('',*,*,#9286,.F.);
#12042=ORIENTED_EDGE('',*,*,#9285,.F.);
#12043=ORIENTED_EDGE('',*,*,#9287,.T.);
#12044=ORIENTED_EDGE('',*,*,#9277,.T.);
#12045=ORIENTED_EDGE('',*,*,#9281,.F.);
#12046=ORIENTED_EDGE('',*,*,#9278,.F.);
#12047=ORIENTED_EDGE('',*,*,#9287,.F.);
#12048=ORIENTED_EDGE('',*,*,#9284,.F.);
#12049=ORIENTED_EDGE('',*,*,#9288,.F.);
#12050=ORIENTED_EDGE('',*,*,#9289,.F.);
#12051=ORIENTED_EDGE('',*,*,#9290,.T.);
#12052=ORIENTED_EDGE('',*,*,#9291,.T.);
#12053=ORIENTED_EDGE('',*,*,#9292,.F.);
#12054=ORIENTED_EDGE('',*,*,#9291,.F.);
#12055=ORIENTED_EDGE('',*,*,#9293,.T.);
#12056=ORIENTED_EDGE('',*,*,#9294,.T.);
#12057=ORIENTED_EDGE('',*,*,#9295,.F.);
#12058=ORIENTED_EDGE('',*,*,#9294,.F.);
#12059=ORIENTED_EDGE('',*,*,#9296,.T.);
#12060=ORIENTED_EDGE('',*,*,#9297,.T.);
#12061=ORIENTED_EDGE('',*,*,#9298,.F.);
#12062=ORIENTED_EDGE('',*,*,#9297,.F.);
#12063=ORIENTED_EDGE('',*,*,#9299,.T.);
#12064=ORIENTED_EDGE('',*,*,#9289,.T.);
#12065=ORIENTED_EDGE('',*,*,#9293,.F.);
#12066=ORIENTED_EDGE('',*,*,#9290,.F.);
#12067=ORIENTED_EDGE('',*,*,#9299,.F.);
#12068=ORIENTED_EDGE('',*,*,#9296,.F.);
#12069=ORIENTED_EDGE('',*,*,#9300,.F.);
#12070=ORIENTED_EDGE('',*,*,#9301,.F.);
#12071=ORIENTED_EDGE('',*,*,#9302,.T.);
#12072=ORIENTED_EDGE('',*,*,#9303,.T.);
#12073=ORIENTED_EDGE('',*,*,#9304,.F.);
#12074=ORIENTED_EDGE('',*,*,#9303,.F.);
#12075=ORIENTED_EDGE('',*,*,#9305,.T.);
#12076=ORIENTED_EDGE('',*,*,#9306,.T.);
#12077=ORIENTED_EDGE('',*,*,#9307,.F.);
#12078=ORIENTED_EDGE('',*,*,#9306,.F.);
#12079=ORIENTED_EDGE('',*,*,#9308,.T.);
#12080=ORIENTED_EDGE('',*,*,#9309,.T.);
#12081=ORIENTED_EDGE('',*,*,#9310,.F.);
#12082=ORIENTED_EDGE('',*,*,#9309,.F.);
#12083=ORIENTED_EDGE('',*,*,#9311,.T.);
#12084=ORIENTED_EDGE('',*,*,#9301,.T.);
#12085=ORIENTED_EDGE('',*,*,#9305,.F.);
#12086=ORIENTED_EDGE('',*,*,#9302,.F.);
#12087=ORIENTED_EDGE('',*,*,#9311,.F.);
#12088=ORIENTED_EDGE('',*,*,#9308,.F.);
#12089=ORIENTED_EDGE('',*,*,#9312,.F.);
#12090=ORIENTED_EDGE('',*,*,#9313,.F.);
#12091=ORIENTED_EDGE('',*,*,#9314,.T.);
#12092=ORIENTED_EDGE('',*,*,#9315,.T.);
#12093=ORIENTED_EDGE('',*,*,#9316,.F.);
#12094=ORIENTED_EDGE('',*,*,#9315,.F.);
#12095=ORIENTED_EDGE('',*,*,#9317,.T.);
#12096=ORIENTED_EDGE('',*,*,#9318,.T.);
#12097=ORIENTED_EDGE('',*,*,#9319,.F.);
#12098=ORIENTED_EDGE('',*,*,#9318,.F.);
#12099=ORIENTED_EDGE('',*,*,#9320,.T.);
#12100=ORIENTED_EDGE('',*,*,#9321,.T.);
#12101=ORIENTED_EDGE('',*,*,#9322,.F.);
#12102=ORIENTED_EDGE('',*,*,#9321,.F.);
#12103=ORIENTED_EDGE('',*,*,#9323,.T.);
#12104=ORIENTED_EDGE('',*,*,#9313,.T.);
#12105=ORIENTED_EDGE('',*,*,#9317,.F.);
#12106=ORIENTED_EDGE('',*,*,#9314,.F.);
#12107=ORIENTED_EDGE('',*,*,#9323,.F.);
#12108=ORIENTED_EDGE('',*,*,#9320,.F.);
#12109=ORIENTED_EDGE('',*,*,#9324,.F.);
#12110=ORIENTED_EDGE('',*,*,#9325,.F.);
#12111=ORIENTED_EDGE('',*,*,#9326,.T.);
#12112=ORIENTED_EDGE('',*,*,#9327,.T.);
#12113=ORIENTED_EDGE('',*,*,#9328,.F.);
#12114=ORIENTED_EDGE('',*,*,#9327,.F.);
#12115=ORIENTED_EDGE('',*,*,#9329,.T.);
#12116=ORIENTED_EDGE('',*,*,#9330,.T.);
#12117=ORIENTED_EDGE('',*,*,#9331,.F.);
#12118=ORIENTED_EDGE('',*,*,#9330,.F.);
#12119=ORIENTED_EDGE('',*,*,#9332,.T.);
#12120=ORIENTED_EDGE('',*,*,#9333,.T.);
#12121=ORIENTED_EDGE('',*,*,#9334,.F.);
#12122=ORIENTED_EDGE('',*,*,#9333,.F.);
#12123=ORIENTED_EDGE('',*,*,#9335,.T.);
#12124=ORIENTED_EDGE('',*,*,#9325,.T.);
#12125=ORIENTED_EDGE('',*,*,#9329,.F.);
#12126=ORIENTED_EDGE('',*,*,#9326,.F.);
#12127=ORIENTED_EDGE('',*,*,#9335,.F.);
#12128=ORIENTED_EDGE('',*,*,#9332,.F.);
#12129=ORIENTED_EDGE('',*,*,#9336,.F.);
#12130=ORIENTED_EDGE('',*,*,#9337,.F.);
#12131=ORIENTED_EDGE('',*,*,#9338,.T.);
#12132=ORIENTED_EDGE('',*,*,#9339,.T.);
#12133=ORIENTED_EDGE('',*,*,#9340,.F.);
#12134=ORIENTED_EDGE('',*,*,#9339,.F.);
#12135=ORIENTED_EDGE('',*,*,#9341,.T.);
#12136=ORIENTED_EDGE('',*,*,#9342,.T.);
#12137=ORIENTED_EDGE('',*,*,#9343,.F.);
#12138=ORIENTED_EDGE('',*,*,#9342,.F.);
#12139=ORIENTED_EDGE('',*,*,#9344,.T.);
#12140=ORIENTED_EDGE('',*,*,#9345,.T.);
#12141=ORIENTED_EDGE('',*,*,#9346,.F.);
#12142=ORIENTED_EDGE('',*,*,#9345,.F.);
#12143=ORIENTED_EDGE('',*,*,#9347,.T.);
#12144=ORIENTED_EDGE('',*,*,#9337,.T.);
#12145=ORIENTED_EDGE('',*,*,#9341,.F.);
#12146=ORIENTED_EDGE('',*,*,#9338,.F.);
#12147=ORIENTED_EDGE('',*,*,#9347,.F.);
#12148=ORIENTED_EDGE('',*,*,#9344,.F.);
#12149=ORIENTED_EDGE('',*,*,#9348,.F.);
#12150=ORIENTED_EDGE('',*,*,#9349,.F.);
#12151=ORIENTED_EDGE('',*,*,#9350,.T.);
#12152=ORIENTED_EDGE('',*,*,#9351,.T.);
#12153=ORIENTED_EDGE('',*,*,#9352,.F.);
#12154=ORIENTED_EDGE('',*,*,#9351,.F.);
#12155=ORIENTED_EDGE('',*,*,#9353,.T.);
#12156=ORIENTED_EDGE('',*,*,#9354,.T.);
#12157=ORIENTED_EDGE('',*,*,#9355,.F.);
#12158=ORIENTED_EDGE('',*,*,#9354,.F.);
#12159=ORIENTED_EDGE('',*,*,#9356,.T.);
#12160=ORIENTED_EDGE('',*,*,#9357,.T.);
#12161=ORIENTED_EDGE('',*,*,#9358,.F.);
#12162=ORIENTED_EDGE('',*,*,#9357,.F.);
#12163=ORIENTED_EDGE('',*,*,#9359,.T.);
#12164=ORIENTED_EDGE('',*,*,#9349,.T.);
#12165=ORIENTED_EDGE('',*,*,#9353,.F.);
#12166=ORIENTED_EDGE('',*,*,#9350,.F.);
#12167=ORIENTED_EDGE('',*,*,#9359,.F.);
#12168=ORIENTED_EDGE('',*,*,#9356,.F.);
#12169=ORIENTED_EDGE('',*,*,#9360,.F.);
#12170=ORIENTED_EDGE('',*,*,#9361,.F.);
#12171=ORIENTED_EDGE('',*,*,#9362,.T.);
#12172=ORIENTED_EDGE('',*,*,#9363,.T.);
#12173=ORIENTED_EDGE('',*,*,#9364,.F.);
#12174=ORIENTED_EDGE('',*,*,#9363,.F.);
#12175=ORIENTED_EDGE('',*,*,#9365,.T.);
#12176=ORIENTED_EDGE('',*,*,#9366,.T.);
#12177=ORIENTED_EDGE('',*,*,#9367,.F.);
#12178=ORIENTED_EDGE('',*,*,#9366,.F.);
#12179=ORIENTED_EDGE('',*,*,#9368,.T.);
#12180=ORIENTED_EDGE('',*,*,#9369,.T.);
#12181=ORIENTED_EDGE('',*,*,#9370,.F.);
#12182=ORIENTED_EDGE('',*,*,#9369,.F.);
#12183=ORIENTED_EDGE('',*,*,#9371,.T.);
#12184=ORIENTED_EDGE('',*,*,#9361,.T.);
#12185=ORIENTED_EDGE('',*,*,#9365,.F.);
#12186=ORIENTED_EDGE('',*,*,#9362,.F.);
#12187=ORIENTED_EDGE('',*,*,#9371,.F.);
#12188=ORIENTED_EDGE('',*,*,#9368,.F.);
#12189=ORIENTED_EDGE('',*,*,#9372,.F.);
#12190=ORIENTED_EDGE('',*,*,#9373,.F.);
#12191=ORIENTED_EDGE('',*,*,#9374,.T.);
#12192=ORIENTED_EDGE('',*,*,#9375,.T.);
#12193=ORIENTED_EDGE('',*,*,#9376,.F.);
#12194=ORIENTED_EDGE('',*,*,#9375,.F.);
#12195=ORIENTED_EDGE('',*,*,#9377,.T.);
#12196=ORIENTED_EDGE('',*,*,#9378,.T.);
#12197=ORIENTED_EDGE('',*,*,#9379,.F.);
#12198=ORIENTED_EDGE('',*,*,#9378,.F.);
#12199=ORIENTED_EDGE('',*,*,#9380,.T.);
#12200=ORIENTED_EDGE('',*,*,#9381,.T.);
#12201=ORIENTED_EDGE('',*,*,#9382,.F.);
#12202=ORIENTED_EDGE('',*,*,#9381,.F.);
#12203=ORIENTED_EDGE('',*,*,#9383,.T.);
#12204=ORIENTED_EDGE('',*,*,#9373,.T.);
#12205=ORIENTED_EDGE('',*,*,#9377,.F.);
#12206=ORIENTED_EDGE('',*,*,#9374,.F.);
#12207=ORIENTED_EDGE('',*,*,#9383,.F.);
#12208=ORIENTED_EDGE('',*,*,#9380,.F.);
#12209=ORIENTED_EDGE('',*,*,#9384,.F.);
#12210=ORIENTED_EDGE('',*,*,#9385,.F.);
#12211=ORIENTED_EDGE('',*,*,#9386,.T.);
#12212=ORIENTED_EDGE('',*,*,#9387,.T.);
#12213=ORIENTED_EDGE('',*,*,#9388,.F.);
#12214=ORIENTED_EDGE('',*,*,#9387,.F.);
#12215=ORIENTED_EDGE('',*,*,#9389,.T.);
#12216=ORIENTED_EDGE('',*,*,#9390,.T.);
#12217=ORIENTED_EDGE('',*,*,#9391,.F.);
#12218=ORIENTED_EDGE('',*,*,#9390,.F.);
#12219=ORIENTED_EDGE('',*,*,#9392,.T.);
#12220=ORIENTED_EDGE('',*,*,#9393,.T.);
#12221=ORIENTED_EDGE('',*,*,#9394,.F.);
#12222=ORIENTED_EDGE('',*,*,#9393,.F.);
#12223=ORIENTED_EDGE('',*,*,#9395,.T.);
#12224=ORIENTED_EDGE('',*,*,#9385,.T.);
#12225=ORIENTED_EDGE('',*,*,#9389,.F.);
#12226=ORIENTED_EDGE('',*,*,#9386,.F.);
#12227=ORIENTED_EDGE('',*,*,#9395,.F.);
#12228=ORIENTED_EDGE('',*,*,#9392,.F.);
#12229=ORIENTED_EDGE('',*,*,#9396,.F.);
#12230=ORIENTED_EDGE('',*,*,#9397,.F.);
#12231=ORIENTED_EDGE('',*,*,#9398,.T.);
#12232=ORIENTED_EDGE('',*,*,#9399,.T.);
#12233=ORIENTED_EDGE('',*,*,#9400,.F.);
#12234=ORIENTED_EDGE('',*,*,#9399,.F.);
#12235=ORIENTED_EDGE('',*,*,#9401,.T.);
#12236=ORIENTED_EDGE('',*,*,#9402,.T.);
#12237=ORIENTED_EDGE('',*,*,#9403,.F.);
#12238=ORIENTED_EDGE('',*,*,#9402,.F.);
#12239=ORIENTED_EDGE('',*,*,#9404,.T.);
#12240=ORIENTED_EDGE('',*,*,#9405,.T.);
#12241=ORIENTED_EDGE('',*,*,#9406,.F.);
#12242=ORIENTED_EDGE('',*,*,#9405,.F.);
#12243=ORIENTED_EDGE('',*,*,#9407,.T.);
#12244=ORIENTED_EDGE('',*,*,#9397,.T.);
#12245=ORIENTED_EDGE('',*,*,#9401,.F.);
#12246=ORIENTED_EDGE('',*,*,#9398,.F.);
#12247=ORIENTED_EDGE('',*,*,#9407,.F.);
#12248=ORIENTED_EDGE('',*,*,#9404,.F.);
#12249=ORIENTED_EDGE('',*,*,#9408,.F.);
#12250=ORIENTED_EDGE('',*,*,#9409,.F.);
#12251=ORIENTED_EDGE('',*,*,#9410,.T.);
#12252=ORIENTED_EDGE('',*,*,#9411,.T.);
#12253=ORIENTED_EDGE('',*,*,#9412,.F.);
#12254=ORIENTED_EDGE('',*,*,#9411,.F.);
#12255=ORIENTED_EDGE('',*,*,#9413,.T.);
#12256=ORIENTED_EDGE('',*,*,#9414,.T.);
#12257=ORIENTED_EDGE('',*,*,#9415,.F.);
#12258=ORIENTED_EDGE('',*,*,#9414,.F.);
#12259=ORIENTED_EDGE('',*,*,#9416,.T.);
#12260=ORIENTED_EDGE('',*,*,#9417,.T.);
#12261=ORIENTED_EDGE('',*,*,#9418,.F.);
#12262=ORIENTED_EDGE('',*,*,#9417,.F.);
#12263=ORIENTED_EDGE('',*,*,#9419,.T.);
#12264=ORIENTED_EDGE('',*,*,#9409,.T.);
#12265=ORIENTED_EDGE('',*,*,#9413,.F.);
#12266=ORIENTED_EDGE('',*,*,#9410,.F.);
#12267=ORIENTED_EDGE('',*,*,#9419,.F.);
#12268=ORIENTED_EDGE('',*,*,#9416,.F.);
#12269=ORIENTED_EDGE('',*,*,#9420,.F.);
#12270=ORIENTED_EDGE('',*,*,#9421,.F.);
#12271=ORIENTED_EDGE('',*,*,#9422,.T.);
#12272=ORIENTED_EDGE('',*,*,#9423,.T.);
#12273=ORIENTED_EDGE('',*,*,#9424,.F.);
#12274=ORIENTED_EDGE('',*,*,#9423,.F.);
#12275=ORIENTED_EDGE('',*,*,#9425,.T.);
#12276=ORIENTED_EDGE('',*,*,#9426,.T.);
#12277=ORIENTED_EDGE('',*,*,#9427,.F.);
#12278=ORIENTED_EDGE('',*,*,#9426,.F.);
#12279=ORIENTED_EDGE('',*,*,#9428,.T.);
#12280=ORIENTED_EDGE('',*,*,#9429,.T.);
#12281=ORIENTED_EDGE('',*,*,#9430,.F.);
#12282=ORIENTED_EDGE('',*,*,#9429,.F.);
#12283=ORIENTED_EDGE('',*,*,#9431,.T.);
#12284=ORIENTED_EDGE('',*,*,#9421,.T.);
#12285=ORIENTED_EDGE('',*,*,#9425,.F.);
#12286=ORIENTED_EDGE('',*,*,#9422,.F.);
#12287=ORIENTED_EDGE('',*,*,#9431,.F.);
#12288=ORIENTED_EDGE('',*,*,#9428,.F.);
#12289=ORIENTED_EDGE('',*,*,#9432,.F.);
#12290=ORIENTED_EDGE('',*,*,#9433,.F.);
#12291=ORIENTED_EDGE('',*,*,#9434,.T.);
#12292=ORIENTED_EDGE('',*,*,#9435,.T.);
#12293=ORIENTED_EDGE('',*,*,#9436,.F.);
#12294=ORIENTED_EDGE('',*,*,#9435,.F.);
#12295=ORIENTED_EDGE('',*,*,#9437,.T.);
#12296=ORIENTED_EDGE('',*,*,#9438,.T.);
#12297=ORIENTED_EDGE('',*,*,#9439,.F.);
#12298=ORIENTED_EDGE('',*,*,#9438,.F.);
#12299=ORIENTED_EDGE('',*,*,#9440,.T.);
#12300=ORIENTED_EDGE('',*,*,#9441,.T.);
#12301=ORIENTED_EDGE('',*,*,#9442,.F.);
#12302=ORIENTED_EDGE('',*,*,#9441,.F.);
#12303=ORIENTED_EDGE('',*,*,#9443,.T.);
#12304=ORIENTED_EDGE('',*,*,#9433,.T.);
#12305=ORIENTED_EDGE('',*,*,#9437,.F.);
#12306=ORIENTED_EDGE('',*,*,#9434,.F.);
#12307=ORIENTED_EDGE('',*,*,#9443,.F.);
#12308=ORIENTED_EDGE('',*,*,#9440,.F.);
#12309=ORIENTED_EDGE('',*,*,#9444,.F.);
#12310=ORIENTED_EDGE('',*,*,#9445,.F.);
#12311=ORIENTED_EDGE('',*,*,#9446,.T.);
#12312=ORIENTED_EDGE('',*,*,#9447,.T.);
#12313=ORIENTED_EDGE('',*,*,#9448,.F.);
#12314=ORIENTED_EDGE('',*,*,#9447,.F.);
#12315=ORIENTED_EDGE('',*,*,#9449,.T.);
#12316=ORIENTED_EDGE('',*,*,#9450,.T.);
#12317=ORIENTED_EDGE('',*,*,#9451,.F.);
#12318=ORIENTED_EDGE('',*,*,#9450,.F.);
#12319=ORIENTED_EDGE('',*,*,#9452,.T.);
#12320=ORIENTED_EDGE('',*,*,#9453,.T.);
#12321=ORIENTED_EDGE('',*,*,#9454,.F.);
#12322=ORIENTED_EDGE('',*,*,#9453,.F.);
#12323=ORIENTED_EDGE('',*,*,#9455,.T.);
#12324=ORIENTED_EDGE('',*,*,#9445,.T.);
#12325=ORIENTED_EDGE('',*,*,#9449,.F.);
#12326=ORIENTED_EDGE('',*,*,#9446,.F.);
#12327=ORIENTED_EDGE('',*,*,#9455,.F.);
#12328=ORIENTED_EDGE('',*,*,#9452,.F.);
#12329=ORIENTED_EDGE('',*,*,#9456,.F.);
#12330=ORIENTED_EDGE('',*,*,#9457,.F.);
#12331=ORIENTED_EDGE('',*,*,#9458,.T.);
#12332=ORIENTED_EDGE('',*,*,#9459,.T.);
#12333=ORIENTED_EDGE('',*,*,#9460,.F.);
#12334=ORIENTED_EDGE('',*,*,#9459,.F.);
#12335=ORIENTED_EDGE('',*,*,#9461,.T.);
#12336=ORIENTED_EDGE('',*,*,#9462,.T.);
#12337=ORIENTED_EDGE('',*,*,#9463,.F.);
#12338=ORIENTED_EDGE('',*,*,#9462,.F.);
#12339=ORIENTED_EDGE('',*,*,#9464,.T.);
#12340=ORIENTED_EDGE('',*,*,#9465,.T.);
#12341=ORIENTED_EDGE('',*,*,#9466,.F.);
#12342=ORIENTED_EDGE('',*,*,#9465,.F.);
#12343=ORIENTED_EDGE('',*,*,#9467,.T.);
#12344=ORIENTED_EDGE('',*,*,#9457,.T.);
#12345=ORIENTED_EDGE('',*,*,#9461,.F.);
#12346=ORIENTED_EDGE('',*,*,#9458,.F.);
#12347=ORIENTED_EDGE('',*,*,#9467,.F.);
#12348=ORIENTED_EDGE('',*,*,#9464,.F.);
#12349=ORIENTED_EDGE('',*,*,#9468,.F.);
#12350=ORIENTED_EDGE('',*,*,#9469,.F.);
#12351=ORIENTED_EDGE('',*,*,#9470,.T.);
#12352=ORIENTED_EDGE('',*,*,#9471,.T.);
#12353=ORIENTED_EDGE('',*,*,#9472,.F.);
#12354=ORIENTED_EDGE('',*,*,#9471,.F.);
#12355=ORIENTED_EDGE('',*,*,#9473,.T.);
#12356=ORIENTED_EDGE('',*,*,#9474,.T.);
#12357=ORIENTED_EDGE('',*,*,#9475,.F.);
#12358=ORIENTED_EDGE('',*,*,#9474,.F.);
#12359=ORIENTED_EDGE('',*,*,#9476,.T.);
#12360=ORIENTED_EDGE('',*,*,#9477,.T.);
#12361=ORIENTED_EDGE('',*,*,#9478,.F.);
#12362=ORIENTED_EDGE('',*,*,#9477,.F.);
#12363=ORIENTED_EDGE('',*,*,#9479,.T.);
#12364=ORIENTED_EDGE('',*,*,#9469,.T.);
#12365=ORIENTED_EDGE('',*,*,#9473,.F.);
#12366=ORIENTED_EDGE('',*,*,#9470,.F.);
#12367=ORIENTED_EDGE('',*,*,#9479,.F.);
#12368=ORIENTED_EDGE('',*,*,#9476,.F.);
#12369=ORIENTED_EDGE('',*,*,#9480,.F.);
#12370=ORIENTED_EDGE('',*,*,#9481,.F.);
#12371=ORIENTED_EDGE('',*,*,#9482,.T.);
#12372=ORIENTED_EDGE('',*,*,#9483,.T.);
#12373=ORIENTED_EDGE('',*,*,#9484,.F.);
#12374=ORIENTED_EDGE('',*,*,#9483,.F.);
#12375=ORIENTED_EDGE('',*,*,#9485,.T.);
#12376=ORIENTED_EDGE('',*,*,#9486,.T.);
#12377=ORIENTED_EDGE('',*,*,#9487,.F.);
#12378=ORIENTED_EDGE('',*,*,#9486,.F.);
#12379=ORIENTED_EDGE('',*,*,#9488,.T.);
#12380=ORIENTED_EDGE('',*,*,#9489,.T.);
#12381=ORIENTED_EDGE('',*,*,#9490,.F.);
#12382=ORIENTED_EDGE('',*,*,#9489,.F.);
#12383=ORIENTED_EDGE('',*,*,#9491,.T.);
#12384=ORIENTED_EDGE('',*,*,#9481,.T.);
#12385=ORIENTED_EDGE('',*,*,#9485,.F.);
#12386=ORIENTED_EDGE('',*,*,#9482,.F.);
#12387=ORIENTED_EDGE('',*,*,#9491,.F.);
#12388=ORIENTED_EDGE('',*,*,#9488,.F.);
#12389=ORIENTED_EDGE('',*,*,#9492,.F.);
#12390=ORIENTED_EDGE('',*,*,#9493,.F.);
#12391=ORIENTED_EDGE('',*,*,#9494,.T.);
#12392=ORIENTED_EDGE('',*,*,#9495,.T.);
#12393=ORIENTED_EDGE('',*,*,#9496,.F.);
#12394=ORIENTED_EDGE('',*,*,#9495,.F.);
#12395=ORIENTED_EDGE('',*,*,#9497,.T.);
#12396=ORIENTED_EDGE('',*,*,#9498,.T.);
#12397=ORIENTED_EDGE('',*,*,#9499,.F.);
#12398=ORIENTED_EDGE('',*,*,#9498,.F.);
#12399=ORIENTED_EDGE('',*,*,#9500,.T.);
#12400=ORIENTED_EDGE('',*,*,#9501,.T.);
#12401=ORIENTED_EDGE('',*,*,#9502,.F.);
#12402=ORIENTED_EDGE('',*,*,#9501,.F.);
#12403=ORIENTED_EDGE('',*,*,#9503,.T.);
#12404=ORIENTED_EDGE('',*,*,#9493,.T.);
#12405=ORIENTED_EDGE('',*,*,#9497,.F.);
#12406=ORIENTED_EDGE('',*,*,#9494,.F.);
#12407=ORIENTED_EDGE('',*,*,#9503,.F.);
#12408=ORIENTED_EDGE('',*,*,#9500,.F.);
#12409=ORIENTED_EDGE('',*,*,#9504,.F.);
#12410=ORIENTED_EDGE('',*,*,#9505,.T.);
#12411=ORIENTED_EDGE('',*,*,#9506,.F.);
#12412=ORIENTED_EDGE('',*,*,#9505,.F.);
#12413=ORIENTED_EDGE('',*,*,#9507,.F.);
#12414=ORIENTED_EDGE('',*,*,#9508,.T.);
#12415=ORIENTED_EDGE('',*,*,#9509,.F.);
#12416=ORIENTED_EDGE('',*,*,#9508,.F.);
#12417=ORIENTED_EDGE('',*,*,#9510,.F.);
#12418=ORIENTED_EDGE('',*,*,#9511,.T.);
#12419=ORIENTED_EDGE('',*,*,#9512,.F.);
#12420=ORIENTED_EDGE('',*,*,#9511,.F.);
#12421=ORIENTED_EDGE('',*,*,#9513,.F.);
#12422=ORIENTED_EDGE('',*,*,#9514,.F.);
#12423=ORIENTED_EDGE('',*,*,#9515,.T.);
#12424=ORIENTED_EDGE('',*,*,#9516,.F.);
#12425=ORIENTED_EDGE('',*,*,#9517,.F.);
#12426=ORIENTED_EDGE('',*,*,#9518,.F.);
#12427=ORIENTED_EDGE('',*,*,#9519,.F.);
#12428=ORIENTED_EDGE('',*,*,#9520,.F.);
#12429=ORIENTED_EDGE('',*,*,#9521,.F.);
#12430=ORIENTED_EDGE('',*,*,#9519,.T.);
#12431=ORIENTED_EDGE('',*,*,#9522,.F.);
#12432=ORIENTED_EDGE('',*,*,#9523,.F.);
#12433=ORIENTED_EDGE('',*,*,#9524,.F.);
#12434=ORIENTED_EDGE('',*,*,#9523,.T.);
#12435=ORIENTED_EDGE('',*,*,#9525,.F.);
#12436=ORIENTED_EDGE('',*,*,#9526,.F.);
#12437=ORIENTED_EDGE('',*,*,#9527,.F.);
#12438=ORIENTED_EDGE('',*,*,#9526,.T.);
#12439=ORIENTED_EDGE('',*,*,#9528,.F.);
#12440=ORIENTED_EDGE('',*,*,#9515,.F.);
#12441=ORIENTED_EDGE('',*,*,#9517,.T.);
#12442=ORIENTED_EDGE('',*,*,#9529,.F.);
#12443=ORIENTED_EDGE('',*,*,#9530,.F.);
#12444=ORIENTED_EDGE('',*,*,#9531,.F.);
#12445=ORIENTED_EDGE('',*,*,#9520,.T.);
#12446=ORIENTED_EDGE('',*,*,#9521,.T.);
#12447=ORIENTED_EDGE('',*,*,#9524,.T.);
#12448=ORIENTED_EDGE('',*,*,#9527,.T.);
#12449=ORIENTED_EDGE('',*,*,#9514,.T.);
#12450=ORIENTED_EDGE('',*,*,#9532,.T.);
#12451=ORIENTED_EDGE('',*,*,#9533,.F.);
#12452=ORIENTED_EDGE('',*,*,#9529,.T.);
#12453=ORIENTED_EDGE('',*,*,#9504,.T.);
#12454=ORIENTED_EDGE('',*,*,#9507,.T.);
#12455=ORIENTED_EDGE('',*,*,#9510,.T.);
#12456=ORIENTED_EDGE('',*,*,#9513,.T.);
#12457=ORIENTED_EDGE('',*,*,#9534,.F.);
#12458=ORIENTED_EDGE('',*,*,#9535,.F.);
#12459=ORIENTED_EDGE('',*,*,#9532,.F.);
#12460=ORIENTED_EDGE('',*,*,#9531,.T.);
#12461=ORIENTED_EDGE('',*,*,#9536,.T.);
#12462=ORIENTED_EDGE('',*,*,#9534,.T.);
#12463=ORIENTED_EDGE('',*,*,#9516,.T.);
#12464=ORIENTED_EDGE('',*,*,#9528,.T.);
#12465=ORIENTED_EDGE('',*,*,#9525,.T.);
#12466=ORIENTED_EDGE('',*,*,#9522,.T.);
#12467=ORIENTED_EDGE('',*,*,#9518,.T.);
#12468=ORIENTED_EDGE('',*,*,#9235,.T.);
#12469=ORIENTED_EDGE('',*,*,#9238,.T.);
#12470=ORIENTED_EDGE('',*,*,#9228,.T.);
#12471=ORIENTED_EDGE('',*,*,#9232,.T.);
#12472=ORIENTED_EDGE('',*,*,#9259,.T.);
#12473=ORIENTED_EDGE('',*,*,#9262,.T.);
#12474=ORIENTED_EDGE('',*,*,#9252,.T.);
#12475=ORIENTED_EDGE('',*,*,#9256,.T.);
#12476=ORIENTED_EDGE('',*,*,#9283,.T.);
#12477=ORIENTED_EDGE('',*,*,#9286,.T.);
#12478=ORIENTED_EDGE('',*,*,#9276,.T.);
#12479=ORIENTED_EDGE('',*,*,#9280,.T.);
#12480=ORIENTED_EDGE('',*,*,#9307,.T.);
#12481=ORIENTED_EDGE('',*,*,#9310,.T.);
#12482=ORIENTED_EDGE('',*,*,#9300,.T.);
#12483=ORIENTED_EDGE('',*,*,#9304,.T.);
#12484=ORIENTED_EDGE('',*,*,#9331,.T.);
#12485=ORIENTED_EDGE('',*,*,#9334,.T.);
#12486=ORIENTED_EDGE('',*,*,#9324,.T.);
#12487=ORIENTED_EDGE('',*,*,#9328,.T.);
#12488=ORIENTED_EDGE('',*,*,#9355,.T.);
#12489=ORIENTED_EDGE('',*,*,#9358,.T.);
#12490=ORIENTED_EDGE('',*,*,#9348,.T.);
#12491=ORIENTED_EDGE('',*,*,#9352,.T.);
#12492=ORIENTED_EDGE('',*,*,#9379,.T.);
#12493=ORIENTED_EDGE('',*,*,#9382,.T.);
#12494=ORIENTED_EDGE('',*,*,#9372,.T.);
#12495=ORIENTED_EDGE('',*,*,#9376,.T.);
#12496=ORIENTED_EDGE('',*,*,#9403,.T.);
#12497=ORIENTED_EDGE('',*,*,#9406,.T.);
#12498=ORIENTED_EDGE('',*,*,#9396,.T.);
#12499=ORIENTED_EDGE('',*,*,#9400,.T.);
#12500=ORIENTED_EDGE('',*,*,#9427,.T.);
#12501=ORIENTED_EDGE('',*,*,#9430,.T.);
#12502=ORIENTED_EDGE('',*,*,#9420,.T.);
#12503=ORIENTED_EDGE('',*,*,#9424,.T.);
#12504=ORIENTED_EDGE('',*,*,#9451,.T.);
#12505=ORIENTED_EDGE('',*,*,#9454,.T.);
#12506=ORIENTED_EDGE('',*,*,#9444,.T.);
#12507=ORIENTED_EDGE('',*,*,#9448,.T.);
#12508=ORIENTED_EDGE('',*,*,#9463,.T.);
#12509=ORIENTED_EDGE('',*,*,#9466,.T.);
#12510=ORIENTED_EDGE('',*,*,#9456,.T.);
#12511=ORIENTED_EDGE('',*,*,#9460,.T.);
#12512=ORIENTED_EDGE('',*,*,#9475,.T.);
#12513=ORIENTED_EDGE('',*,*,#9478,.T.);
#12514=ORIENTED_EDGE('',*,*,#9468,.T.);
#12515=ORIENTED_EDGE('',*,*,#9472,.T.);
#12516=ORIENTED_EDGE('',*,*,#9487,.T.);
#12517=ORIENTED_EDGE('',*,*,#9490,.T.);
#12518=ORIENTED_EDGE('',*,*,#9480,.T.);
#12519=ORIENTED_EDGE('',*,*,#9484,.T.);
#12520=ORIENTED_EDGE('',*,*,#9499,.T.);
#12521=ORIENTED_EDGE('',*,*,#9502,.T.);
#12522=ORIENTED_EDGE('',*,*,#9492,.T.);
#12523=ORIENTED_EDGE('',*,*,#9496,.T.);
#12524=ORIENTED_EDGE('',*,*,#9506,.T.);
#12525=ORIENTED_EDGE('',*,*,#9509,.T.);
#12526=ORIENTED_EDGE('',*,*,#9512,.T.);
#12527=ORIENTED_EDGE('',*,*,#9439,.T.);
#12528=ORIENTED_EDGE('',*,*,#9442,.T.);
#12529=ORIENTED_EDGE('',*,*,#9432,.T.);
#12530=ORIENTED_EDGE('',*,*,#9436,.T.);
#12531=ORIENTED_EDGE('',*,*,#9415,.T.);
#12532=ORIENTED_EDGE('',*,*,#9418,.T.);
#12533=ORIENTED_EDGE('',*,*,#9408,.T.);
#12534=ORIENTED_EDGE('',*,*,#9412,.T.);
#12535=ORIENTED_EDGE('',*,*,#9391,.T.);
#12536=ORIENTED_EDGE('',*,*,#9394,.T.);
#12537=ORIENTED_EDGE('',*,*,#9384,.T.);
#12538=ORIENTED_EDGE('',*,*,#9388,.T.);
#12539=ORIENTED_EDGE('',*,*,#9367,.T.);
#12540=ORIENTED_EDGE('',*,*,#9370,.T.);
#12541=ORIENTED_EDGE('',*,*,#9360,.T.);
#12542=ORIENTED_EDGE('',*,*,#9364,.T.);
#12543=ORIENTED_EDGE('',*,*,#9343,.T.);
#12544=ORIENTED_EDGE('',*,*,#9346,.T.);
#12545=ORIENTED_EDGE('',*,*,#9336,.T.);
#12546=ORIENTED_EDGE('',*,*,#9340,.T.);
#12547=ORIENTED_EDGE('',*,*,#9319,.T.);
#12548=ORIENTED_EDGE('',*,*,#9322,.T.);
#12549=ORIENTED_EDGE('',*,*,#9312,.T.);
#12550=ORIENTED_EDGE('',*,*,#9316,.T.);
#12551=ORIENTED_EDGE('',*,*,#9295,.T.);
#12552=ORIENTED_EDGE('',*,*,#9298,.T.);
#12553=ORIENTED_EDGE('',*,*,#9288,.T.);
#12554=ORIENTED_EDGE('',*,*,#9292,.T.);
#12555=ORIENTED_EDGE('',*,*,#9271,.T.);
#12556=ORIENTED_EDGE('',*,*,#9274,.T.);
#12557=ORIENTED_EDGE('',*,*,#9264,.T.);
#12558=ORIENTED_EDGE('',*,*,#9268,.T.);
#12559=ORIENTED_EDGE('',*,*,#9247,.T.);
#12560=ORIENTED_EDGE('',*,*,#9250,.T.);
#12561=ORIENTED_EDGE('',*,*,#9240,.T.);
#12562=ORIENTED_EDGE('',*,*,#9244,.T.);
#12563=ORIENTED_EDGE('',*,*,#9223,.T.);
#12564=ORIENTED_EDGE('',*,*,#9226,.T.);
#12565=ORIENTED_EDGE('',*,*,#9216,.T.);
#12566=ORIENTED_EDGE('',*,*,#9220,.T.);
#12567=ORIENTED_EDGE('',*,*,#9530,.T.);
#12568=ORIENTED_EDGE('',*,*,#9533,.T.);
#12569=ORIENTED_EDGE('',*,*,#9535,.T.);
#12570=ORIENTED_EDGE('',*,*,#9536,.F.);
#12571=ORIENTED_EDGE('',*,*,#9537,.F.);
#12572=ORIENTED_EDGE('',*,*,#9538,.T.);
#12573=ORIENTED_EDGE('',*,*,#9539,.F.);
#12574=ORIENTED_EDGE('',*,*,#9538,.F.);
#12575=ORIENTED_EDGE('',*,*,#9540,.F.);
#12576=ORIENTED_EDGE('',*,*,#9541,.T.);
#12577=ORIENTED_EDGE('',*,*,#9542,.T.);
#12578=ORIENTED_EDGE('',*,*,#9541,.F.);
#12579=ORIENTED_EDGE('',*,*,#9540,.T.);
#12580=ORIENTED_EDGE('',*,*,#9539,.T.);
#12581=ORIENTED_EDGE('',*,*,#9542,.F.);
#12582=ORIENTED_EDGE('',*,*,#9537,.T.);
#12583=ORIENTED_EDGE('',*,*,#9543,.F.);
#12584=ORIENTED_EDGE('',*,*,#9544,.T.);
#12585=ORIENTED_EDGE('',*,*,#9545,.F.);
#12586=ORIENTED_EDGE('',*,*,#9544,.F.);
#12587=ORIENTED_EDGE('',*,*,#9546,.F.);
#12588=ORIENTED_EDGE('',*,*,#9547,.T.);
#12589=ORIENTED_EDGE('',*,*,#9548,.T.);
#12590=ORIENTED_EDGE('',*,*,#9547,.F.);
#12591=ORIENTED_EDGE('',*,*,#9546,.T.);
#12592=ORIENTED_EDGE('',*,*,#9545,.T.);
#12593=ORIENTED_EDGE('',*,*,#9548,.F.);
#12594=ORIENTED_EDGE('',*,*,#9543,.T.);
#12595=ORIENTED_EDGE('',*,*,#9549,.T.);
#12596=ORIENTED_EDGE('',*,*,#9550,.T.);
#12597=ORIENTED_EDGE('',*,*,#9551,.F.);
#12598=ORIENTED_EDGE('',*,*,#9552,.F.);
#12599=ORIENTED_EDGE('',*,*,#9553,.T.);
#12600=ORIENTED_EDGE('',*,*,#9552,.T.);
#12601=ORIENTED_EDGE('',*,*,#9554,.F.);
#12602=ORIENTED_EDGE('',*,*,#9555,.F.);
#12603=ORIENTED_EDGE('',*,*,#9556,.T.);
#12604=ORIENTED_EDGE('',*,*,#9555,.T.);
#12605=ORIENTED_EDGE('',*,*,#9557,.F.);
#12606=ORIENTED_EDGE('',*,*,#9558,.F.);
#12607=ORIENTED_EDGE('',*,*,#9559,.T.);
#12608=ORIENTED_EDGE('',*,*,#9558,.T.);
#12609=ORIENTED_EDGE('',*,*,#9560,.F.);
#12610=ORIENTED_EDGE('',*,*,#9550,.F.);
#12611=ORIENTED_EDGE('',*,*,#9560,.T.);
#12612=ORIENTED_EDGE('',*,*,#9557,.T.);
#12613=ORIENTED_EDGE('',*,*,#9554,.T.);
#12614=ORIENTED_EDGE('',*,*,#9551,.T.);
#12615=ORIENTED_EDGE('',*,*,#9559,.F.);
#12616=ORIENTED_EDGE('',*,*,#9549,.F.);
#12617=ORIENTED_EDGE('',*,*,#9553,.F.);
#12618=ORIENTED_EDGE('',*,*,#9556,.F.);
#12619=ORIENTED_EDGE('',*,*,#9561,.T.);
#12620=ORIENTED_EDGE('',*,*,#9562,.T.);
#12621=ORIENTED_EDGE('',*,*,#9563,.F.);
#12622=ORIENTED_EDGE('',*,*,#9564,.F.);
#12623=ORIENTED_EDGE('',*,*,#9565,.T.);
#12624=ORIENTED_EDGE('',*,*,#9564,.T.);
#12625=ORIENTED_EDGE('',*,*,#9566,.F.);
#12626=ORIENTED_EDGE('',*,*,#9567,.F.);
#12627=ORIENTED_EDGE('',*,*,#9568,.T.);
#12628=ORIENTED_EDGE('',*,*,#9567,.T.);
#12629=ORIENTED_EDGE('',*,*,#9569,.F.);
#12630=ORIENTED_EDGE('',*,*,#9570,.F.);
#12631=ORIENTED_EDGE('',*,*,#9571,.T.);
#12632=ORIENTED_EDGE('',*,*,#9570,.T.);
#12633=ORIENTED_EDGE('',*,*,#9572,.F.);
#12634=ORIENTED_EDGE('',*,*,#9562,.F.);
#12635=ORIENTED_EDGE('',*,*,#9572,.T.);
#12636=ORIENTED_EDGE('',*,*,#9569,.T.);
#12637=ORIENTED_EDGE('',*,*,#9566,.T.);
#12638=ORIENTED_EDGE('',*,*,#9563,.T.);
#12639=ORIENTED_EDGE('',*,*,#9571,.F.);
#12640=ORIENTED_EDGE('',*,*,#9561,.F.);
#12641=ORIENTED_EDGE('',*,*,#9565,.F.);
#12642=ORIENTED_EDGE('',*,*,#9568,.F.);
#12643=ORIENTED_EDGE('',*,*,#9573,.T.);
#12644=ORIENTED_EDGE('',*,*,#9574,.T.);
#12645=ORIENTED_EDGE('',*,*,#9575,.T.);
#12646=ORIENTED_EDGE('',*,*,#9576,.F.);
#12647=ORIENTED_EDGE('',*,*,#9577,.T.);
#12648=ORIENTED_EDGE('',*,*,#9578,.T.);
#12649=ORIENTED_EDGE('',*,*,#9579,.T.);
#12650=ORIENTED_EDGE('',*,*,#9574,.F.);
#12651=ORIENTED_EDGE('',*,*,#9580,.T.);
#12652=ORIENTED_EDGE('',*,*,#9581,.T.);
#12653=ORIENTED_EDGE('',*,*,#9582,.T.);
#12654=ORIENTED_EDGE('',*,*,#9578,.F.);
#12655=ORIENTED_EDGE('',*,*,#9583,.T.);
#12656=ORIENTED_EDGE('',*,*,#9584,.T.);
#12657=ORIENTED_EDGE('',*,*,#9585,.T.);
#12658=ORIENTED_EDGE('',*,*,#9581,.F.);
#12659=ORIENTED_EDGE('',*,*,#9586,.T.);
#12660=ORIENTED_EDGE('',*,*,#9587,.T.);
#12661=ORIENTED_EDGE('',*,*,#9588,.T.);
#12662=ORIENTED_EDGE('',*,*,#9584,.F.);
#12663=ORIENTED_EDGE('',*,*,#9589,.T.);
#12664=ORIENTED_EDGE('',*,*,#9576,.T.);
#12665=ORIENTED_EDGE('',*,*,#9590,.T.);
#12666=ORIENTED_EDGE('',*,*,#9587,.F.);
#12667=ORIENTED_EDGE('',*,*,#9589,.F.);
#12668=ORIENTED_EDGE('',*,*,#9586,.F.);
#12669=ORIENTED_EDGE('',*,*,#9583,.F.);
#12670=ORIENTED_EDGE('',*,*,#9580,.F.);
#12671=ORIENTED_EDGE('',*,*,#9577,.F.);
#12672=ORIENTED_EDGE('',*,*,#9573,.F.);
#12673=ORIENTED_EDGE('',*,*,#9590,.F.);
#12674=ORIENTED_EDGE('',*,*,#9575,.F.);
#12675=ORIENTED_EDGE('',*,*,#9579,.F.);
#12676=ORIENTED_EDGE('',*,*,#9582,.F.);
#12677=ORIENTED_EDGE('',*,*,#9585,.F.);
#12678=ORIENTED_EDGE('',*,*,#9588,.F.);
#12679=ORIENTED_EDGE('',*,*,#9591,.T.);
#12680=ORIENTED_EDGE('',*,*,#9592,.F.);
#12681=ORIENTED_EDGE('',*,*,#9591,.F.);
#12682=ORIENTED_EDGE('',*,*,#9593,.T.);
#12683=ORIENTED_EDGE('',*,*,#9594,.T.);
#12684=ORIENTED_EDGE('',*,*,#9593,.F.);
#12685=ORIENTED_EDGE('',*,*,#9594,.F.);
#12686=ORIENTED_EDGE('',*,*,#9595,.F.);
#12687=ORIENTED_EDGE('',*,*,#9596,.F.);
#12688=ORIENTED_EDGE('',*,*,#9597,.T.);
#12689=ORIENTED_EDGE('',*,*,#9595,.T.);
#12690=ORIENTED_EDGE('',*,*,#9597,.F.);
#12691=ORIENTED_EDGE('',*,*,#9598,.F.);
#12692=ORIENTED_EDGE('',*,*,#9599,.T.);
#12693=ORIENTED_EDGE('',*,*,#9596,.T.);
#12694=ORIENTED_EDGE('',*,*,#9599,.F.);
#12695=ORIENTED_EDGE('',*,*,#9600,.F.);
#12696=ORIENTED_EDGE('',*,*,#9601,.T.);
#12697=ORIENTED_EDGE('',*,*,#9598,.T.);
#12698=ORIENTED_EDGE('',*,*,#9601,.F.);
#12699=ORIENTED_EDGE('',*,*,#9600,.T.);
#12700=ORIENTED_EDGE('',*,*,#9602,.F.);
#12701=ORIENTED_EDGE('',*,*,#9603,.F.);
#12702=ORIENTED_EDGE('',*,*,#9604,.T.);
#12703=ORIENTED_EDGE('',*,*,#9602,.T.);
#12704=ORIENTED_EDGE('',*,*,#9604,.F.);
#12705=ORIENTED_EDGE('',*,*,#9592,.T.);
#12706=ORIENTED_EDGE('',*,*,#9605,.T.);
#12707=ORIENTED_EDGE('',*,*,#9603,.T.);
#12708=ORIENTED_EDGE('',*,*,#9605,.F.);
#12709=ORIENTED_EDGE('',*,*,#9606,.F.);
#12710=ORIENTED_EDGE('',*,*,#9607,.T.);
#12711=ORIENTED_EDGE('',*,*,#9608,.F.);
#12712=ORIENTED_EDGE('',*,*,#9607,.F.);
#12713=ORIENTED_EDGE('',*,*,#9606,.T.);
#12714=ORIENTED_EDGE('',*,*,#9609,.F.);
#12715=ORIENTED_EDGE('',*,*,#9610,.T.);
#12716=ORIENTED_EDGE('',*,*,#9611,.F.);
#12717=ORIENTED_EDGE('',*,*,#9612,.T.);
#12718=ORIENTED_EDGE('',*,*,#9613,.F.);
#12719=ORIENTED_EDGE('',*,*,#9612,.F.);
#12720=ORIENTED_EDGE('',*,*,#9614,.F.);
#12721=ORIENTED_EDGE('',*,*,#9615,.F.);
#12722=ORIENTED_EDGE('',*,*,#9616,.F.);
#12723=ORIENTED_EDGE('',*,*,#9615,.T.);
#12724=ORIENTED_EDGE('',*,*,#9617,.T.);
#12725=ORIENTED_EDGE('',*,*,#9618,.T.);
#12726=ORIENTED_EDGE('',*,*,#9614,.T.);
#12727=ORIENTED_EDGE('',*,*,#9611,.T.);
#12728=ORIENTED_EDGE('',*,*,#9619,.T.);
#12729=ORIENTED_EDGE('',*,*,#9617,.F.);
#12730=ORIENTED_EDGE('',*,*,#9620,.F.);
#12731=ORIENTED_EDGE('',*,*,#9618,.F.);
#12732=ORIENTED_EDGE('',*,*,#9619,.F.);
#12733=ORIENTED_EDGE('',*,*,#9610,.F.);
#12734=ORIENTED_EDGE('',*,*,#9621,.F.);
#12735=ORIENTED_EDGE('',*,*,#9622,.T.);
#12736=ORIENTED_EDGE('',*,*,#9623,.F.);
#12737=ORIENTED_EDGE('',*,*,#9624,.T.);
#12738=ORIENTED_EDGE('',*,*,#9625,.F.);
#12739=ORIENTED_EDGE('',*,*,#9624,.F.);
#12740=ORIENTED_EDGE('',*,*,#9626,.F.);
#12741=ORIENTED_EDGE('',*,*,#9627,.F.);
#12742=ORIENTED_EDGE('',*,*,#9628,.F.);
#12743=ORIENTED_EDGE('',*,*,#9627,.T.);
#12744=ORIENTED_EDGE('',*,*,#9629,.T.);
#12745=ORIENTED_EDGE('',*,*,#9630,.T.);
#12746=ORIENTED_EDGE('',*,*,#9626,.T.);
#12747=ORIENTED_EDGE('',*,*,#9623,.T.);
#12748=ORIENTED_EDGE('',*,*,#9631,.T.);
#12749=ORIENTED_EDGE('',*,*,#9629,.F.);
#12750=ORIENTED_EDGE('',*,*,#9632,.F.);
#12751=ORIENTED_EDGE('',*,*,#9630,.F.);
#12752=ORIENTED_EDGE('',*,*,#9631,.F.);
#12753=ORIENTED_EDGE('',*,*,#9622,.F.);
#12754=ORIENTED_EDGE('',*,*,#9633,.T.);
#12755=ORIENTED_EDGE('',*,*,#9634,.F.);
#12756=ORIENTED_EDGE('',*,*,#9635,.F.);
#12757=ORIENTED_EDGE('',*,*,#9636,.F.);
#12758=ORIENTED_EDGE('',*,*,#9633,.F.);
#12759=ORIENTED_EDGE('',*,*,#9637,.T.);
#12760=ORIENTED_EDGE('',*,*,#9635,.T.);
#12761=ORIENTED_EDGE('',*,*,#9637,.F.);
#12762=ORIENTED_EDGE('',*,*,#9636,.T.);
#12763=ORIENTED_EDGE('',*,*,#9638,.T.);
#12764=ORIENTED_EDGE('',*,*,#9639,.T.);
#12765=ORIENTED_EDGE('',*,*,#9638,.F.);
#12766=ORIENTED_EDGE('',*,*,#9640,.F.);
#12767=ORIENTED_EDGE('',*,*,#9641,.T.);
#12768=ORIENTED_EDGE('',*,*,#9634,.T.);
#12769=ORIENTED_EDGE('',*,*,#9641,.F.);
#12770=ORIENTED_EDGE('',*,*,#9616,.T.);
#12771=ORIENTED_EDGE('',*,*,#9620,.T.);
#12772=ORIENTED_EDGE('',*,*,#9609,.T.);
#12773=ORIENTED_EDGE('',*,*,#9613,.T.);
#12774=ORIENTED_EDGE('',*,*,#9628,.T.);
#12775=ORIENTED_EDGE('',*,*,#9632,.T.);
#12776=ORIENTED_EDGE('',*,*,#9621,.T.);
#12777=ORIENTED_EDGE('',*,*,#9625,.T.);
#12778=ORIENTED_EDGE('',*,*,#9640,.T.);
#12779=ORIENTED_EDGE('',*,*,#9608,.T.);
#12780=ORIENTED_EDGE('',*,*,#9639,.F.);
#12781=ORIENTED_EDGE('',*,*,#9642,.F.);
#12782=ORIENTED_EDGE('',*,*,#9643,.T.);
#12783=ORIENTED_EDGE('',*,*,#9644,.T.);
#12784=ORIENTED_EDGE('',*,*,#9643,.F.);
#12785=ORIENTED_EDGE('',*,*,#9645,.F.);
#12786=ORIENTED_EDGE('',*,*,#9646,.T.);
#12787=ORIENTED_EDGE('',*,*,#9647,.T.);
#12788=ORIENTED_EDGE('',*,*,#9646,.F.);
#12789=ORIENTED_EDGE('',*,*,#9645,.T.);
#12790=ORIENTED_EDGE('',*,*,#9642,.T.);
#12791=ORIENTED_EDGE('',*,*,#9647,.F.);
#12792=ORIENTED_EDGE('',*,*,#9644,.F.);
#12793=ORIENTED_EDGE('',*,*,#9648,.F.);
#12794=ORIENTED_EDGE('',*,*,#9649,.T.);
#12795=ORIENTED_EDGE('',*,*,#9650,.T.);
#12796=ORIENTED_EDGE('',*,*,#9649,.F.);
#12797=ORIENTED_EDGE('',*,*,#9651,.F.);
#12798=ORIENTED_EDGE('',*,*,#9652,.T.);
#12799=ORIENTED_EDGE('',*,*,#9653,.T.);
#12800=ORIENTED_EDGE('',*,*,#9652,.F.);
#12801=ORIENTED_EDGE('',*,*,#9651,.T.);
#12802=ORIENTED_EDGE('',*,*,#9648,.T.);
#12803=ORIENTED_EDGE('',*,*,#9653,.F.);
#12804=ORIENTED_EDGE('',*,*,#9650,.F.);
#12805=ORIENTED_EDGE('',*,*,#9654,.F.);
#12806=ORIENTED_EDGE('',*,*,#9655,.T.);
#12807=ORIENTED_EDGE('',*,*,#9656,.F.);
#12808=ORIENTED_EDGE('',*,*,#9657,.F.);
#12809=ORIENTED_EDGE('',*,*,#9658,.T.);
#12810=ORIENTED_EDGE('',*,*,#9659,.F.);
#12811=ORIENTED_EDGE('',*,*,#9660,.F.);
#12812=ORIENTED_EDGE('',*,*,#9658,.F.);
#12813=ORIENTED_EDGE('',*,*,#9661,.F.);
#12814=ORIENTED_EDGE('',*,*,#9662,.F.);
#12815=ORIENTED_EDGE('',*,*,#9655,.F.);
#12816=ORIENTED_EDGE('',*,*,#9663,.F.);
#12817=ORIENTED_EDGE('',*,*,#9661,.T.);
#12818=ORIENTED_EDGE('',*,*,#9657,.T.);
#12819=ORIENTED_EDGE('',*,*,#9664,.F.);
#12820=ORIENTED_EDGE('',*,*,#9665,.T.);
#12821=ORIENTED_EDGE('',*,*,#9666,.T.);
#12822=ORIENTED_EDGE('',*,*,#9665,.F.);
#12823=ORIENTED_EDGE('',*,*,#9662,.T.);
#12824=ORIENTED_EDGE('',*,*,#9663,.T.);
#12825=ORIENTED_EDGE('',*,*,#9656,.T.);
#12826=ORIENTED_EDGE('',*,*,#9654,.T.);
#12827=ORIENTED_EDGE('',*,*,#9667,.F.);
#12828=ORIENTED_EDGE('',*,*,#9668,.T.);
#12829=ORIENTED_EDGE('',*,*,#9669,.T.);
#12830=ORIENTED_EDGE('',*,*,#9668,.F.);
#12831=ORIENTED_EDGE('',*,*,#9659,.T.);
#12832=ORIENTED_EDGE('',*,*,#9660,.T.);
#12833=ORIENTED_EDGE('',*,*,#9667,.T.);
#12834=ORIENTED_EDGE('',*,*,#9664,.T.);
#12835=ORIENTED_EDGE('',*,*,#9669,.F.);
#12836=ORIENTED_EDGE('',*,*,#9666,.F.);
#12837=ORIENTED_EDGE('',*,*,#9670,.F.);
#12838=ORIENTED_EDGE('',*,*,#9671,.T.);
#12839=ORIENTED_EDGE('',*,*,#9672,.F.);
#12840=ORIENTED_EDGE('',*,*,#9671,.F.);
#12841=ORIENTED_EDGE('',*,*,#9673,.F.);
#12842=ORIENTED_EDGE('',*,*,#9674,.T.);
#12843=ORIENTED_EDGE('',*,*,#9675,.F.);
#12844=ORIENTED_EDGE('',*,*,#9676,.F.);
#12845=ORIENTED_EDGE('',*,*,#9677,.F.);
#12846=ORIENTED_EDGE('',*,*,#9678,.T.);
#12847=ORIENTED_EDGE('',*,*,#9679,.F.);
#12848=ORIENTED_EDGE('',*,*,#9674,.F.);
#12849=ORIENTED_EDGE('',*,*,#9680,.F.);
#12850=ORIENTED_EDGE('',*,*,#9681,.F.);
#12851=ORIENTED_EDGE('',*,*,#9682,.F.);
#12852=ORIENTED_EDGE('',*,*,#9678,.F.);
#12853=ORIENTED_EDGE('',*,*,#9683,.T.);
#12854=ORIENTED_EDGE('',*,*,#9675,.T.);
#12855=ORIENTED_EDGE('',*,*,#9679,.T.);
#12856=ORIENTED_EDGE('',*,*,#9682,.T.);
#12857=ORIENTED_EDGE('',*,*,#9684,.T.);
#12858=ORIENTED_EDGE('',*,*,#9676,.T.);
#12859=ORIENTED_EDGE('',*,*,#9684,.F.);
#12860=ORIENTED_EDGE('',*,*,#9681,.T.);
#12861=ORIENTED_EDGE('',*,*,#9685,.T.);
#12862=ORIENTED_EDGE('',*,*,#9686,.F.);
#12863=ORIENTED_EDGE('',*,*,#9687,.F.);
#12864=ORIENTED_EDGE('',*,*,#9688,.F.);
#12865=ORIENTED_EDGE('',*,*,#9689,.T.);
#12866=ORIENTED_EDGE('',*,*,#9689,.F.);
#12867=ORIENTED_EDGE('',*,*,#9690,.T.);
#12868=ORIENTED_EDGE('',*,*,#9691,.F.);
#12869=ORIENTED_EDGE('',*,*,#9692,.T.);
#12870=ORIENTED_EDGE('',*,*,#9670,.T.);
#12871=ORIENTED_EDGE('',*,*,#9688,.T.);
#12872=ORIENTED_EDGE('',*,*,#9693,.F.);
#12873=ORIENTED_EDGE('',*,*,#9694,.F.);
#12874=ORIENTED_EDGE('',*,*,#9690,.F.);
#12875=ORIENTED_EDGE('',*,*,#9695,.T.);
#12876=ORIENTED_EDGE('',*,*,#9696,.F.);
#12877=ORIENTED_EDGE('',*,*,#9693,.T.);
#12878=ORIENTED_EDGE('',*,*,#9687,.T.);
#12879=ORIENTED_EDGE('',*,*,#9672,.T.);
#12880=ORIENTED_EDGE('',*,*,#9686,.T.);
#12881=ORIENTED_EDGE('',*,*,#9692,.F.);
#12882=ORIENTED_EDGE('',*,*,#9697,.F.);
#12883=ORIENTED_EDGE('',*,*,#9695,.F.);
#12884=ORIENTED_EDGE('',*,*,#9683,.F.);
#12885=ORIENTED_EDGE('',*,*,#9698,.T.);
#12886=ORIENTED_EDGE('',*,*,#9699,.T.);
#12887=ORIENTED_EDGE('',*,*,#9698,.F.);
#12888=ORIENTED_EDGE('',*,*,#9697,.T.);
#12889=ORIENTED_EDGE('',*,*,#9691,.T.);
#12890=ORIENTED_EDGE('',*,*,#9694,.T.);
#12891=ORIENTED_EDGE('',*,*,#9696,.T.);
#12892=ORIENTED_EDGE('',*,*,#9699,.F.);
#12893=ORIENTED_EDGE('',*,*,#9673,.T.);
#12894=ORIENTED_EDGE('',*,*,#9685,.F.);
#12895=ORIENTED_EDGE('',*,*,#9680,.T.);
#12896=ORIENTED_EDGE('',*,*,#9677,.T.);
#12897=ORIENTED_EDGE('',*,*,#9700,.F.);
#12898=ORIENTED_EDGE('',*,*,#9701,.T.);
#12899=ORIENTED_EDGE('',*,*,#9702,.T.);
#12900=ORIENTED_EDGE('',*,*,#9701,.F.);
#12901=ORIENTED_EDGE('',*,*,#9703,.F.);
#12902=ORIENTED_EDGE('',*,*,#9704,.T.);
#12903=ORIENTED_EDGE('',*,*,#9705,.T.);
#12904=ORIENTED_EDGE('',*,*,#9704,.F.);
#12905=ORIENTED_EDGE('',*,*,#9703,.T.);
#12906=ORIENTED_EDGE('',*,*,#9700,.T.);
#12907=ORIENTED_EDGE('',*,*,#9705,.F.);
#12908=ORIENTED_EDGE('',*,*,#9702,.F.);
#12909=ORIENTED_EDGE('',*,*,#9706,.F.);
#12910=ORIENTED_EDGE('',*,*,#9707,.T.);
#12911=ORIENTED_EDGE('',*,*,#9708,.T.);
#12912=ORIENTED_EDGE('',*,*,#9707,.F.);
#12913=ORIENTED_EDGE('',*,*,#9709,.F.);
#12914=ORIENTED_EDGE('',*,*,#9710,.T.);
#12915=ORIENTED_EDGE('',*,*,#9711,.T.);
#12916=ORIENTED_EDGE('',*,*,#9710,.F.);
#12917=ORIENTED_EDGE('',*,*,#9709,.T.);
#12918=ORIENTED_EDGE('',*,*,#9706,.T.);
#12919=ORIENTED_EDGE('',*,*,#9711,.F.);
#12920=ORIENTED_EDGE('',*,*,#9708,.F.);
#12921=ORIENTED_EDGE('',*,*,#9712,.F.);
#12922=ORIENTED_EDGE('',*,*,#9713,.T.);
#12923=ORIENTED_EDGE('',*,*,#9714,.T.);
#12924=ORIENTED_EDGE('',*,*,#9713,.F.);
#12925=ORIENTED_EDGE('',*,*,#9715,.F.);
#12926=ORIENTED_EDGE('',*,*,#9716,.T.);
#12927=ORIENTED_EDGE('',*,*,#9717,.T.);
#12928=ORIENTED_EDGE('',*,*,#9716,.F.);
#12929=ORIENTED_EDGE('',*,*,#9715,.T.);
#12930=ORIENTED_EDGE('',*,*,#9712,.T.);
#12931=ORIENTED_EDGE('',*,*,#9717,.F.);
#12932=ORIENTED_EDGE('',*,*,#9714,.F.);
#12933=ORIENTED_EDGE('',*,*,#9718,.F.);
#12934=ORIENTED_EDGE('',*,*,#9719,.T.);
#12935=ORIENTED_EDGE('',*,*,#9720,.T.);
#12936=ORIENTED_EDGE('',*,*,#9719,.F.);
#12937=ORIENTED_EDGE('',*,*,#9721,.F.);
#12938=ORIENTED_EDGE('',*,*,#9722,.T.);
#12939=ORIENTED_EDGE('',*,*,#9723,.T.);
#12940=ORIENTED_EDGE('',*,*,#9722,.F.);
#12941=ORIENTED_EDGE('',*,*,#9721,.T.);
#12942=ORIENTED_EDGE('',*,*,#9718,.T.);
#12943=ORIENTED_EDGE('',*,*,#9723,.F.);
#12944=ORIENTED_EDGE('',*,*,#9720,.F.);
#12945=ORIENTED_EDGE('',*,*,#9724,.F.);
#12946=ORIENTED_EDGE('',*,*,#9725,.T.);
#12947=ORIENTED_EDGE('',*,*,#9726,.T.);
#12948=ORIENTED_EDGE('',*,*,#9725,.F.);
#12949=ORIENTED_EDGE('',*,*,#9727,.F.);
#12950=ORIENTED_EDGE('',*,*,#9728,.T.);
#12951=ORIENTED_EDGE('',*,*,#9729,.T.);
#12952=ORIENTED_EDGE('',*,*,#9728,.F.);
#12953=ORIENTED_EDGE('',*,*,#9727,.T.);
#12954=ORIENTED_EDGE('',*,*,#9724,.T.);
#12955=ORIENTED_EDGE('',*,*,#9729,.F.);
#12956=ORIENTED_EDGE('',*,*,#9726,.F.);
#12957=ORIENTED_EDGE('',*,*,#9730,.T.);
#12958=ORIENTED_EDGE('',*,*,#9731,.T.);
#12959=ORIENTED_EDGE('',*,*,#9732,.T.);
#12960=ORIENTED_EDGE('',*,*,#9733,.F.);
#12961=ORIENTED_EDGE('',*,*,#9734,.T.);
#12962=ORIENTED_EDGE('',*,*,#9735,.T.);
#12963=ORIENTED_EDGE('',*,*,#9736,.T.);
#12964=ORIENTED_EDGE('',*,*,#9731,.F.);
#12965=ORIENTED_EDGE('',*,*,#9737,.T.);
#12966=ORIENTED_EDGE('',*,*,#9738,.T.);
#12967=ORIENTED_EDGE('',*,*,#9739,.T.);
#12968=ORIENTED_EDGE('',*,*,#9735,.F.);
#12969=ORIENTED_EDGE('',*,*,#9740,.T.);
#12970=ORIENTED_EDGE('',*,*,#9741,.T.);
#12971=ORIENTED_EDGE('',*,*,#9742,.T.);
#12972=ORIENTED_EDGE('',*,*,#9738,.F.);
#12973=ORIENTED_EDGE('',*,*,#9743,.T.);
#12974=ORIENTED_EDGE('',*,*,#9744,.T.);
#12975=ORIENTED_EDGE('',*,*,#9745,.T.);
#12976=ORIENTED_EDGE('',*,*,#9741,.F.);
#12977=ORIENTED_EDGE('',*,*,#9746,.T.);
#12978=ORIENTED_EDGE('',*,*,#9733,.T.);
#12979=ORIENTED_EDGE('',*,*,#9747,.T.);
#12980=ORIENTED_EDGE('',*,*,#9744,.F.);
#12981=ORIENTED_EDGE('',*,*,#9746,.F.);
#12982=ORIENTED_EDGE('',*,*,#9743,.F.);
#12983=ORIENTED_EDGE('',*,*,#9740,.F.);
#12984=ORIENTED_EDGE('',*,*,#9737,.F.);
#12985=ORIENTED_EDGE('',*,*,#9734,.F.);
#12986=ORIENTED_EDGE('',*,*,#9730,.F.);
#12987=ORIENTED_EDGE('',*,*,#9747,.F.);
#12988=ORIENTED_EDGE('',*,*,#9732,.F.);
#12989=ORIENTED_EDGE('',*,*,#9736,.F.);
#12990=ORIENTED_EDGE('',*,*,#9739,.F.);
#12991=ORIENTED_EDGE('',*,*,#9742,.F.);
#12992=ORIENTED_EDGE('',*,*,#9745,.F.);
#12993=ORIENTED_EDGE('',*,*,#9748,.T.);
#12994=ORIENTED_EDGE('',*,*,#9749,.F.);
#12995=ORIENTED_EDGE('',*,*,#9748,.F.);
#12996=ORIENTED_EDGE('',*,*,#9750,.T.);
#12997=ORIENTED_EDGE('',*,*,#9751,.T.);
#12998=ORIENTED_EDGE('',*,*,#9750,.F.);
#12999=ORIENTED_EDGE('',*,*,#9751,.F.);
#13000=ORIENTED_EDGE('',*,*,#9752,.F.);
#13001=ORIENTED_EDGE('',*,*,#9753,.F.);
#13002=ORIENTED_EDGE('',*,*,#9754,.T.);
#13003=ORIENTED_EDGE('',*,*,#9752,.T.);
#13004=ORIENTED_EDGE('',*,*,#9754,.F.);
#13005=ORIENTED_EDGE('',*,*,#9755,.F.);
#13006=ORIENTED_EDGE('',*,*,#9756,.T.);
#13007=ORIENTED_EDGE('',*,*,#9753,.T.);
#13008=ORIENTED_EDGE('',*,*,#9756,.F.);
#13009=ORIENTED_EDGE('',*,*,#9757,.F.);
#13010=ORIENTED_EDGE('',*,*,#9758,.T.);
#13011=ORIENTED_EDGE('',*,*,#9755,.T.);
#13012=ORIENTED_EDGE('',*,*,#9758,.F.);
#13013=ORIENTED_EDGE('',*,*,#9757,.T.);
#13014=ORIENTED_EDGE('',*,*,#9759,.F.);
#13015=ORIENTED_EDGE('',*,*,#9760,.F.);
#13016=ORIENTED_EDGE('',*,*,#9761,.T.);
#13017=ORIENTED_EDGE('',*,*,#9759,.T.);
#13018=ORIENTED_EDGE('',*,*,#9761,.F.);
#13019=ORIENTED_EDGE('',*,*,#9749,.T.);
#13020=ORIENTED_EDGE('',*,*,#9762,.T.);
#13021=ORIENTED_EDGE('',*,*,#9760,.T.);
#13022=ORIENTED_EDGE('',*,*,#9762,.F.);
#13023=ORIENTED_EDGE('',*,*,#9763,.F.);
#13024=ORIENTED_EDGE('',*,*,#9764,.T.);
#13025=ORIENTED_EDGE('',*,*,#9765,.F.);
#13026=ORIENTED_EDGE('',*,*,#9764,.F.);
#13027=ORIENTED_EDGE('',*,*,#9763,.T.);
#13028=ORIENTED_EDGE('',*,*,#9766,.F.);
#13029=ORIENTED_EDGE('',*,*,#9767,.T.);
#13030=ORIENTED_EDGE('',*,*,#9768,.F.);
#13031=ORIENTED_EDGE('',*,*,#9769,.T.);
#13032=ORIENTED_EDGE('',*,*,#9770,.F.);
#13033=ORIENTED_EDGE('',*,*,#9769,.F.);
#13034=ORIENTED_EDGE('',*,*,#9771,.F.);
#13035=ORIENTED_EDGE('',*,*,#9772,.F.);
#13036=ORIENTED_EDGE('',*,*,#9773,.F.);
#13037=ORIENTED_EDGE('',*,*,#9772,.T.);
#13038=ORIENTED_EDGE('',*,*,#9774,.T.);
#13039=ORIENTED_EDGE('',*,*,#9775,.T.);
#13040=ORIENTED_EDGE('',*,*,#9771,.T.);
#13041=ORIENTED_EDGE('',*,*,#9768,.T.);
#13042=ORIENTED_EDGE('',*,*,#9776,.T.);
#13043=ORIENTED_EDGE('',*,*,#9774,.F.);
#13044=ORIENTED_EDGE('',*,*,#9777,.F.);
#13045=ORIENTED_EDGE('',*,*,#9775,.F.);
#13046=ORIENTED_EDGE('',*,*,#9776,.F.);
#13047=ORIENTED_EDGE('',*,*,#9767,.F.);
#13048=ORIENTED_EDGE('',*,*,#9778,.T.);
#13049=ORIENTED_EDGE('',*,*,#9779,.F.);
#13050=ORIENTED_EDGE('',*,*,#9780,.F.);
#13051=ORIENTED_EDGE('',*,*,#9781,.F.);
#13052=ORIENTED_EDGE('',*,*,#9778,.F.);
#13053=ORIENTED_EDGE('',*,*,#9782,.T.);
#13054=ORIENTED_EDGE('',*,*,#9780,.T.);
#13055=ORIENTED_EDGE('',*,*,#9782,.F.);
#13056=ORIENTED_EDGE('',*,*,#9781,.T.);
#13057=ORIENTED_EDGE('',*,*,#9783,.T.);
#13058=ORIENTED_EDGE('',*,*,#9784,.T.);
#13059=ORIENTED_EDGE('',*,*,#9783,.F.);
#13060=ORIENTED_EDGE('',*,*,#9785,.F.);
#13061=ORIENTED_EDGE('',*,*,#9786,.T.);
#13062=ORIENTED_EDGE('',*,*,#9779,.T.);
#13063=ORIENTED_EDGE('',*,*,#9786,.F.);
#13064=ORIENTED_EDGE('',*,*,#9773,.T.);
#13065=ORIENTED_EDGE('',*,*,#9777,.T.);
#13066=ORIENTED_EDGE('',*,*,#9766,.T.);
#13067=ORIENTED_EDGE('',*,*,#9770,.T.);
#13068=ORIENTED_EDGE('',*,*,#9785,.T.);
#13069=ORIENTED_EDGE('',*,*,#9765,.T.);
#13070=ORIENTED_EDGE('',*,*,#9784,.F.);
#13071=ORIENTED_EDGE('',*,*,#9787,.F.);
#13072=ORIENTED_EDGE('',*,*,#9788,.T.);
#13073=ORIENTED_EDGE('',*,*,#9789,.T.);
#13074=ORIENTED_EDGE('',*,*,#9788,.F.);
#13075=ORIENTED_EDGE('',*,*,#9790,.F.);
#13076=ORIENTED_EDGE('',*,*,#9791,.T.);
#13077=ORIENTED_EDGE('',*,*,#9792,.T.);
#13078=ORIENTED_EDGE('',*,*,#9791,.F.);
#13079=ORIENTED_EDGE('',*,*,#9790,.T.);
#13080=ORIENTED_EDGE('',*,*,#9787,.T.);
#13081=ORIENTED_EDGE('',*,*,#9792,.F.);
#13082=ORIENTED_EDGE('',*,*,#9789,.F.);
#13083=ORIENTED_EDGE('',*,*,#9793,.F.);
#13084=ORIENTED_EDGE('',*,*,#9794,.T.);
#13085=ORIENTED_EDGE('',*,*,#9795,.T.);
#13086=ORIENTED_EDGE('',*,*,#9794,.F.);
#13087=ORIENTED_EDGE('',*,*,#9796,.F.);
#13088=ORIENTED_EDGE('',*,*,#9797,.T.);
#13089=ORIENTED_EDGE('',*,*,#9798,.T.);
#13090=ORIENTED_EDGE('',*,*,#9797,.F.);
#13091=ORIENTED_EDGE('',*,*,#9796,.T.);
#13092=ORIENTED_EDGE('',*,*,#9793,.T.);
#13093=ORIENTED_EDGE('',*,*,#9798,.F.);
#13094=ORIENTED_EDGE('',*,*,#9795,.F.);
#13095=ORIENTED_EDGE('',*,*,#9799,.F.);
#13096=ORIENTED_EDGE('',*,*,#9800,.T.);
#13097=ORIENTED_EDGE('',*,*,#9801,.F.);
#13098=ORIENTED_EDGE('',*,*,#9802,.F.);
#13099=ORIENTED_EDGE('',*,*,#9803,.T.);
#13100=ORIENTED_EDGE('',*,*,#9804,.F.);
#13101=ORIENTED_EDGE('',*,*,#9805,.F.);
#13102=ORIENTED_EDGE('',*,*,#9803,.F.);
#13103=ORIENTED_EDGE('',*,*,#9806,.F.);
#13104=ORIENTED_EDGE('',*,*,#9807,.F.);
#13105=ORIENTED_EDGE('',*,*,#9800,.F.);
#13106=ORIENTED_EDGE('',*,*,#9808,.F.);
#13107=ORIENTED_EDGE('',*,*,#9806,.T.);
#13108=ORIENTED_EDGE('',*,*,#9802,.T.);
#13109=ORIENTED_EDGE('',*,*,#9809,.F.);
#13110=ORIENTED_EDGE('',*,*,#9810,.T.);
#13111=ORIENTED_EDGE('',*,*,#9811,.T.);
#13112=ORIENTED_EDGE('',*,*,#9810,.F.);
#13113=ORIENTED_EDGE('',*,*,#9807,.T.);
#13114=ORIENTED_EDGE('',*,*,#9808,.T.);
#13115=ORIENTED_EDGE('',*,*,#9801,.T.);
#13116=ORIENTED_EDGE('',*,*,#9799,.T.);
#13117=ORIENTED_EDGE('',*,*,#9812,.F.);
#13118=ORIENTED_EDGE('',*,*,#9813,.T.);
#13119=ORIENTED_EDGE('',*,*,#9814,.T.);
#13120=ORIENTED_EDGE('',*,*,#9813,.F.);
#13121=ORIENTED_EDGE('',*,*,#9804,.T.);
#13122=ORIENTED_EDGE('',*,*,#9805,.T.);
#13123=ORIENTED_EDGE('',*,*,#9812,.T.);
#13124=ORIENTED_EDGE('',*,*,#9809,.T.);
#13125=ORIENTED_EDGE('',*,*,#9814,.F.);
#13126=ORIENTED_EDGE('',*,*,#9811,.F.);
#13127=ORIENTED_EDGE('',*,*,#9815,.F.);
#13128=ORIENTED_EDGE('',*,*,#9816,.T.);
#13129=ORIENTED_EDGE('',*,*,#9817,.T.);
#13130=ORIENTED_EDGE('',*,*,#9816,.F.);
#13131=ORIENTED_EDGE('',*,*,#9818,.F.);
#13132=ORIENTED_EDGE('',*,*,#9819,.T.);
#13133=ORIENTED_EDGE('',*,*,#9820,.T.);
#13134=ORIENTED_EDGE('',*,*,#9819,.F.);
#13135=ORIENTED_EDGE('',*,*,#9818,.T.);
#13136=ORIENTED_EDGE('',*,*,#9815,.T.);
#13137=ORIENTED_EDGE('',*,*,#9820,.F.);
#13138=ORIENTED_EDGE('',*,*,#9817,.F.);
#13139=ORIENTED_EDGE('',*,*,#9821,.F.);
#13140=ORIENTED_EDGE('',*,*,#9822,.T.);
#13141=ORIENTED_EDGE('',*,*,#9823,.F.);
#13142=ORIENTED_EDGE('',*,*,#9822,.F.);
#13143=ORIENTED_EDGE('',*,*,#9821,.T.);
#13144=ORIENTED_EDGE('',*,*,#9824,.F.);
#13145=ORIENTED_EDGE('',*,*,#9825,.T.);
#13146=ORIENTED_EDGE('',*,*,#9826,.F.);
#13147=ORIENTED_EDGE('',*,*,#9827,.T.);
#13148=ORIENTED_EDGE('',*,*,#9828,.F.);
#13149=ORIENTED_EDGE('',*,*,#9827,.F.);
#13150=ORIENTED_EDGE('',*,*,#9829,.F.);
#13151=ORIENTED_EDGE('',*,*,#9830,.F.);
#13152=ORIENTED_EDGE('',*,*,#9831,.F.);
#13153=ORIENTED_EDGE('',*,*,#9830,.T.);
#13154=ORIENTED_EDGE('',*,*,#9832,.T.);
#13155=ORIENTED_EDGE('',*,*,#9833,.T.);
#13156=ORIENTED_EDGE('',*,*,#9829,.T.);
#13157=ORIENTED_EDGE('',*,*,#9826,.T.);
#13158=ORIENTED_EDGE('',*,*,#9834,.T.);
#13159=ORIENTED_EDGE('',*,*,#9832,.F.);
#13160=ORIENTED_EDGE('',*,*,#9835,.F.);
#13161=ORIENTED_EDGE('',*,*,#9833,.F.);
#13162=ORIENTED_EDGE('',*,*,#9834,.F.);
#13163=ORIENTED_EDGE('',*,*,#9825,.F.);
#13164=ORIENTED_EDGE('',*,*,#9836,.T.);
#13165=ORIENTED_EDGE('',*,*,#9837,.F.);
#13166=ORIENTED_EDGE('',*,*,#9838,.F.);
#13167=ORIENTED_EDGE('',*,*,#9839,.F.);
#13168=ORIENTED_EDGE('',*,*,#9836,.F.);
#13169=ORIENTED_EDGE('',*,*,#9840,.T.);
#13170=ORIENTED_EDGE('',*,*,#9838,.T.);
#13171=ORIENTED_EDGE('',*,*,#9840,.F.);
#13172=ORIENTED_EDGE('',*,*,#9839,.T.);
#13173=ORIENTED_EDGE('',*,*,#9841,.T.);
#13174=ORIENTED_EDGE('',*,*,#9842,.T.);
#13175=ORIENTED_EDGE('',*,*,#9841,.F.);
#13176=ORIENTED_EDGE('',*,*,#9843,.F.);
#13177=ORIENTED_EDGE('',*,*,#9844,.T.);
#13178=ORIENTED_EDGE('',*,*,#9837,.T.);
#13179=ORIENTED_EDGE('',*,*,#9844,.F.);
#13180=ORIENTED_EDGE('',*,*,#9831,.T.);
#13181=ORIENTED_EDGE('',*,*,#9835,.T.);
#13182=ORIENTED_EDGE('',*,*,#9824,.T.);
#13183=ORIENTED_EDGE('',*,*,#9828,.T.);
#13184=ORIENTED_EDGE('',*,*,#9843,.T.);
#13185=ORIENTED_EDGE('',*,*,#9823,.T.);
#13186=ORIENTED_EDGE('',*,*,#9842,.F.);
#13187=ORIENTED_EDGE('',*,*,#9845,.F.);
#13188=ORIENTED_EDGE('',*,*,#9846,.T.);
#13189=ORIENTED_EDGE('',*,*,#9847,.T.);
#13190=ORIENTED_EDGE('',*,*,#9846,.F.);
#13191=ORIENTED_EDGE('',*,*,#9848,.F.);
#13192=ORIENTED_EDGE('',*,*,#9849,.T.);
#13193=ORIENTED_EDGE('',*,*,#9850,.T.);
#13194=ORIENTED_EDGE('',*,*,#9849,.F.);
#13195=ORIENTED_EDGE('',*,*,#9848,.T.);
#13196=ORIENTED_EDGE('',*,*,#9845,.T.);
#13197=ORIENTED_EDGE('',*,*,#9850,.F.);
#13198=ORIENTED_EDGE('',*,*,#9847,.F.);
#13199=ORIENTED_EDGE('',*,*,#9851,.F.);
#13200=ORIENTED_EDGE('',*,*,#9852,.T.);
#13201=ORIENTED_EDGE('',*,*,#9853,.T.);
#13202=ORIENTED_EDGE('',*,*,#9852,.F.);
#13203=ORIENTED_EDGE('',*,*,#9854,.F.);
#13204=ORIENTED_EDGE('',*,*,#9855,.T.);
#13205=ORIENTED_EDGE('',*,*,#9856,.T.);
#13206=ORIENTED_EDGE('',*,*,#9855,.F.);
#13207=ORIENTED_EDGE('',*,*,#9854,.T.);
#13208=ORIENTED_EDGE('',*,*,#9851,.T.);
#13209=ORIENTED_EDGE('',*,*,#9856,.F.);
#13210=ORIENTED_EDGE('',*,*,#9853,.F.);
#13211=ORIENTED_EDGE('',*,*,#9857,.F.);
#13212=ORIENTED_EDGE('',*,*,#9858,.T.);
#13213=ORIENTED_EDGE('',*,*,#9859,.F.);
#13214=ORIENTED_EDGE('',*,*,#9860,.F.);
#13215=ORIENTED_EDGE('',*,*,#9861,.T.);
#13216=ORIENTED_EDGE('',*,*,#9862,.F.);
#13217=ORIENTED_EDGE('',*,*,#9863,.F.);
#13218=ORIENTED_EDGE('',*,*,#9861,.F.);
#13219=ORIENTED_EDGE('',*,*,#9864,.F.);
#13220=ORIENTED_EDGE('',*,*,#9865,.F.);
#13221=ORIENTED_EDGE('',*,*,#9858,.F.);
#13222=ORIENTED_EDGE('',*,*,#9866,.F.);
#13223=ORIENTED_EDGE('',*,*,#9864,.T.);
#13224=ORIENTED_EDGE('',*,*,#9860,.T.);
#13225=ORIENTED_EDGE('',*,*,#9867,.F.);
#13226=ORIENTED_EDGE('',*,*,#9868,.T.);
#13227=ORIENTED_EDGE('',*,*,#9869,.T.);
#13228=ORIENTED_EDGE('',*,*,#9868,.F.);
#13229=ORIENTED_EDGE('',*,*,#9865,.T.);
#13230=ORIENTED_EDGE('',*,*,#9866,.T.);
#13231=ORIENTED_EDGE('',*,*,#9859,.T.);
#13232=ORIENTED_EDGE('',*,*,#9857,.T.);
#13233=ORIENTED_EDGE('',*,*,#9870,.F.);
#13234=ORIENTED_EDGE('',*,*,#9871,.T.);
#13235=ORIENTED_EDGE('',*,*,#9872,.T.);
#13236=ORIENTED_EDGE('',*,*,#9871,.F.);
#13237=ORIENTED_EDGE('',*,*,#9862,.T.);
#13238=ORIENTED_EDGE('',*,*,#9863,.T.);
#13239=ORIENTED_EDGE('',*,*,#9870,.T.);
#13240=ORIENTED_EDGE('',*,*,#9867,.T.);
#13241=ORIENTED_EDGE('',*,*,#9872,.F.);
#13242=ORIENTED_EDGE('',*,*,#9869,.F.);
#13243=ORIENTED_EDGE('',*,*,#9873,.F.);
#13244=ORIENTED_EDGE('',*,*,#9874,.T.);
#13245=ORIENTED_EDGE('',*,*,#9875,.T.);
#13246=ORIENTED_EDGE('',*,*,#9874,.F.);
#13247=ORIENTED_EDGE('',*,*,#9876,.F.);
#13248=ORIENTED_EDGE('',*,*,#9877,.T.);
#13249=ORIENTED_EDGE('',*,*,#9878,.T.);
#13250=ORIENTED_EDGE('',*,*,#9877,.F.);
#13251=ORIENTED_EDGE('',*,*,#9876,.T.);
#13252=ORIENTED_EDGE('',*,*,#9873,.T.);
#13253=ORIENTED_EDGE('',*,*,#9878,.F.);
#13254=ORIENTED_EDGE('',*,*,#9875,.F.);
#13255=ORIENTED_EDGE('',*,*,#9879,.F.);
#13256=ORIENTED_EDGE('',*,*,#9880,.F.);
#13257=ORIENTED_EDGE('',*,*,#9881,.F.);
#13258=ORIENTED_EDGE('',*,*,#9882,.F.);
#13259=ORIENTED_EDGE('',*,*,#9883,.F.);
#13260=ORIENTED_EDGE('',*,*,#9884,.T.);
#13261=ORIENTED_EDGE('',*,*,#9885,.F.);
#13262=ORIENTED_EDGE('',*,*,#9880,.T.);
#13263=ORIENTED_EDGE('',*,*,#9886,.F.);
#13264=ORIENTED_EDGE('',*,*,#9887,.F.);
#13265=ORIENTED_EDGE('',*,*,#9888,.F.);
#13266=ORIENTED_EDGE('',*,*,#9884,.F.);
#13267=ORIENTED_EDGE('',*,*,#9889,.T.);
#13268=ORIENTED_EDGE('',*,*,#9890,.T.);
#13269=ORIENTED_EDGE('',*,*,#9891,.T.);
#13270=ORIENTED_EDGE('',*,*,#9892,.T.);
#13271=ORIENTED_EDGE('',*,*,#9893,.T.);
#13272=ORIENTED_EDGE('',*,*,#9894,.T.);
#13273=ORIENTED_EDGE('',*,*,#9895,.T.);
#13274=ORIENTED_EDGE('',*,*,#9896,.T.);
#13275=ORIENTED_EDGE('',*,*,#9897,.T.);
#13276=ORIENTED_EDGE('',*,*,#9898,.T.);
#13277=ORIENTED_EDGE('',*,*,#9899,.T.);
#13278=ORIENTED_EDGE('',*,*,#9900,.T.);
#13279=ORIENTED_EDGE('',*,*,#9901,.T.);
#13280=ORIENTED_EDGE('',*,*,#9902,.T.);
#13281=ORIENTED_EDGE('',*,*,#9903,.T.);
#13282=ORIENTED_EDGE('',*,*,#9904,.T.);
#13283=ORIENTED_EDGE('',*,*,#9905,.T.);
#13284=ORIENTED_EDGE('',*,*,#9906,.T.);
#13285=ORIENTED_EDGE('',*,*,#9907,.T.);
#13286=ORIENTED_EDGE('',*,*,#9908,.T.);
#13287=ORIENTED_EDGE('',*,*,#9909,.T.);
#13288=ORIENTED_EDGE('',*,*,#9910,.T.);
#13289=ORIENTED_EDGE('',*,*,#9911,.T.);
#13290=ORIENTED_EDGE('',*,*,#9912,.T.);
#13291=ORIENTED_EDGE('',*,*,#9913,.T.);
#13292=ORIENTED_EDGE('',*,*,#9914,.T.);
#13293=ORIENTED_EDGE('',*,*,#9915,.T.);
#13294=ORIENTED_EDGE('',*,*,#9916,.T.);
#13295=ORIENTED_EDGE('',*,*,#9917,.T.);
#13296=ORIENTED_EDGE('',*,*,#9918,.T.);
#13297=ORIENTED_EDGE('',*,*,#9919,.T.);
#13298=ORIENTED_EDGE('',*,*,#9920,.T.);
#13299=ORIENTED_EDGE('',*,*,#9921,.T.);
#13300=ORIENTED_EDGE('',*,*,#9922,.T.);
#13301=ORIENTED_EDGE('',*,*,#9923,.T.);
#13302=ORIENTED_EDGE('',*,*,#9924,.T.);
#13303=ORIENTED_EDGE('',*,*,#9925,.T.);
#13304=ORIENTED_EDGE('',*,*,#9926,.T.);
#13305=ORIENTED_EDGE('',*,*,#9927,.T.);
#13306=ORIENTED_EDGE('',*,*,#9928,.T.);
#13307=ORIENTED_EDGE('',*,*,#9929,.T.);
#13308=ORIENTED_EDGE('',*,*,#9930,.T.);
#13309=ORIENTED_EDGE('',*,*,#9931,.T.);
#13310=ORIENTED_EDGE('',*,*,#9932,.T.);
#13311=ORIENTED_EDGE('',*,*,#9933,.T.);
#13312=ORIENTED_EDGE('',*,*,#9934,.T.);
#13313=ORIENTED_EDGE('',*,*,#9935,.T.);
#13314=ORIENTED_EDGE('',*,*,#9936,.T.);
#13315=ORIENTED_EDGE('',*,*,#9937,.T.);
#13316=ORIENTED_EDGE('',*,*,#9938,.T.);
#13317=ORIENTED_EDGE('',*,*,#9939,.T.);
#13318=ORIENTED_EDGE('',*,*,#9940,.T.);
#13319=ORIENTED_EDGE('',*,*,#9941,.T.);
#13320=ORIENTED_EDGE('',*,*,#9942,.T.);
#13321=ORIENTED_EDGE('',*,*,#9943,.T.);
#13322=ORIENTED_EDGE('',*,*,#9944,.T.);
#13323=ORIENTED_EDGE('',*,*,#9945,.T.);
#13324=ORIENTED_EDGE('',*,*,#9946,.T.);
#13325=ORIENTED_EDGE('',*,*,#9947,.T.);
#13326=ORIENTED_EDGE('',*,*,#9948,.T.);
#13327=ORIENTED_EDGE('',*,*,#9949,.T.);
#13328=ORIENTED_EDGE('',*,*,#9950,.T.);
#13329=ORIENTED_EDGE('',*,*,#9951,.T.);
#13330=ORIENTED_EDGE('',*,*,#9952,.T.);
#13331=ORIENTED_EDGE('',*,*,#9953,.T.);
#13332=ORIENTED_EDGE('',*,*,#9954,.T.);
#13333=ORIENTED_EDGE('',*,*,#9955,.T.);
#13334=ORIENTED_EDGE('',*,*,#9956,.T.);
#13335=ORIENTED_EDGE('',*,*,#9957,.T.);
#13336=ORIENTED_EDGE('',*,*,#9958,.T.);
#13337=ORIENTED_EDGE('',*,*,#9959,.T.);
#13338=ORIENTED_EDGE('',*,*,#9960,.T.);
#13339=ORIENTED_EDGE('',*,*,#9961,.T.);
#13340=ORIENTED_EDGE('',*,*,#9962,.T.);
#13341=ORIENTED_EDGE('',*,*,#9963,.T.);
#13342=ORIENTED_EDGE('',*,*,#9964,.T.);
#13343=ORIENTED_EDGE('',*,*,#9965,.T.);
#13344=ORIENTED_EDGE('',*,*,#9966,.T.);
#13345=ORIENTED_EDGE('',*,*,#9967,.T.);
#13346=ORIENTED_EDGE('',*,*,#9968,.T.);
#13347=ORIENTED_EDGE('',*,*,#9881,.T.);
#13348=ORIENTED_EDGE('',*,*,#9885,.T.);
#13349=ORIENTED_EDGE('',*,*,#9888,.T.);
#13350=ORIENTED_EDGE('',*,*,#9969,.T.);
#13351=ORIENTED_EDGE('',*,*,#9882,.T.);
#13352=ORIENTED_EDGE('',*,*,#9969,.F.);
#13353=ORIENTED_EDGE('',*,*,#9887,.T.);
#13354=ORIENTED_EDGE('',*,*,#9970,.F.);
#13355=ORIENTED_EDGE('',*,*,#9971,.F.);
#13356=ORIENTED_EDGE('',*,*,#9972,.T.);
#13357=ORIENTED_EDGE('',*,*,#9973,.F.);
#13358=ORIENTED_EDGE('',*,*,#9972,.F.);
#13359=ORIENTED_EDGE('',*,*,#9971,.T.);
#13360=ORIENTED_EDGE('',*,*,#9879,.T.);
#13361=ORIENTED_EDGE('',*,*,#9970,.T.);
#13362=ORIENTED_EDGE('',*,*,#9886,.T.);
#13363=ORIENTED_EDGE('',*,*,#9883,.T.);
#13364=ORIENTED_EDGE('',*,*,#9974,.F.);
#13365=ORIENTED_EDGE('',*,*,#9975,.F.);
#13366=ORIENTED_EDGE('',*,*,#9976,.F.);
#13367=ORIENTED_EDGE('',*,*,#9966,.F.);
#13368=ORIENTED_EDGE('',*,*,#9976,.T.);
#13369=ORIENTED_EDGE('',*,*,#9977,.F.);
#13370=ORIENTED_EDGE('',*,*,#9978,.F.);
#13371=ORIENTED_EDGE('',*,*,#9967,.F.);
#13372=ORIENTED_EDGE('',*,*,#9978,.T.);
#13373=ORIENTED_EDGE('',*,*,#9979,.F.);
#13374=ORIENTED_EDGE('',*,*,#9980,.F.);
#13375=ORIENTED_EDGE('',*,*,#9968,.F.);
#13376=ORIENTED_EDGE('',*,*,#9980,.T.);
#13377=ORIENTED_EDGE('',*,*,#9981,.F.);
#13378=ORIENTED_EDGE('',*,*,#9982,.T.);
#13379=ORIENTED_EDGE('',*,*,#9889,.F.);
#13380=ORIENTED_EDGE('',*,*,#9982,.F.);
#13381=ORIENTED_EDGE('',*,*,#9983,.F.);
#13382=ORIENTED_EDGE('',*,*,#9984,.F.);
#13383=ORIENTED_EDGE('',*,*,#9890,.F.);
#13384=ORIENTED_EDGE('',*,*,#9984,.T.);
#13385=ORIENTED_EDGE('',*,*,#9985,.F.);
#13386=ORIENTED_EDGE('',*,*,#9986,.F.);
#13387=ORIENTED_EDGE('',*,*,#9891,.F.);
#13388=ORIENTED_EDGE('',*,*,#9986,.T.);
#13389=ORIENTED_EDGE('',*,*,#9987,.F.);
#13390=ORIENTED_EDGE('',*,*,#9988,.F.);
#13391=ORIENTED_EDGE('',*,*,#9892,.F.);
#13392=ORIENTED_EDGE('',*,*,#9988,.T.);
#13393=ORIENTED_EDGE('',*,*,#9989,.F.);
#13394=ORIENTED_EDGE('',*,*,#9990,.T.);
#13395=ORIENTED_EDGE('',*,*,#9893,.F.);
#13396=ORIENTED_EDGE('',*,*,#9990,.F.);
#13397=ORIENTED_EDGE('',*,*,#9991,.F.);
#13398=ORIENTED_EDGE('',*,*,#9992,.F.);
#13399=ORIENTED_EDGE('',*,*,#9894,.F.);
#13400=ORIENTED_EDGE('',*,*,#9992,.T.);
#13401=ORIENTED_EDGE('',*,*,#9993,.F.);
#13402=ORIENTED_EDGE('',*,*,#9994,.F.);
#13403=ORIENTED_EDGE('',*,*,#9895,.F.);
#13404=ORIENTED_EDGE('',*,*,#9994,.T.);
#13405=ORIENTED_EDGE('',*,*,#9995,.F.);
#13406=ORIENTED_EDGE('',*,*,#9996,.F.);
#13407=ORIENTED_EDGE('',*,*,#9896,.F.);
#13408=ORIENTED_EDGE('',*,*,#9996,.T.);
#13409=ORIENTED_EDGE('',*,*,#9997,.F.);
#13410=ORIENTED_EDGE('',*,*,#9998,.T.);
#13411=ORIENTED_EDGE('',*,*,#9897,.F.);
#13412=ORIENTED_EDGE('',*,*,#9998,.F.);
#13413=ORIENTED_EDGE('',*,*,#9999,.F.);
#13414=ORIENTED_EDGE('',*,*,#10000,.F.);
#13415=ORIENTED_EDGE('',*,*,#9898,.F.);
#13416=ORIENTED_EDGE('',*,*,#10000,.T.);
#13417=ORIENTED_EDGE('',*,*,#10001,.F.);
#13418=ORIENTED_EDGE('',*,*,#10002,.F.);
#13419=ORIENTED_EDGE('',*,*,#9899,.F.);
#13420=ORIENTED_EDGE('',*,*,#10002,.T.);
#13421=ORIENTED_EDGE('',*,*,#10003,.F.);
#13422=ORIENTED_EDGE('',*,*,#10004,.F.);
#13423=ORIENTED_EDGE('',*,*,#9900,.F.);
#13424=ORIENTED_EDGE('',*,*,#10004,.T.);
#13425=ORIENTED_EDGE('',*,*,#10005,.F.);
#13426=ORIENTED_EDGE('',*,*,#10006,.T.);
#13427=ORIENTED_EDGE('',*,*,#9901,.F.);
#13428=ORIENTED_EDGE('',*,*,#10006,.F.);
#13429=ORIENTED_EDGE('',*,*,#10007,.F.);
#13430=ORIENTED_EDGE('',*,*,#10008,.F.);
#13431=ORIENTED_EDGE('',*,*,#9902,.F.);
#13432=ORIENTED_EDGE('',*,*,#10008,.T.);
#13433=ORIENTED_EDGE('',*,*,#10009,.F.);
#13434=ORIENTED_EDGE('',*,*,#10010,.F.);
#13435=ORIENTED_EDGE('',*,*,#9903,.F.);
#13436=ORIENTED_EDGE('',*,*,#10010,.T.);
#13437=ORIENTED_EDGE('',*,*,#10011,.F.);
#13438=ORIENTED_EDGE('',*,*,#10012,.F.);
#13439=ORIENTED_EDGE('',*,*,#9904,.F.);
#13440=ORIENTED_EDGE('',*,*,#10012,.T.);
#13441=ORIENTED_EDGE('',*,*,#10013,.F.);
#13442=ORIENTED_EDGE('',*,*,#10014,.T.);
#13443=ORIENTED_EDGE('',*,*,#9905,.F.);
#13444=ORIENTED_EDGE('',*,*,#10014,.F.);
#13445=ORIENTED_EDGE('',*,*,#10015,.F.);
#13446=ORIENTED_EDGE('',*,*,#10016,.F.);
#13447=ORIENTED_EDGE('',*,*,#9906,.F.);
#13448=ORIENTED_EDGE('',*,*,#10016,.T.);
#13449=ORIENTED_EDGE('',*,*,#10017,.F.);
#13450=ORIENTED_EDGE('',*,*,#10018,.F.);
#13451=ORIENTED_EDGE('',*,*,#9907,.F.);
#13452=ORIENTED_EDGE('',*,*,#10018,.T.);
#13453=ORIENTED_EDGE('',*,*,#10019,.F.);
#13454=ORIENTED_EDGE('',*,*,#10020,.F.);
#13455=ORIENTED_EDGE('',*,*,#9908,.F.);
#13456=ORIENTED_EDGE('',*,*,#10020,.T.);
#13457=ORIENTED_EDGE('',*,*,#10021,.F.);
#13458=ORIENTED_EDGE('',*,*,#10022,.T.);
#13459=ORIENTED_EDGE('',*,*,#9909,.F.);
#13460=ORIENTED_EDGE('',*,*,#10022,.F.);
#13461=ORIENTED_EDGE('',*,*,#10023,.F.);
#13462=ORIENTED_EDGE('',*,*,#10024,.F.);
#13463=ORIENTED_EDGE('',*,*,#9910,.F.);
#13464=ORIENTED_EDGE('',*,*,#10024,.T.);
#13465=ORIENTED_EDGE('',*,*,#10025,.F.);
#13466=ORIENTED_EDGE('',*,*,#10026,.F.);
#13467=ORIENTED_EDGE('',*,*,#9911,.F.);
#13468=ORIENTED_EDGE('',*,*,#10026,.T.);
#13469=ORIENTED_EDGE('',*,*,#10027,.F.);
#13470=ORIENTED_EDGE('',*,*,#10028,.F.);
#13471=ORIENTED_EDGE('',*,*,#9912,.F.);
#13472=ORIENTED_EDGE('',*,*,#10028,.T.);
#13473=ORIENTED_EDGE('',*,*,#10029,.F.);
#13474=ORIENTED_EDGE('',*,*,#10030,.T.);
#13475=ORIENTED_EDGE('',*,*,#9913,.F.);
#13476=ORIENTED_EDGE('',*,*,#10030,.F.);
#13477=ORIENTED_EDGE('',*,*,#10031,.F.);
#13478=ORIENTED_EDGE('',*,*,#10032,.F.);
#13479=ORIENTED_EDGE('',*,*,#9914,.F.);
#13480=ORIENTED_EDGE('',*,*,#10032,.T.);
#13481=ORIENTED_EDGE('',*,*,#10033,.F.);
#13482=ORIENTED_EDGE('',*,*,#10034,.F.);
#13483=ORIENTED_EDGE('',*,*,#9915,.F.);
#13484=ORIENTED_EDGE('',*,*,#10034,.T.);
#13485=ORIENTED_EDGE('',*,*,#10035,.F.);
#13486=ORIENTED_EDGE('',*,*,#10036,.F.);
#13487=ORIENTED_EDGE('',*,*,#9916,.F.);
#13488=ORIENTED_EDGE('',*,*,#10036,.T.);
#13489=ORIENTED_EDGE('',*,*,#10037,.F.);
#13490=ORIENTED_EDGE('',*,*,#10038,.T.);
#13491=ORIENTED_EDGE('',*,*,#9917,.F.);
#13492=ORIENTED_EDGE('',*,*,#10038,.F.);
#13493=ORIENTED_EDGE('',*,*,#10039,.F.);
#13494=ORIENTED_EDGE('',*,*,#10040,.F.);
#13495=ORIENTED_EDGE('',*,*,#9918,.F.);
#13496=ORIENTED_EDGE('',*,*,#10040,.T.);
#13497=ORIENTED_EDGE('',*,*,#10041,.F.);
#13498=ORIENTED_EDGE('',*,*,#10042,.F.);
#13499=ORIENTED_EDGE('',*,*,#9919,.F.);
#13500=ORIENTED_EDGE('',*,*,#10042,.T.);
#13501=ORIENTED_EDGE('',*,*,#10043,.F.);
#13502=ORIENTED_EDGE('',*,*,#10044,.F.);
#13503=ORIENTED_EDGE('',*,*,#9920,.F.);
#13504=ORIENTED_EDGE('',*,*,#10044,.T.);
#13505=ORIENTED_EDGE('',*,*,#10045,.F.);
#13506=ORIENTED_EDGE('',*,*,#10046,.T.);
#13507=ORIENTED_EDGE('',*,*,#9921,.F.);
#13508=ORIENTED_EDGE('',*,*,#10046,.F.);
#13509=ORIENTED_EDGE('',*,*,#10047,.F.);
#13510=ORIENTED_EDGE('',*,*,#10048,.F.);
#13511=ORIENTED_EDGE('',*,*,#9922,.F.);
#13512=ORIENTED_EDGE('',*,*,#10048,.T.);
#13513=ORIENTED_EDGE('',*,*,#10049,.F.);
#13514=ORIENTED_EDGE('',*,*,#10050,.F.);
#13515=ORIENTED_EDGE('',*,*,#9923,.F.);
#13516=ORIENTED_EDGE('',*,*,#10050,.T.);
#13517=ORIENTED_EDGE('',*,*,#10051,.F.);
#13518=ORIENTED_EDGE('',*,*,#10052,.F.);
#13519=ORIENTED_EDGE('',*,*,#9924,.F.);
#13520=ORIENTED_EDGE('',*,*,#10052,.T.);
#13521=ORIENTED_EDGE('',*,*,#10053,.F.);
#13522=ORIENTED_EDGE('',*,*,#10054,.T.);
#13523=ORIENTED_EDGE('',*,*,#9925,.F.);
#13524=ORIENTED_EDGE('',*,*,#10054,.F.);
#13525=ORIENTED_EDGE('',*,*,#10055,.F.);
#13526=ORIENTED_EDGE('',*,*,#10056,.F.);
#13527=ORIENTED_EDGE('',*,*,#9926,.F.);
#13528=ORIENTED_EDGE('',*,*,#10056,.T.);
#13529=ORIENTED_EDGE('',*,*,#10057,.F.);
#13530=ORIENTED_EDGE('',*,*,#10058,.F.);
#13531=ORIENTED_EDGE('',*,*,#9927,.F.);
#13532=ORIENTED_EDGE('',*,*,#10058,.T.);
#13533=ORIENTED_EDGE('',*,*,#10059,.F.);
#13534=ORIENTED_EDGE('',*,*,#10060,.F.);
#13535=ORIENTED_EDGE('',*,*,#9928,.F.);
#13536=ORIENTED_EDGE('',*,*,#10060,.T.);
#13537=ORIENTED_EDGE('',*,*,#10061,.F.);
#13538=ORIENTED_EDGE('',*,*,#10062,.T.);
#13539=ORIENTED_EDGE('',*,*,#9929,.F.);
#13540=ORIENTED_EDGE('',*,*,#10062,.F.);
#13541=ORIENTED_EDGE('',*,*,#10063,.F.);
#13542=ORIENTED_EDGE('',*,*,#10064,.F.);
#13543=ORIENTED_EDGE('',*,*,#9930,.F.);
#13544=ORIENTED_EDGE('',*,*,#10064,.T.);
#13545=ORIENTED_EDGE('',*,*,#10065,.F.);
#13546=ORIENTED_EDGE('',*,*,#10066,.F.);
#13547=ORIENTED_EDGE('',*,*,#9931,.F.);
#13548=ORIENTED_EDGE('',*,*,#10066,.T.);
#13549=ORIENTED_EDGE('',*,*,#10067,.F.);
#13550=ORIENTED_EDGE('',*,*,#10068,.F.);
#13551=ORIENTED_EDGE('',*,*,#9932,.F.);
#13552=ORIENTED_EDGE('',*,*,#10068,.T.);
#13553=ORIENTED_EDGE('',*,*,#10069,.F.);
#13554=ORIENTED_EDGE('',*,*,#10070,.T.);
#13555=ORIENTED_EDGE('',*,*,#9933,.F.);
#13556=ORIENTED_EDGE('',*,*,#10070,.F.);
#13557=ORIENTED_EDGE('',*,*,#10071,.F.);
#13558=ORIENTED_EDGE('',*,*,#10072,.F.);
#13559=ORIENTED_EDGE('',*,*,#9934,.F.);
#13560=ORIENTED_EDGE('',*,*,#10072,.T.);
#13561=ORIENTED_EDGE('',*,*,#10073,.F.);
#13562=ORIENTED_EDGE('',*,*,#10074,.F.);
#13563=ORIENTED_EDGE('',*,*,#9935,.F.);
#13564=ORIENTED_EDGE('',*,*,#10074,.T.);
#13565=ORIENTED_EDGE('',*,*,#10075,.F.);
#13566=ORIENTED_EDGE('',*,*,#10076,.F.);
#13567=ORIENTED_EDGE('',*,*,#9936,.F.);
#13568=ORIENTED_EDGE('',*,*,#10076,.T.);
#13569=ORIENTED_EDGE('',*,*,#10077,.F.);
#13570=ORIENTED_EDGE('',*,*,#10078,.T.);
#13571=ORIENTED_EDGE('',*,*,#9937,.F.);
#13572=ORIENTED_EDGE('',*,*,#10078,.F.);
#13573=ORIENTED_EDGE('',*,*,#10079,.F.);
#13574=ORIENTED_EDGE('',*,*,#10080,.F.);
#13575=ORIENTED_EDGE('',*,*,#9938,.F.);
#13576=ORIENTED_EDGE('',*,*,#10080,.T.);
#13577=ORIENTED_EDGE('',*,*,#10081,.F.);
#13578=ORIENTED_EDGE('',*,*,#10082,.F.);
#13579=ORIENTED_EDGE('',*,*,#9939,.F.);
#13580=ORIENTED_EDGE('',*,*,#10082,.T.);
#13581=ORIENTED_EDGE('',*,*,#10083,.F.);
#13582=ORIENTED_EDGE('',*,*,#10084,.F.);
#13583=ORIENTED_EDGE('',*,*,#9940,.F.);
#13584=ORIENTED_EDGE('',*,*,#10084,.T.);
#13585=ORIENTED_EDGE('',*,*,#10085,.F.);
#13586=ORIENTED_EDGE('',*,*,#10086,.T.);
#13587=ORIENTED_EDGE('',*,*,#9941,.F.);
#13588=ORIENTED_EDGE('',*,*,#10086,.F.);
#13589=ORIENTED_EDGE('',*,*,#10087,.F.);
#13590=ORIENTED_EDGE('',*,*,#10088,.F.);
#13591=ORIENTED_EDGE('',*,*,#9942,.F.);
#13592=ORIENTED_EDGE('',*,*,#10088,.T.);
#13593=ORIENTED_EDGE('',*,*,#10089,.F.);
#13594=ORIENTED_EDGE('',*,*,#10090,.F.);
#13595=ORIENTED_EDGE('',*,*,#9943,.F.);
#13596=ORIENTED_EDGE('',*,*,#10090,.T.);
#13597=ORIENTED_EDGE('',*,*,#10091,.F.);
#13598=ORIENTED_EDGE('',*,*,#10092,.F.);
#13599=ORIENTED_EDGE('',*,*,#9944,.F.);
#13600=ORIENTED_EDGE('',*,*,#10092,.T.);
#13601=ORIENTED_EDGE('',*,*,#10093,.F.);
#13602=ORIENTED_EDGE('',*,*,#10094,.T.);
#13603=ORIENTED_EDGE('',*,*,#9945,.F.);
#13604=ORIENTED_EDGE('',*,*,#10094,.F.);
#13605=ORIENTED_EDGE('',*,*,#10095,.F.);
#13606=ORIENTED_EDGE('',*,*,#10096,.F.);
#13607=ORIENTED_EDGE('',*,*,#9946,.F.);
#13608=ORIENTED_EDGE('',*,*,#10096,.T.);
#13609=ORIENTED_EDGE('',*,*,#10097,.F.);
#13610=ORIENTED_EDGE('',*,*,#10098,.F.);
#13611=ORIENTED_EDGE('',*,*,#9947,.F.);
#13612=ORIENTED_EDGE('',*,*,#10098,.T.);
#13613=ORIENTED_EDGE('',*,*,#10099,.F.);
#13614=ORIENTED_EDGE('',*,*,#10100,.F.);
#13615=ORIENTED_EDGE('',*,*,#9948,.F.);
#13616=ORIENTED_EDGE('',*,*,#10100,.T.);
#13617=ORIENTED_EDGE('',*,*,#10101,.F.);
#13618=ORIENTED_EDGE('',*,*,#10102,.T.);
#13619=ORIENTED_EDGE('',*,*,#9949,.F.);
#13620=ORIENTED_EDGE('',*,*,#10102,.F.);
#13621=ORIENTED_EDGE('',*,*,#10103,.F.);
#13622=ORIENTED_EDGE('',*,*,#10104,.F.);
#13623=ORIENTED_EDGE('',*,*,#9950,.F.);
#13624=ORIENTED_EDGE('',*,*,#10104,.T.);
#13625=ORIENTED_EDGE('',*,*,#10105,.F.);
#13626=ORIENTED_EDGE('',*,*,#10106,.F.);
#13627=ORIENTED_EDGE('',*,*,#9951,.F.);
#13628=ORIENTED_EDGE('',*,*,#10106,.T.);
#13629=ORIENTED_EDGE('',*,*,#10107,.F.);
#13630=ORIENTED_EDGE('',*,*,#10108,.F.);
#13631=ORIENTED_EDGE('',*,*,#9952,.F.);
#13632=ORIENTED_EDGE('',*,*,#10108,.T.);
#13633=ORIENTED_EDGE('',*,*,#10109,.F.);
#13634=ORIENTED_EDGE('',*,*,#10110,.T.);
#13635=ORIENTED_EDGE('',*,*,#9953,.F.);
#13636=ORIENTED_EDGE('',*,*,#10110,.F.);
#13637=ORIENTED_EDGE('',*,*,#10111,.F.);
#13638=ORIENTED_EDGE('',*,*,#10112,.F.);
#13639=ORIENTED_EDGE('',*,*,#9954,.F.);
#13640=ORIENTED_EDGE('',*,*,#10112,.T.);
#13641=ORIENTED_EDGE('',*,*,#10113,.F.);
#13642=ORIENTED_EDGE('',*,*,#10114,.F.);
#13643=ORIENTED_EDGE('',*,*,#9955,.F.);
#13644=ORIENTED_EDGE('',*,*,#10114,.T.);
#13645=ORIENTED_EDGE('',*,*,#10115,.F.);
#13646=ORIENTED_EDGE('',*,*,#10116,.F.);
#13647=ORIENTED_EDGE('',*,*,#9956,.F.);
#13648=ORIENTED_EDGE('',*,*,#10116,.T.);
#13649=ORIENTED_EDGE('',*,*,#10117,.F.);
#13650=ORIENTED_EDGE('',*,*,#10118,.T.);
#13651=ORIENTED_EDGE('',*,*,#9957,.F.);
#13652=ORIENTED_EDGE('',*,*,#10118,.F.);
#13653=ORIENTED_EDGE('',*,*,#10119,.F.);
#13654=ORIENTED_EDGE('',*,*,#10120,.F.);
#13655=ORIENTED_EDGE('',*,*,#9958,.F.);
#13656=ORIENTED_EDGE('',*,*,#10120,.T.);
#13657=ORIENTED_EDGE('',*,*,#10121,.F.);
#13658=ORIENTED_EDGE('',*,*,#10122,.F.);
#13659=ORIENTED_EDGE('',*,*,#9959,.F.);
#13660=ORIENTED_EDGE('',*,*,#10122,.T.);
#13661=ORIENTED_EDGE('',*,*,#10123,.F.);
#13662=ORIENTED_EDGE('',*,*,#10124,.F.);
#13663=ORIENTED_EDGE('',*,*,#9960,.F.);
#13664=ORIENTED_EDGE('',*,*,#10124,.T.);
#13665=ORIENTED_EDGE('',*,*,#10125,.F.);
#13666=ORIENTED_EDGE('',*,*,#10126,.T.);
#13667=ORIENTED_EDGE('',*,*,#9961,.F.);
#13668=ORIENTED_EDGE('',*,*,#10126,.F.);
#13669=ORIENTED_EDGE('',*,*,#10127,.F.);
#13670=ORIENTED_EDGE('',*,*,#10128,.F.);
#13671=ORIENTED_EDGE('',*,*,#9962,.F.);
#13672=ORIENTED_EDGE('',*,*,#10128,.T.);
#13673=ORIENTED_EDGE('',*,*,#10129,.F.);
#13674=ORIENTED_EDGE('',*,*,#10130,.F.);
#13675=ORIENTED_EDGE('',*,*,#9963,.F.);
#13676=ORIENTED_EDGE('',*,*,#10130,.T.);
#13677=ORIENTED_EDGE('',*,*,#10131,.F.);
#13678=ORIENTED_EDGE('',*,*,#10132,.F.);
#13679=ORIENTED_EDGE('',*,*,#9964,.F.);
#13680=ORIENTED_EDGE('',*,*,#10133,.T.);
#13681=ORIENTED_EDGE('',*,*,#10131,.T.);
#13682=ORIENTED_EDGE('',*,*,#10129,.T.);
#13683=ORIENTED_EDGE('',*,*,#10127,.T.);
#13684=ORIENTED_EDGE('',*,*,#10125,.T.);
#13685=ORIENTED_EDGE('',*,*,#10123,.T.);
#13686=ORIENTED_EDGE('',*,*,#10121,.T.);
#13687=ORIENTED_EDGE('',*,*,#10119,.T.);
#13688=ORIENTED_EDGE('',*,*,#10117,.T.);
#13689=ORIENTED_EDGE('',*,*,#10115,.T.);
#13690=ORIENTED_EDGE('',*,*,#10113,.T.);
#13691=ORIENTED_EDGE('',*,*,#10111,.T.);
#13692=ORIENTED_EDGE('',*,*,#10109,.T.);
#13693=ORIENTED_EDGE('',*,*,#10107,.T.);
#13694=ORIENTED_EDGE('',*,*,#10105,.T.);
#13695=ORIENTED_EDGE('',*,*,#10103,.T.);
#13696=ORIENTED_EDGE('',*,*,#10101,.T.);
#13697=ORIENTED_EDGE('',*,*,#10099,.T.);
#13698=ORIENTED_EDGE('',*,*,#10097,.T.);
#13699=ORIENTED_EDGE('',*,*,#10095,.T.);
#13700=ORIENTED_EDGE('',*,*,#10093,.T.);
#13701=ORIENTED_EDGE('',*,*,#10091,.T.);
#13702=ORIENTED_EDGE('',*,*,#10089,.T.);
#13703=ORIENTED_EDGE('',*,*,#10087,.T.);
#13704=ORIENTED_EDGE('',*,*,#10085,.T.);
#13705=ORIENTED_EDGE('',*,*,#10083,.T.);
#13706=ORIENTED_EDGE('',*,*,#10081,.T.);
#13707=ORIENTED_EDGE('',*,*,#10079,.T.);
#13708=ORIENTED_EDGE('',*,*,#10077,.T.);
#13709=ORIENTED_EDGE('',*,*,#10075,.T.);
#13710=ORIENTED_EDGE('',*,*,#10073,.T.);
#13711=ORIENTED_EDGE('',*,*,#10071,.T.);
#13712=ORIENTED_EDGE('',*,*,#10069,.T.);
#13713=ORIENTED_EDGE('',*,*,#10067,.T.);
#13714=ORIENTED_EDGE('',*,*,#10065,.T.);
#13715=ORIENTED_EDGE('',*,*,#10063,.T.);
#13716=ORIENTED_EDGE('',*,*,#10061,.T.);
#13717=ORIENTED_EDGE('',*,*,#10059,.T.);
#13718=ORIENTED_EDGE('',*,*,#10057,.T.);
#13719=ORIENTED_EDGE('',*,*,#10055,.T.);
#13720=ORIENTED_EDGE('',*,*,#10053,.T.);
#13721=ORIENTED_EDGE('',*,*,#10051,.T.);
#13722=ORIENTED_EDGE('',*,*,#10049,.T.);
#13723=ORIENTED_EDGE('',*,*,#10047,.T.);
#13724=ORIENTED_EDGE('',*,*,#10045,.T.);
#13725=ORIENTED_EDGE('',*,*,#10043,.T.);
#13726=ORIENTED_EDGE('',*,*,#10041,.T.);
#13727=ORIENTED_EDGE('',*,*,#10039,.T.);
#13728=ORIENTED_EDGE('',*,*,#10037,.T.);
#13729=ORIENTED_EDGE('',*,*,#10035,.T.);
#13730=ORIENTED_EDGE('',*,*,#10033,.T.);
#13731=ORIENTED_EDGE('',*,*,#10031,.T.);
#13732=ORIENTED_EDGE('',*,*,#10029,.T.);
#13733=ORIENTED_EDGE('',*,*,#10027,.T.);
#13734=ORIENTED_EDGE('',*,*,#10025,.T.);
#13735=ORIENTED_EDGE('',*,*,#10023,.T.);
#13736=ORIENTED_EDGE('',*,*,#10021,.T.);
#13737=ORIENTED_EDGE('',*,*,#10019,.T.);
#13738=ORIENTED_EDGE('',*,*,#10017,.T.);
#13739=ORIENTED_EDGE('',*,*,#10015,.T.);
#13740=ORIENTED_EDGE('',*,*,#10013,.T.);
#13741=ORIENTED_EDGE('',*,*,#10011,.T.);
#13742=ORIENTED_EDGE('',*,*,#10009,.T.);
#13743=ORIENTED_EDGE('',*,*,#10007,.T.);
#13744=ORIENTED_EDGE('',*,*,#10005,.T.);
#13745=ORIENTED_EDGE('',*,*,#10003,.T.);
#13746=ORIENTED_EDGE('',*,*,#10001,.T.);
#13747=ORIENTED_EDGE('',*,*,#9999,.T.);
#13748=ORIENTED_EDGE('',*,*,#9997,.T.);
#13749=ORIENTED_EDGE('',*,*,#9995,.T.);
#13750=ORIENTED_EDGE('',*,*,#9993,.T.);
#13751=ORIENTED_EDGE('',*,*,#9991,.T.);
#13752=ORIENTED_EDGE('',*,*,#9989,.T.);
#13753=ORIENTED_EDGE('',*,*,#9987,.T.);
#13754=ORIENTED_EDGE('',*,*,#9985,.T.);
#13755=ORIENTED_EDGE('',*,*,#9983,.T.);
#13756=ORIENTED_EDGE('',*,*,#9981,.T.);
#13757=ORIENTED_EDGE('',*,*,#9979,.T.);
#13758=ORIENTED_EDGE('',*,*,#9977,.T.);
#13759=ORIENTED_EDGE('',*,*,#9975,.T.);
#13760=ORIENTED_EDGE('',*,*,#9973,.T.);
#13761=ORIENTED_EDGE('',*,*,#9974,.T.);
#13762=ORIENTED_EDGE('',*,*,#9965,.F.);
#13763=ORIENTED_EDGE('',*,*,#10132,.T.);
#13764=ORIENTED_EDGE('',*,*,#10133,.F.);
#13765=ORIENTED_EDGE('',*,*,#10134,.F.);
#13766=ORIENTED_EDGE('',*,*,#10135,.F.);
#13767=ORIENTED_EDGE('',*,*,#10136,.F.);
#13768=ORIENTED_EDGE('',*,*,#10137,.F.);
#13769=ORIENTED_EDGE('',*,*,#10138,.F.);
#13770=ORIENTED_EDGE('',*,*,#10139,.F.);
#13771=ORIENTED_EDGE('',*,*,#10140,.F.);
#13772=ORIENTED_EDGE('',*,*,#10141,.F.);
#13773=ORIENTED_EDGE('',*,*,#10138,.T.);
#13774=ORIENTED_EDGE('',*,*,#10142,.T.);
#13775=ORIENTED_EDGE('',*,*,#10143,.T.);
#13776=ORIENTED_EDGE('',*,*,#10144,.T.);
#13777=ORIENTED_EDGE('',*,*,#10137,.T.);
#13778=ORIENTED_EDGE('',*,*,#10145,.F.);
#13779=ORIENTED_EDGE('',*,*,#10146,.T.);
#13780=ORIENTED_EDGE('',*,*,#10142,.F.);
#13781=ORIENTED_EDGE('',*,*,#10136,.T.);
#13782=ORIENTED_EDGE('',*,*,#10147,.T.);
#13783=ORIENTED_EDGE('',*,*,#10148,.T.);
#13784=ORIENTED_EDGE('',*,*,#10145,.T.);
#13785=ORIENTED_EDGE('',*,*,#10135,.T.);
#13786=ORIENTED_EDGE('',*,*,#10149,.F.);
#13787=ORIENTED_EDGE('',*,*,#10150,.T.);
#13788=ORIENTED_EDGE('',*,*,#10147,.F.);
#13789=ORIENTED_EDGE('',*,*,#10143,.F.);
#13790=ORIENTED_EDGE('',*,*,#10146,.F.);
#13791=ORIENTED_EDGE('',*,*,#10148,.F.);
#13792=ORIENTED_EDGE('',*,*,#10150,.F.);
#13793=ORIENTED_EDGE('',*,*,#10151,.F.);
#13794=ORIENTED_EDGE('',*,*,#10152,.F.);
#13795=ORIENTED_EDGE('',*,*,#10153,.F.);
#13796=ORIENTED_EDGE('',*,*,#10154,.F.);
#13797=ORIENTED_EDGE('',*,*,#10134,.T.);
#13798=ORIENTED_EDGE('',*,*,#10155,.T.);
#13799=ORIENTED_EDGE('',*,*,#10151,.T.);
#13800=ORIENTED_EDGE('',*,*,#10149,.T.);
#13801=ORIENTED_EDGE('',*,*,#10141,.T.);
#13802=ORIENTED_EDGE('',*,*,#10156,.F.);
#13803=ORIENTED_EDGE('',*,*,#10152,.T.);
#13804=ORIENTED_EDGE('',*,*,#10155,.F.);
#13805=ORIENTED_EDGE('',*,*,#10140,.T.);
#13806=ORIENTED_EDGE('',*,*,#10157,.T.);
#13807=ORIENTED_EDGE('',*,*,#10153,.T.);
#13808=ORIENTED_EDGE('',*,*,#10156,.T.);
#13809=ORIENTED_EDGE('',*,*,#10139,.T.);
#13810=ORIENTED_EDGE('',*,*,#10144,.F.);
#13811=ORIENTED_EDGE('',*,*,#10154,.T.);
#13812=ORIENTED_EDGE('',*,*,#10157,.F.);
#13813=ORIENTED_EDGE('',*,*,#10158,.F.);
#13814=ORIENTED_EDGE('',*,*,#10159,.T.);
#13815=ORIENTED_EDGE('',*,*,#10160,.F.);
#13816=ORIENTED_EDGE('',*,*,#10159,.F.);
#13817=ORIENTED_EDGE('',*,*,#10158,.T.);
#13818=ORIENTED_EDGE('',*,*,#10161,.F.);
#13819=ORIENTED_EDGE('',*,*,#10162,.T.);
#13820=ORIENTED_EDGE('',*,*,#10163,.F.);
#13821=ORIENTED_EDGE('',*,*,#10164,.T.);
#13822=ORIENTED_EDGE('',*,*,#10165,.F.);
#13823=ORIENTED_EDGE('',*,*,#10164,.F.);
#13824=ORIENTED_EDGE('',*,*,#10166,.F.);
#13825=ORIENTED_EDGE('',*,*,#10167,.F.);
#13826=ORIENTED_EDGE('',*,*,#10168,.F.);
#13827=ORIENTED_EDGE('',*,*,#10167,.T.);
#13828=ORIENTED_EDGE('',*,*,#10169,.T.);
#13829=ORIENTED_EDGE('',*,*,#10170,.T.);
#13830=ORIENTED_EDGE('',*,*,#10166,.T.);
#13831=ORIENTED_EDGE('',*,*,#10163,.T.);
#13832=ORIENTED_EDGE('',*,*,#10171,.T.);
#13833=ORIENTED_EDGE('',*,*,#10169,.F.);
#13834=ORIENTED_EDGE('',*,*,#10172,.F.);
#13835=ORIENTED_EDGE('',*,*,#10170,.F.);
#13836=ORIENTED_EDGE('',*,*,#10171,.F.);
#13837=ORIENTED_EDGE('',*,*,#10162,.F.);
#13838=ORIENTED_EDGE('',*,*,#10173,.T.);
#13839=ORIENTED_EDGE('',*,*,#10174,.F.);
#13840=ORIENTED_EDGE('',*,*,#10175,.F.);
#13841=ORIENTED_EDGE('',*,*,#10176,.F.);
#13842=ORIENTED_EDGE('',*,*,#10173,.F.);
#13843=ORIENTED_EDGE('',*,*,#10177,.T.);
#13844=ORIENTED_EDGE('',*,*,#10175,.T.);
#13845=ORIENTED_EDGE('',*,*,#10177,.F.);
#13846=ORIENTED_EDGE('',*,*,#10176,.T.);
#13847=ORIENTED_EDGE('',*,*,#10178,.T.);
#13848=ORIENTED_EDGE('',*,*,#10179,.T.);
#13849=ORIENTED_EDGE('',*,*,#10178,.F.);
#13850=ORIENTED_EDGE('',*,*,#10180,.F.);
#13851=ORIENTED_EDGE('',*,*,#10181,.T.);
#13852=ORIENTED_EDGE('',*,*,#10174,.T.);
#13853=ORIENTED_EDGE('',*,*,#10181,.F.);
#13854=ORIENTED_EDGE('',*,*,#10168,.T.);
#13855=ORIENTED_EDGE('',*,*,#10172,.T.);
#13856=ORIENTED_EDGE('',*,*,#10161,.T.);
#13857=ORIENTED_EDGE('',*,*,#10165,.T.);
#13858=ORIENTED_EDGE('',*,*,#10180,.T.);
#13859=ORIENTED_EDGE('',*,*,#10160,.T.);
#13860=ORIENTED_EDGE('',*,*,#10179,.F.);
#13861=ORIENTED_EDGE('',*,*,#10182,.F.);
#13862=ORIENTED_EDGE('',*,*,#10183,.T.);
#13863=ORIENTED_EDGE('',*,*,#10184,.T.);
#13864=ORIENTED_EDGE('',*,*,#10183,.F.);
#13865=ORIENTED_EDGE('',*,*,#10185,.F.);
#13866=ORIENTED_EDGE('',*,*,#10186,.T.);
#13867=ORIENTED_EDGE('',*,*,#10187,.T.);
#13868=ORIENTED_EDGE('',*,*,#10186,.F.);
#13869=ORIENTED_EDGE('',*,*,#10185,.T.);
#13870=ORIENTED_EDGE('',*,*,#10182,.T.);
#13871=ORIENTED_EDGE('',*,*,#10187,.F.);
#13872=ORIENTED_EDGE('',*,*,#10184,.F.);
#13873=ORIENTED_EDGE('',*,*,#10188,.F.);
#13874=ORIENTED_EDGE('',*,*,#10189,.T.);
#13875=ORIENTED_EDGE('',*,*,#10190,.T.);
#13876=ORIENTED_EDGE('',*,*,#10189,.F.);
#13877=ORIENTED_EDGE('',*,*,#10191,.F.);
#13878=ORIENTED_EDGE('',*,*,#10192,.T.);
#13879=ORIENTED_EDGE('',*,*,#10193,.T.);
#13880=ORIENTED_EDGE('',*,*,#10192,.F.);
#13881=ORIENTED_EDGE('',*,*,#10191,.T.);
#13882=ORIENTED_EDGE('',*,*,#10188,.T.);
#13883=ORIENTED_EDGE('',*,*,#10193,.F.);
#13884=ORIENTED_EDGE('',*,*,#10190,.F.);
#13885=ORIENTED_EDGE('',*,*,#10194,.F.);
#13886=ORIENTED_EDGE('',*,*,#10195,.T.);
#13887=ORIENTED_EDGE('',*,*,#10196,.F.);
#13888=ORIENTED_EDGE('',*,*,#10197,.F.);
#13889=ORIENTED_EDGE('',*,*,#10198,.T.);
#13890=ORIENTED_EDGE('',*,*,#10199,.F.);
#13891=ORIENTED_EDGE('',*,*,#10200,.F.);
#13892=ORIENTED_EDGE('',*,*,#10198,.F.);
#13893=ORIENTED_EDGE('',*,*,#10201,.F.);
#13894=ORIENTED_EDGE('',*,*,#10202,.F.);
#13895=ORIENTED_EDGE('',*,*,#10195,.F.);
#13896=ORIENTED_EDGE('',*,*,#10203,.F.);
#13897=ORIENTED_EDGE('',*,*,#10201,.T.);
#13898=ORIENTED_EDGE('',*,*,#10197,.T.);
#13899=ORIENTED_EDGE('',*,*,#10204,.F.);
#13900=ORIENTED_EDGE('',*,*,#10205,.T.);
#13901=ORIENTED_EDGE('',*,*,#10206,.T.);
#13902=ORIENTED_EDGE('',*,*,#10205,.F.);
#13903=ORIENTED_EDGE('',*,*,#10202,.T.);
#13904=ORIENTED_EDGE('',*,*,#10203,.T.);
#13905=ORIENTED_EDGE('',*,*,#10196,.T.);
#13906=ORIENTED_EDGE('',*,*,#10194,.T.);
#13907=ORIENTED_EDGE('',*,*,#10207,.F.);
#13908=ORIENTED_EDGE('',*,*,#10208,.T.);
#13909=ORIENTED_EDGE('',*,*,#10209,.T.);
#13910=ORIENTED_EDGE('',*,*,#10208,.F.);
#13911=ORIENTED_EDGE('',*,*,#10199,.T.);
#13912=ORIENTED_EDGE('',*,*,#10200,.T.);
#13913=ORIENTED_EDGE('',*,*,#10207,.T.);
#13914=ORIENTED_EDGE('',*,*,#10204,.T.);
#13915=ORIENTED_EDGE('',*,*,#10209,.F.);
#13916=ORIENTED_EDGE('',*,*,#10206,.F.);
#13917=ORIENTED_EDGE('',*,*,#10210,.F.);
#13918=ORIENTED_EDGE('',*,*,#10211,.T.);
#13919=ORIENTED_EDGE('',*,*,#10212,.T.);
#13920=ORIENTED_EDGE('',*,*,#10211,.F.);
#13921=ORIENTED_EDGE('',*,*,#10213,.F.);
#13922=ORIENTED_EDGE('',*,*,#10214,.T.);
#13923=ORIENTED_EDGE('',*,*,#10215,.T.);
#13924=ORIENTED_EDGE('',*,*,#10214,.F.);
#13925=ORIENTED_EDGE('',*,*,#10213,.T.);
#13926=ORIENTED_EDGE('',*,*,#10210,.T.);
#13927=ORIENTED_EDGE('',*,*,#10215,.F.);
#13928=ORIENTED_EDGE('',*,*,#10212,.F.);
#13929=ORIENTED_EDGE('',*,*,#10216,.F.);
#13930=ORIENTED_EDGE('',*,*,#10217,.T.);
#13931=ORIENTED_EDGE('',*,*,#10218,.T.);
#13932=ORIENTED_EDGE('',*,*,#10217,.F.);
#13933=ORIENTED_EDGE('',*,*,#10219,.F.);
#13934=ORIENTED_EDGE('',*,*,#10220,.T.);
#13935=ORIENTED_EDGE('',*,*,#10221,.T.);
#13936=ORIENTED_EDGE('',*,*,#10220,.F.);
#13937=ORIENTED_EDGE('',*,*,#10219,.T.);
#13938=ORIENTED_EDGE('',*,*,#10216,.T.);
#13939=ORIENTED_EDGE('',*,*,#10221,.F.);
#13940=ORIENTED_EDGE('',*,*,#10218,.F.);
#13941=ORIENTED_EDGE('',*,*,#10222,.F.);
#13942=ORIENTED_EDGE('',*,*,#10223,.T.);
#13943=ORIENTED_EDGE('',*,*,#10224,.F.);
#13944=ORIENTED_EDGE('',*,*,#10225,.F.);
#13945=ORIENTED_EDGE('',*,*,#10226,.T.);
#13946=ORIENTED_EDGE('',*,*,#10227,.F.);
#13947=ORIENTED_EDGE('',*,*,#10228,.F.);
#13948=ORIENTED_EDGE('',*,*,#10226,.F.);
#13949=ORIENTED_EDGE('',*,*,#10229,.F.);
#13950=ORIENTED_EDGE('',*,*,#10230,.F.);
#13951=ORIENTED_EDGE('',*,*,#10223,.F.);
#13952=ORIENTED_EDGE('',*,*,#10231,.F.);
#13953=ORIENTED_EDGE('',*,*,#10229,.T.);
#13954=ORIENTED_EDGE('',*,*,#10225,.T.);
#13955=ORIENTED_EDGE('',*,*,#10232,.F.);
#13956=ORIENTED_EDGE('',*,*,#10233,.T.);
#13957=ORIENTED_EDGE('',*,*,#10234,.T.);
#13958=ORIENTED_EDGE('',*,*,#10235,.F.);
#13959=ORIENTED_EDGE('',*,*,#10236,.F.);
#13960=ORIENTED_EDGE('',*,*,#10237,.F.);
#13961=ORIENTED_EDGE('',*,*,#10233,.F.);
#13962=ORIENTED_EDGE('',*,*,#10238,.F.);
#13963=ORIENTED_EDGE('',*,*,#10235,.T.);
#13964=ORIENTED_EDGE('',*,*,#10239,.T.);
#13965=ORIENTED_EDGE('',*,*,#10240,.F.);
#13966=ORIENTED_EDGE('',*,*,#10239,.F.);
#13967=ORIENTED_EDGE('',*,*,#10234,.F.);
#13968=ORIENTED_EDGE('',*,*,#10237,.T.);
#13969=ORIENTED_EDGE('',*,*,#10241,.F.);
#13970=ORIENTED_EDGE('',*,*,#10242,.T.);
#13971=ORIENTED_EDGE('',*,*,#10243,.T.);
#13972=ORIENTED_EDGE('',*,*,#10242,.F.);
#13973=ORIENTED_EDGE('',*,*,#10230,.T.);
#13974=ORIENTED_EDGE('',*,*,#10231,.T.);
#13975=ORIENTED_EDGE('',*,*,#10224,.T.);
#13976=ORIENTED_EDGE('',*,*,#10222,.T.);
#13977=ORIENTED_EDGE('',*,*,#10244,.F.);
#13978=ORIENTED_EDGE('',*,*,#10245,.T.);
#13979=ORIENTED_EDGE('',*,*,#10246,.T.);
#13980=ORIENTED_EDGE('',*,*,#10245,.F.);
#13981=ORIENTED_EDGE('',*,*,#10227,.T.);
#13982=ORIENTED_EDGE('',*,*,#10228,.T.);
#13983=ORIENTED_EDGE('',*,*,#10240,.T.);
#13984=ORIENTED_EDGE('',*,*,#10236,.T.);
#13985=ORIENTED_EDGE('',*,*,#10232,.T.);
#13986=ORIENTED_EDGE('',*,*,#10238,.T.);
#13987=ORIENTED_EDGE('',*,*,#10244,.T.);
#13988=ORIENTED_EDGE('',*,*,#10241,.T.);
#13989=ORIENTED_EDGE('',*,*,#10246,.F.);
#13990=ORIENTED_EDGE('',*,*,#10243,.F.);
#13991=ORIENTED_EDGE('',*,*,#10247,.F.);
#13992=ORIENTED_EDGE('',*,*,#10248,.T.);
#13993=ORIENTED_EDGE('',*,*,#10249,.T.);
#13994=ORIENTED_EDGE('',*,*,#10248,.F.);
#13995=ORIENTED_EDGE('',*,*,#10250,.F.);
#13996=ORIENTED_EDGE('',*,*,#10251,.T.);
#13997=ORIENTED_EDGE('',*,*,#10252,.T.);
#13998=ORIENTED_EDGE('',*,*,#10251,.F.);
#13999=ORIENTED_EDGE('',*,*,#10250,.T.);
#14000=ORIENTED_EDGE('',*,*,#10247,.T.);
#14001=ORIENTED_EDGE('',*,*,#10252,.F.);
#14002=ORIENTED_EDGE('',*,*,#10249,.F.);
#14003=ORIENTED_EDGE('',*,*,#10253,.F.);
#14004=ORIENTED_EDGE('',*,*,#10254,.F.);
#14005=ORIENTED_EDGE('',*,*,#10255,.F.);
#14006=ORIENTED_EDGE('',*,*,#10256,.F.);
#14007=ORIENTED_EDGE('',*,*,#10257,.F.);
#14008=ORIENTED_EDGE('',*,*,#10258,.T.);
#14009=ORIENTED_EDGE('',*,*,#10259,.F.);
#14010=ORIENTED_EDGE('',*,*,#10254,.T.);
#14011=ORIENTED_EDGE('',*,*,#10260,.F.);
#14012=ORIENTED_EDGE('',*,*,#10261,.F.);
#14013=ORIENTED_EDGE('',*,*,#10262,.F.);
#14014=ORIENTED_EDGE('',*,*,#10258,.F.);
#14015=ORIENTED_EDGE('',*,*,#10263,.T.);
#14016=ORIENTED_EDGE('',*,*,#10264,.T.);
#14017=ORIENTED_EDGE('',*,*,#10265,.T.);
#14018=ORIENTED_EDGE('',*,*,#10266,.T.);
#14019=ORIENTED_EDGE('',*,*,#10267,.T.);
#14020=ORIENTED_EDGE('',*,*,#10268,.T.);
#14021=ORIENTED_EDGE('',*,*,#10269,.T.);
#14022=ORIENTED_EDGE('',*,*,#10270,.T.);
#14023=ORIENTED_EDGE('',*,*,#10271,.T.);
#14024=ORIENTED_EDGE('',*,*,#10272,.T.);
#14025=ORIENTED_EDGE('',*,*,#10273,.T.);
#14026=ORIENTED_EDGE('',*,*,#10274,.T.);
#14027=ORIENTED_EDGE('',*,*,#10275,.T.);
#14028=ORIENTED_EDGE('',*,*,#10276,.T.);
#14029=ORIENTED_EDGE('',*,*,#10277,.T.);
#14030=ORIENTED_EDGE('',*,*,#10278,.T.);
#14031=ORIENTED_EDGE('',*,*,#10279,.T.);
#14032=ORIENTED_EDGE('',*,*,#10280,.T.);
#14033=ORIENTED_EDGE('',*,*,#10281,.T.);
#14034=ORIENTED_EDGE('',*,*,#10282,.T.);
#14035=ORIENTED_EDGE('',*,*,#10283,.T.);
#14036=ORIENTED_EDGE('',*,*,#10284,.T.);
#14037=ORIENTED_EDGE('',*,*,#10285,.T.);
#14038=ORIENTED_EDGE('',*,*,#10286,.T.);
#14039=ORIENTED_EDGE('',*,*,#10287,.T.);
#14040=ORIENTED_EDGE('',*,*,#10288,.T.);
#14041=ORIENTED_EDGE('',*,*,#10289,.T.);
#14042=ORIENTED_EDGE('',*,*,#10290,.T.);
#14043=ORIENTED_EDGE('',*,*,#10291,.T.);
#14044=ORIENTED_EDGE('',*,*,#10292,.T.);
#14045=ORIENTED_EDGE('',*,*,#10293,.T.);
#14046=ORIENTED_EDGE('',*,*,#10294,.T.);
#14047=ORIENTED_EDGE('',*,*,#10295,.T.);
#14048=ORIENTED_EDGE('',*,*,#10296,.T.);
#14049=ORIENTED_EDGE('',*,*,#10297,.T.);
#14050=ORIENTED_EDGE('',*,*,#10298,.T.);
#14051=ORIENTED_EDGE('',*,*,#10299,.T.);
#14052=ORIENTED_EDGE('',*,*,#10300,.T.);
#14053=ORIENTED_EDGE('',*,*,#10301,.T.);
#14054=ORIENTED_EDGE('',*,*,#10302,.T.);
#14055=ORIENTED_EDGE('',*,*,#10303,.T.);
#14056=ORIENTED_EDGE('',*,*,#10304,.T.);
#14057=ORIENTED_EDGE('',*,*,#10305,.T.);
#14058=ORIENTED_EDGE('',*,*,#10306,.T.);
#14059=ORIENTED_EDGE('',*,*,#10307,.T.);
#14060=ORIENTED_EDGE('',*,*,#10308,.T.);
#14061=ORIENTED_EDGE('',*,*,#10309,.T.);
#14062=ORIENTED_EDGE('',*,*,#10310,.T.);
#14063=ORIENTED_EDGE('',*,*,#10311,.T.);
#14064=ORIENTED_EDGE('',*,*,#10312,.T.);
#14065=ORIENTED_EDGE('',*,*,#10313,.T.);
#14066=ORIENTED_EDGE('',*,*,#10314,.T.);
#14067=ORIENTED_EDGE('',*,*,#10315,.T.);
#14068=ORIENTED_EDGE('',*,*,#10316,.T.);
#14069=ORIENTED_EDGE('',*,*,#10317,.T.);
#14070=ORIENTED_EDGE('',*,*,#10318,.T.);
#14071=ORIENTED_EDGE('',*,*,#10319,.T.);
#14072=ORIENTED_EDGE('',*,*,#10320,.T.);
#14073=ORIENTED_EDGE('',*,*,#10321,.T.);
#14074=ORIENTED_EDGE('',*,*,#10322,.T.);
#14075=ORIENTED_EDGE('',*,*,#10323,.T.);
#14076=ORIENTED_EDGE('',*,*,#10324,.T.);
#14077=ORIENTED_EDGE('',*,*,#10325,.T.);
#14078=ORIENTED_EDGE('',*,*,#10326,.T.);
#14079=ORIENTED_EDGE('',*,*,#10327,.T.);
#14080=ORIENTED_EDGE('',*,*,#10328,.T.);
#14081=ORIENTED_EDGE('',*,*,#10329,.T.);
#14082=ORIENTED_EDGE('',*,*,#10330,.T.);
#14083=ORIENTED_EDGE('',*,*,#10331,.T.);
#14084=ORIENTED_EDGE('',*,*,#10332,.T.);
#14085=ORIENTED_EDGE('',*,*,#10333,.T.);
#14086=ORIENTED_EDGE('',*,*,#10334,.T.);
#14087=ORIENTED_EDGE('',*,*,#10335,.T.);
#14088=ORIENTED_EDGE('',*,*,#10336,.T.);
#14089=ORIENTED_EDGE('',*,*,#10337,.T.);
#14090=ORIENTED_EDGE('',*,*,#10338,.T.);
#14091=ORIENTED_EDGE('',*,*,#10339,.T.);
#14092=ORIENTED_EDGE('',*,*,#10340,.T.);
#14093=ORIENTED_EDGE('',*,*,#10341,.T.);
#14094=ORIENTED_EDGE('',*,*,#10342,.T.);
#14095=ORIENTED_EDGE('',*,*,#10343,.T.);
#14096=ORIENTED_EDGE('',*,*,#10344,.T.);
#14097=ORIENTED_EDGE('',*,*,#10345,.T.);
#14098=ORIENTED_EDGE('',*,*,#10346,.T.);
#14099=ORIENTED_EDGE('',*,*,#10347,.T.);
#14100=ORIENTED_EDGE('',*,*,#10348,.T.);
#14101=ORIENTED_EDGE('',*,*,#10349,.T.);
#14102=ORIENTED_EDGE('',*,*,#10350,.T.);
#14103=ORIENTED_EDGE('',*,*,#10351,.T.);
#14104=ORIENTED_EDGE('',*,*,#10352,.T.);
#14105=ORIENTED_EDGE('',*,*,#10353,.T.);
#14106=ORIENTED_EDGE('',*,*,#10354,.T.);
#14107=ORIENTED_EDGE('',*,*,#10355,.T.);
#14108=ORIENTED_EDGE('',*,*,#10356,.T.);
#14109=ORIENTED_EDGE('',*,*,#10357,.T.);
#14110=ORIENTED_EDGE('',*,*,#10358,.T.);
#14111=ORIENTED_EDGE('',*,*,#10359,.T.);
#14112=ORIENTED_EDGE('',*,*,#10360,.T.);
#14113=ORIENTED_EDGE('',*,*,#10361,.T.);
#14114=ORIENTED_EDGE('',*,*,#10362,.T.);
#14115=ORIENTED_EDGE('',*,*,#10363,.T.);
#14116=ORIENTED_EDGE('',*,*,#10364,.T.);
#14117=ORIENTED_EDGE('',*,*,#10365,.T.);
#14118=ORIENTED_EDGE('',*,*,#10366,.T.);
#14119=ORIENTED_EDGE('',*,*,#10367,.T.);
#14120=ORIENTED_EDGE('',*,*,#10368,.T.);
#14121=ORIENTED_EDGE('',*,*,#10369,.T.);
#14122=ORIENTED_EDGE('',*,*,#10370,.T.);
#14123=ORIENTED_EDGE('',*,*,#10371,.T.);
#14124=ORIENTED_EDGE('',*,*,#10372,.T.);
#14125=ORIENTED_EDGE('',*,*,#10373,.T.);
#14126=ORIENTED_EDGE('',*,*,#10374,.T.);
#14127=ORIENTED_EDGE('',*,*,#10375,.T.);
#14128=ORIENTED_EDGE('',*,*,#10376,.T.);
#14129=ORIENTED_EDGE('',*,*,#10377,.T.);
#14130=ORIENTED_EDGE('',*,*,#10378,.T.);
#14131=ORIENTED_EDGE('',*,*,#10379,.T.);
#14132=ORIENTED_EDGE('',*,*,#10380,.T.);
#14133=ORIENTED_EDGE('',*,*,#10381,.T.);
#14134=ORIENTED_EDGE('',*,*,#10382,.T.);
#14135=ORIENTED_EDGE('',*,*,#10383,.T.);
#14136=ORIENTED_EDGE('',*,*,#10384,.T.);
#14137=ORIENTED_EDGE('',*,*,#10385,.T.);
#14138=ORIENTED_EDGE('',*,*,#10386,.T.);
#14139=ORIENTED_EDGE('',*,*,#10387,.T.);
#14140=ORIENTED_EDGE('',*,*,#10388,.T.);
#14141=ORIENTED_EDGE('',*,*,#10389,.T.);
#14142=ORIENTED_EDGE('',*,*,#10390,.T.);
#14143=ORIENTED_EDGE('',*,*,#10391,.T.);
#14144=ORIENTED_EDGE('',*,*,#10392,.T.);
#14145=ORIENTED_EDGE('',*,*,#10393,.T.);
#14146=ORIENTED_EDGE('',*,*,#10394,.T.);
#14147=ORIENTED_EDGE('',*,*,#10395,.T.);
#14148=ORIENTED_EDGE('',*,*,#10396,.T.);
#14149=ORIENTED_EDGE('',*,*,#10397,.T.);
#14150=ORIENTED_EDGE('',*,*,#10398,.T.);
#14151=ORIENTED_EDGE('',*,*,#10399,.T.);
#14152=ORIENTED_EDGE('',*,*,#10400,.T.);
#14153=ORIENTED_EDGE('',*,*,#10401,.T.);
#14154=ORIENTED_EDGE('',*,*,#10402,.T.);
#14155=ORIENTED_EDGE('',*,*,#10403,.T.);
#14156=ORIENTED_EDGE('',*,*,#10404,.T.);
#14157=ORIENTED_EDGE('',*,*,#10405,.T.);
#14158=ORIENTED_EDGE('',*,*,#10406,.T.);
#14159=ORIENTED_EDGE('',*,*,#10407,.T.);
#14160=ORIENTED_EDGE('',*,*,#10408,.T.);
#14161=ORIENTED_EDGE('',*,*,#10409,.T.);
#14162=ORIENTED_EDGE('',*,*,#10410,.T.);
#14163=ORIENTED_EDGE('',*,*,#10411,.T.);
#14164=ORIENTED_EDGE('',*,*,#10412,.T.);
#14165=ORIENTED_EDGE('',*,*,#10413,.T.);
#14166=ORIENTED_EDGE('',*,*,#10414,.T.);
#14167=ORIENTED_EDGE('',*,*,#10415,.T.);
#14168=ORIENTED_EDGE('',*,*,#10416,.T.);
#14169=ORIENTED_EDGE('',*,*,#10417,.T.);
#14170=ORIENTED_EDGE('',*,*,#10418,.T.);
#14171=ORIENTED_EDGE('',*,*,#10419,.T.);
#14172=ORIENTED_EDGE('',*,*,#10420,.T.);
#14173=ORIENTED_EDGE('',*,*,#10421,.T.);
#14174=ORIENTED_EDGE('',*,*,#10422,.T.);
#14175=ORIENTED_EDGE('',*,*,#10255,.T.);
#14176=ORIENTED_EDGE('',*,*,#10259,.T.);
#14177=ORIENTED_EDGE('',*,*,#10262,.T.);
#14178=ORIENTED_EDGE('',*,*,#10423,.T.);
#14179=ORIENTED_EDGE('',*,*,#10256,.T.);
#14180=ORIENTED_EDGE('',*,*,#10423,.F.);
#14181=ORIENTED_EDGE('',*,*,#10261,.T.);
#14182=ORIENTED_EDGE('',*,*,#10424,.F.);
#14183=ORIENTED_EDGE('',*,*,#10425,.F.);
#14184=ORIENTED_EDGE('',*,*,#10426,.T.);
#14185=ORIENTED_EDGE('',*,*,#10427,.F.);
#14186=ORIENTED_EDGE('',*,*,#10426,.F.);
#14187=ORIENTED_EDGE('',*,*,#10425,.T.);
#14188=ORIENTED_EDGE('',*,*,#10253,.T.);
#14189=ORIENTED_EDGE('',*,*,#10424,.T.);
#14190=ORIENTED_EDGE('',*,*,#10260,.T.);
#14191=ORIENTED_EDGE('',*,*,#10257,.T.);
#14192=ORIENTED_EDGE('',*,*,#10428,.F.);
#14193=ORIENTED_EDGE('',*,*,#10429,.F.);
#14194=ORIENTED_EDGE('',*,*,#10430,.F.);
#14195=ORIENTED_EDGE('',*,*,#10420,.F.);
#14196=ORIENTED_EDGE('',*,*,#10431,.F.);
#14197=ORIENTED_EDGE('',*,*,#10422,.F.);
#14198=ORIENTED_EDGE('',*,*,#10432,.T.);
#14199=ORIENTED_EDGE('',*,*,#10433,.F.);
#14200=ORIENTED_EDGE('',*,*,#10430,.T.);
#14201=ORIENTED_EDGE('',*,*,#10434,.F.);
#14202=ORIENTED_EDGE('',*,*,#10432,.F.);
#14203=ORIENTED_EDGE('',*,*,#10421,.F.);
#14204=ORIENTED_EDGE('',*,*,#10431,.T.);
#14205=ORIENTED_EDGE('',*,*,#10435,.F.);
#14206=ORIENTED_EDGE('',*,*,#10436,.T.);
#14207=ORIENTED_EDGE('',*,*,#10263,.F.);
#14208=ORIENTED_EDGE('',*,*,#10436,.F.);
#14209=ORIENTED_EDGE('',*,*,#10437,.F.);
#14210=ORIENTED_EDGE('',*,*,#10438,.F.);
#14211=ORIENTED_EDGE('',*,*,#10264,.F.);
#14212=ORIENTED_EDGE('',*,*,#10439,.F.);
#14213=ORIENTED_EDGE('',*,*,#10266,.F.);
#14214=ORIENTED_EDGE('',*,*,#10440,.T.);
#14215=ORIENTED_EDGE('',*,*,#10441,.F.);
#14216=ORIENTED_EDGE('',*,*,#10438,.T.);
#14217=ORIENTED_EDGE('',*,*,#10442,.F.);
#14218=ORIENTED_EDGE('',*,*,#10440,.F.);
#14219=ORIENTED_EDGE('',*,*,#10265,.F.);
#14220=ORIENTED_EDGE('',*,*,#10439,.T.);
#14221=ORIENTED_EDGE('',*,*,#10443,.F.);
#14222=ORIENTED_EDGE('',*,*,#10444,.T.);
#14223=ORIENTED_EDGE('',*,*,#10267,.F.);
#14224=ORIENTED_EDGE('',*,*,#10444,.F.);
#14225=ORIENTED_EDGE('',*,*,#10445,.F.);
#14226=ORIENTED_EDGE('',*,*,#10446,.F.);
#14227=ORIENTED_EDGE('',*,*,#10268,.F.);
#14228=ORIENTED_EDGE('',*,*,#10447,.F.);
#14229=ORIENTED_EDGE('',*,*,#10270,.F.);
#14230=ORIENTED_EDGE('',*,*,#10448,.T.);
#14231=ORIENTED_EDGE('',*,*,#10449,.F.);
#14232=ORIENTED_EDGE('',*,*,#10446,.T.);
#14233=ORIENTED_EDGE('',*,*,#10450,.F.);
#14234=ORIENTED_EDGE('',*,*,#10448,.F.);
#14235=ORIENTED_EDGE('',*,*,#10269,.F.);
#14236=ORIENTED_EDGE('',*,*,#10447,.T.);
#14237=ORIENTED_EDGE('',*,*,#10451,.F.);
#14238=ORIENTED_EDGE('',*,*,#10452,.T.);
#14239=ORIENTED_EDGE('',*,*,#10271,.F.);
#14240=ORIENTED_EDGE('',*,*,#10452,.F.);
#14241=ORIENTED_EDGE('',*,*,#10453,.F.);
#14242=ORIENTED_EDGE('',*,*,#10454,.F.);
#14243=ORIENTED_EDGE('',*,*,#10272,.F.);
#14244=ORIENTED_EDGE('',*,*,#10455,.F.);
#14245=ORIENTED_EDGE('',*,*,#10274,.F.);
#14246=ORIENTED_EDGE('',*,*,#10456,.T.);
#14247=ORIENTED_EDGE('',*,*,#10457,.F.);
#14248=ORIENTED_EDGE('',*,*,#10454,.T.);
#14249=ORIENTED_EDGE('',*,*,#10458,.F.);
#14250=ORIENTED_EDGE('',*,*,#10456,.F.);
#14251=ORIENTED_EDGE('',*,*,#10273,.F.);
#14252=ORIENTED_EDGE('',*,*,#10455,.T.);
#14253=ORIENTED_EDGE('',*,*,#10459,.F.);
#14254=ORIENTED_EDGE('',*,*,#10460,.T.);
#14255=ORIENTED_EDGE('',*,*,#10275,.F.);
#14256=ORIENTED_EDGE('',*,*,#10460,.F.);
#14257=ORIENTED_EDGE('',*,*,#10461,.F.);
#14258=ORIENTED_EDGE('',*,*,#10462,.F.);
#14259=ORIENTED_EDGE('',*,*,#10276,.F.);
#14260=ORIENTED_EDGE('',*,*,#10463,.F.);
#14261=ORIENTED_EDGE('',*,*,#10278,.F.);
#14262=ORIENTED_EDGE('',*,*,#10464,.T.);
#14263=ORIENTED_EDGE('',*,*,#10465,.F.);
#14264=ORIENTED_EDGE('',*,*,#10462,.T.);
#14265=ORIENTED_EDGE('',*,*,#10466,.F.);
#14266=ORIENTED_EDGE('',*,*,#10464,.F.);
#14267=ORIENTED_EDGE('',*,*,#10277,.F.);
#14268=ORIENTED_EDGE('',*,*,#10463,.T.);
#14269=ORIENTED_EDGE('',*,*,#10467,.F.);
#14270=ORIENTED_EDGE('',*,*,#10468,.T.);
#14271=ORIENTED_EDGE('',*,*,#10279,.F.);
#14272=ORIENTED_EDGE('',*,*,#10468,.F.);
#14273=ORIENTED_EDGE('',*,*,#10469,.F.);
#14274=ORIENTED_EDGE('',*,*,#10470,.F.);
#14275=ORIENTED_EDGE('',*,*,#10280,.F.);
#14276=ORIENTED_EDGE('',*,*,#10471,.F.);
#14277=ORIENTED_EDGE('',*,*,#10282,.F.);
#14278=ORIENTED_EDGE('',*,*,#10472,.T.);
#14279=ORIENTED_EDGE('',*,*,#10473,.F.);
#14280=ORIENTED_EDGE('',*,*,#10470,.T.);
#14281=ORIENTED_EDGE('',*,*,#10474,.F.);
#14282=ORIENTED_EDGE('',*,*,#10472,.F.);
#14283=ORIENTED_EDGE('',*,*,#10281,.F.);
#14284=ORIENTED_EDGE('',*,*,#10471,.T.);
#14285=ORIENTED_EDGE('',*,*,#10475,.F.);
#14286=ORIENTED_EDGE('',*,*,#10476,.T.);
#14287=ORIENTED_EDGE('',*,*,#10283,.F.);
#14288=ORIENTED_EDGE('',*,*,#10476,.F.);
#14289=ORIENTED_EDGE('',*,*,#10477,.F.);
#14290=ORIENTED_EDGE('',*,*,#10478,.F.);
#14291=ORIENTED_EDGE('',*,*,#10284,.F.);
#14292=ORIENTED_EDGE('',*,*,#10479,.F.);
#14293=ORIENTED_EDGE('',*,*,#10286,.F.);
#14294=ORIENTED_EDGE('',*,*,#10480,.T.);
#14295=ORIENTED_EDGE('',*,*,#10481,.F.);
#14296=ORIENTED_EDGE('',*,*,#10478,.T.);
#14297=ORIENTED_EDGE('',*,*,#10482,.F.);
#14298=ORIENTED_EDGE('',*,*,#10480,.F.);
#14299=ORIENTED_EDGE('',*,*,#10285,.F.);
#14300=ORIENTED_EDGE('',*,*,#10479,.T.);
#14301=ORIENTED_EDGE('',*,*,#10483,.F.);
#14302=ORIENTED_EDGE('',*,*,#10484,.T.);
#14303=ORIENTED_EDGE('',*,*,#10287,.F.);
#14304=ORIENTED_EDGE('',*,*,#10484,.F.);
#14305=ORIENTED_EDGE('',*,*,#10485,.F.);
#14306=ORIENTED_EDGE('',*,*,#10486,.F.);
#14307=ORIENTED_EDGE('',*,*,#10288,.F.);
#14308=ORIENTED_EDGE('',*,*,#10487,.F.);
#14309=ORIENTED_EDGE('',*,*,#10290,.F.);
#14310=ORIENTED_EDGE('',*,*,#10488,.T.);
#14311=ORIENTED_EDGE('',*,*,#10489,.F.);
#14312=ORIENTED_EDGE('',*,*,#10486,.T.);
#14313=ORIENTED_EDGE('',*,*,#10490,.F.);
#14314=ORIENTED_EDGE('',*,*,#10488,.F.);
#14315=ORIENTED_EDGE('',*,*,#10289,.F.);
#14316=ORIENTED_EDGE('',*,*,#10487,.T.);
#14317=ORIENTED_EDGE('',*,*,#10491,.F.);
#14318=ORIENTED_EDGE('',*,*,#10492,.T.);
#14319=ORIENTED_EDGE('',*,*,#10291,.F.);
#14320=ORIENTED_EDGE('',*,*,#10492,.F.);
#14321=ORIENTED_EDGE('',*,*,#10493,.F.);
#14322=ORIENTED_EDGE('',*,*,#10494,.F.);
#14323=ORIENTED_EDGE('',*,*,#10292,.F.);
#14324=ORIENTED_EDGE('',*,*,#10495,.F.);
#14325=ORIENTED_EDGE('',*,*,#10294,.F.);
#14326=ORIENTED_EDGE('',*,*,#10496,.T.);
#14327=ORIENTED_EDGE('',*,*,#10497,.F.);
#14328=ORIENTED_EDGE('',*,*,#10494,.T.);
#14329=ORIENTED_EDGE('',*,*,#10498,.F.);
#14330=ORIENTED_EDGE('',*,*,#10496,.F.);
#14331=ORIENTED_EDGE('',*,*,#10293,.F.);
#14332=ORIENTED_EDGE('',*,*,#10495,.T.);
#14333=ORIENTED_EDGE('',*,*,#10499,.F.);
#14334=ORIENTED_EDGE('',*,*,#10500,.T.);
#14335=ORIENTED_EDGE('',*,*,#10295,.F.);
#14336=ORIENTED_EDGE('',*,*,#10500,.F.);
#14337=ORIENTED_EDGE('',*,*,#10501,.F.);
#14338=ORIENTED_EDGE('',*,*,#10502,.F.);
#14339=ORIENTED_EDGE('',*,*,#10296,.F.);
#14340=ORIENTED_EDGE('',*,*,#10503,.F.);
#14341=ORIENTED_EDGE('',*,*,#10298,.F.);
#14342=ORIENTED_EDGE('',*,*,#10504,.T.);
#14343=ORIENTED_EDGE('',*,*,#10505,.F.);
#14344=ORIENTED_EDGE('',*,*,#10502,.T.);
#14345=ORIENTED_EDGE('',*,*,#10506,.F.);
#14346=ORIENTED_EDGE('',*,*,#10504,.F.);
#14347=ORIENTED_EDGE('',*,*,#10297,.F.);
#14348=ORIENTED_EDGE('',*,*,#10503,.T.);
#14349=ORIENTED_EDGE('',*,*,#10507,.F.);
#14350=ORIENTED_EDGE('',*,*,#10508,.T.);
#14351=ORIENTED_EDGE('',*,*,#10299,.F.);
#14352=ORIENTED_EDGE('',*,*,#10508,.F.);
#14353=ORIENTED_EDGE('',*,*,#10509,.F.);
#14354=ORIENTED_EDGE('',*,*,#10510,.F.);
#14355=ORIENTED_EDGE('',*,*,#10300,.F.);
#14356=ORIENTED_EDGE('',*,*,#10511,.F.);
#14357=ORIENTED_EDGE('',*,*,#10302,.F.);
#14358=ORIENTED_EDGE('',*,*,#10512,.T.);
#14359=ORIENTED_EDGE('',*,*,#10513,.F.);
#14360=ORIENTED_EDGE('',*,*,#10510,.T.);
#14361=ORIENTED_EDGE('',*,*,#10514,.F.);
#14362=ORIENTED_EDGE('',*,*,#10512,.F.);
#14363=ORIENTED_EDGE('',*,*,#10301,.F.);
#14364=ORIENTED_EDGE('',*,*,#10511,.T.);
#14365=ORIENTED_EDGE('',*,*,#10515,.F.);
#14366=ORIENTED_EDGE('',*,*,#10516,.T.);
#14367=ORIENTED_EDGE('',*,*,#10303,.F.);
#14368=ORIENTED_EDGE('',*,*,#10516,.F.);
#14369=ORIENTED_EDGE('',*,*,#10517,.F.);
#14370=ORIENTED_EDGE('',*,*,#10518,.F.);
#14371=ORIENTED_EDGE('',*,*,#10304,.F.);
#14372=ORIENTED_EDGE('',*,*,#10519,.F.);
#14373=ORIENTED_EDGE('',*,*,#10306,.F.);
#14374=ORIENTED_EDGE('',*,*,#10520,.T.);
#14375=ORIENTED_EDGE('',*,*,#10521,.F.);
#14376=ORIENTED_EDGE('',*,*,#10518,.T.);
#14377=ORIENTED_EDGE('',*,*,#10522,.F.);
#14378=ORIENTED_EDGE('',*,*,#10520,.F.);
#14379=ORIENTED_EDGE('',*,*,#10305,.F.);
#14380=ORIENTED_EDGE('',*,*,#10519,.T.);
#14381=ORIENTED_EDGE('',*,*,#10523,.F.);
#14382=ORIENTED_EDGE('',*,*,#10524,.T.);
#14383=ORIENTED_EDGE('',*,*,#10307,.F.);
#14384=ORIENTED_EDGE('',*,*,#10524,.F.);
#14385=ORIENTED_EDGE('',*,*,#10525,.F.);
#14386=ORIENTED_EDGE('',*,*,#10526,.F.);
#14387=ORIENTED_EDGE('',*,*,#10308,.F.);
#14388=ORIENTED_EDGE('',*,*,#10527,.F.);
#14389=ORIENTED_EDGE('',*,*,#10310,.F.);
#14390=ORIENTED_EDGE('',*,*,#10528,.T.);
#14391=ORIENTED_EDGE('',*,*,#10529,.F.);
#14392=ORIENTED_EDGE('',*,*,#10526,.T.);
#14393=ORIENTED_EDGE('',*,*,#10530,.F.);
#14394=ORIENTED_EDGE('',*,*,#10528,.F.);
#14395=ORIENTED_EDGE('',*,*,#10309,.F.);
#14396=ORIENTED_EDGE('',*,*,#10527,.T.);
#14397=ORIENTED_EDGE('',*,*,#10531,.F.);
#14398=ORIENTED_EDGE('',*,*,#10532,.T.);
#14399=ORIENTED_EDGE('',*,*,#10311,.F.);
#14400=ORIENTED_EDGE('',*,*,#10532,.F.);
#14401=ORIENTED_EDGE('',*,*,#10533,.F.);
#14402=ORIENTED_EDGE('',*,*,#10534,.F.);
#14403=ORIENTED_EDGE('',*,*,#10312,.F.);
#14404=ORIENTED_EDGE('',*,*,#10535,.F.);
#14405=ORIENTED_EDGE('',*,*,#10314,.F.);
#14406=ORIENTED_EDGE('',*,*,#10536,.T.);
#14407=ORIENTED_EDGE('',*,*,#10537,.F.);
#14408=ORIENTED_EDGE('',*,*,#10534,.T.);
#14409=ORIENTED_EDGE('',*,*,#10538,.F.);
#14410=ORIENTED_EDGE('',*,*,#10536,.F.);
#14411=ORIENTED_EDGE('',*,*,#10313,.F.);
#14412=ORIENTED_EDGE('',*,*,#10535,.T.);
#14413=ORIENTED_EDGE('',*,*,#10539,.F.);
#14414=ORIENTED_EDGE('',*,*,#10540,.T.);
#14415=ORIENTED_EDGE('',*,*,#10315,.F.);
#14416=ORIENTED_EDGE('',*,*,#10540,.F.);
#14417=ORIENTED_EDGE('',*,*,#10541,.F.);
#14418=ORIENTED_EDGE('',*,*,#10542,.F.);
#14419=ORIENTED_EDGE('',*,*,#10316,.F.);
#14420=ORIENTED_EDGE('',*,*,#10543,.F.);
#14421=ORIENTED_EDGE('',*,*,#10318,.F.);
#14422=ORIENTED_EDGE('',*,*,#10544,.T.);
#14423=ORIENTED_EDGE('',*,*,#10545,.F.);
#14424=ORIENTED_EDGE('',*,*,#10542,.T.);
#14425=ORIENTED_EDGE('',*,*,#10546,.F.);
#14426=ORIENTED_EDGE('',*,*,#10544,.F.);
#14427=ORIENTED_EDGE('',*,*,#10317,.F.);
#14428=ORIENTED_EDGE('',*,*,#10543,.T.);
#14429=ORIENTED_EDGE('',*,*,#10547,.F.);
#14430=ORIENTED_EDGE('',*,*,#10548,.T.);
#14431=ORIENTED_EDGE('',*,*,#10319,.F.);
#14432=ORIENTED_EDGE('',*,*,#10548,.F.);
#14433=ORIENTED_EDGE('',*,*,#10549,.F.);
#14434=ORIENTED_EDGE('',*,*,#10550,.F.);
#14435=ORIENTED_EDGE('',*,*,#10320,.F.);
#14436=ORIENTED_EDGE('',*,*,#10551,.F.);
#14437=ORIENTED_EDGE('',*,*,#10322,.F.);
#14438=ORIENTED_EDGE('',*,*,#10552,.T.);
#14439=ORIENTED_EDGE('',*,*,#10553,.F.);
#14440=ORIENTED_EDGE('',*,*,#10550,.T.);
#14441=ORIENTED_EDGE('',*,*,#10554,.F.);
#14442=ORIENTED_EDGE('',*,*,#10552,.F.);
#14443=ORIENTED_EDGE('',*,*,#10321,.F.);
#14444=ORIENTED_EDGE('',*,*,#10551,.T.);
#14445=ORIENTED_EDGE('',*,*,#10555,.F.);
#14446=ORIENTED_EDGE('',*,*,#10556,.T.);
#14447=ORIENTED_EDGE('',*,*,#10323,.F.);
#14448=ORIENTED_EDGE('',*,*,#10556,.F.);
#14449=ORIENTED_EDGE('',*,*,#10557,.F.);
#14450=ORIENTED_EDGE('',*,*,#10558,.F.);
#14451=ORIENTED_EDGE('',*,*,#10324,.F.);
#14452=ORIENTED_EDGE('',*,*,#10559,.F.);
#14453=ORIENTED_EDGE('',*,*,#10326,.F.);
#14454=ORIENTED_EDGE('',*,*,#10560,.T.);
#14455=ORIENTED_EDGE('',*,*,#10561,.F.);
#14456=ORIENTED_EDGE('',*,*,#10558,.T.);
#14457=ORIENTED_EDGE('',*,*,#10562,.F.);
#14458=ORIENTED_EDGE('',*,*,#10560,.F.);
#14459=ORIENTED_EDGE('',*,*,#10325,.F.);
#14460=ORIENTED_EDGE('',*,*,#10559,.T.);
#14461=ORIENTED_EDGE('',*,*,#10563,.F.);
#14462=ORIENTED_EDGE('',*,*,#10564,.T.);
#14463=ORIENTED_EDGE('',*,*,#10327,.F.);
#14464=ORIENTED_EDGE('',*,*,#10564,.F.);
#14465=ORIENTED_EDGE('',*,*,#10565,.F.);
#14466=ORIENTED_EDGE('',*,*,#10566,.F.);
#14467=ORIENTED_EDGE('',*,*,#10328,.F.);
#14468=ORIENTED_EDGE('',*,*,#10567,.F.);
#14469=ORIENTED_EDGE('',*,*,#10330,.F.);
#14470=ORIENTED_EDGE('',*,*,#10568,.T.);
#14471=ORIENTED_EDGE('',*,*,#10569,.F.);
#14472=ORIENTED_EDGE('',*,*,#10566,.T.);
#14473=ORIENTED_EDGE('',*,*,#10570,.F.);
#14474=ORIENTED_EDGE('',*,*,#10568,.F.);
#14475=ORIENTED_EDGE('',*,*,#10329,.F.);
#14476=ORIENTED_EDGE('',*,*,#10567,.T.);
#14477=ORIENTED_EDGE('',*,*,#10571,.F.);
#14478=ORIENTED_EDGE('',*,*,#10572,.T.);
#14479=ORIENTED_EDGE('',*,*,#10331,.F.);
#14480=ORIENTED_EDGE('',*,*,#10572,.F.);
#14481=ORIENTED_EDGE('',*,*,#10573,.F.);
#14482=ORIENTED_EDGE('',*,*,#10574,.F.);
#14483=ORIENTED_EDGE('',*,*,#10332,.F.);
#14484=ORIENTED_EDGE('',*,*,#10575,.F.);
#14485=ORIENTED_EDGE('',*,*,#10334,.F.);
#14486=ORIENTED_EDGE('',*,*,#10576,.T.);
#14487=ORIENTED_EDGE('',*,*,#10577,.F.);
#14488=ORIENTED_EDGE('',*,*,#10574,.T.);
#14489=ORIENTED_EDGE('',*,*,#10578,.F.);
#14490=ORIENTED_EDGE('',*,*,#10576,.F.);
#14491=ORIENTED_EDGE('',*,*,#10333,.F.);
#14492=ORIENTED_EDGE('',*,*,#10575,.T.);
#14493=ORIENTED_EDGE('',*,*,#10579,.F.);
#14494=ORIENTED_EDGE('',*,*,#10580,.T.);
#14495=ORIENTED_EDGE('',*,*,#10335,.F.);
#14496=ORIENTED_EDGE('',*,*,#10580,.F.);
#14497=ORIENTED_EDGE('',*,*,#10581,.F.);
#14498=ORIENTED_EDGE('',*,*,#10582,.F.);
#14499=ORIENTED_EDGE('',*,*,#10336,.F.);
#14500=ORIENTED_EDGE('',*,*,#10583,.F.);
#14501=ORIENTED_EDGE('',*,*,#10338,.F.);
#14502=ORIENTED_EDGE('',*,*,#10584,.T.);
#14503=ORIENTED_EDGE('',*,*,#10585,.F.);
#14504=ORIENTED_EDGE('',*,*,#10582,.T.);
#14505=ORIENTED_EDGE('',*,*,#10586,.F.);
#14506=ORIENTED_EDGE('',*,*,#10584,.F.);
#14507=ORIENTED_EDGE('',*,*,#10337,.F.);
#14508=ORIENTED_EDGE('',*,*,#10583,.T.);
#14509=ORIENTED_EDGE('',*,*,#10587,.F.);
#14510=ORIENTED_EDGE('',*,*,#10588,.T.);
#14511=ORIENTED_EDGE('',*,*,#10339,.F.);
#14512=ORIENTED_EDGE('',*,*,#10588,.F.);
#14513=ORIENTED_EDGE('',*,*,#10589,.F.);
#14514=ORIENTED_EDGE('',*,*,#10590,.F.);
#14515=ORIENTED_EDGE('',*,*,#10340,.F.);
#14516=ORIENTED_EDGE('',*,*,#10591,.F.);
#14517=ORIENTED_EDGE('',*,*,#10342,.F.);
#14518=ORIENTED_EDGE('',*,*,#10592,.T.);
#14519=ORIENTED_EDGE('',*,*,#10593,.F.);
#14520=ORIENTED_EDGE('',*,*,#10590,.T.);
#14521=ORIENTED_EDGE('',*,*,#10594,.F.);
#14522=ORIENTED_EDGE('',*,*,#10592,.F.);
#14523=ORIENTED_EDGE('',*,*,#10341,.F.);
#14524=ORIENTED_EDGE('',*,*,#10591,.T.);
#14525=ORIENTED_EDGE('',*,*,#10595,.F.);
#14526=ORIENTED_EDGE('',*,*,#10596,.T.);
#14527=ORIENTED_EDGE('',*,*,#10343,.F.);
#14528=ORIENTED_EDGE('',*,*,#10596,.F.);
#14529=ORIENTED_EDGE('',*,*,#10597,.F.);
#14530=ORIENTED_EDGE('',*,*,#10598,.F.);
#14531=ORIENTED_EDGE('',*,*,#10344,.F.);
#14532=ORIENTED_EDGE('',*,*,#10599,.F.);
#14533=ORIENTED_EDGE('',*,*,#10346,.F.);
#14534=ORIENTED_EDGE('',*,*,#10600,.T.);
#14535=ORIENTED_EDGE('',*,*,#10601,.F.);
#14536=ORIENTED_EDGE('',*,*,#10598,.T.);
#14537=ORIENTED_EDGE('',*,*,#10602,.F.);
#14538=ORIENTED_EDGE('',*,*,#10600,.F.);
#14539=ORIENTED_EDGE('',*,*,#10345,.F.);
#14540=ORIENTED_EDGE('',*,*,#10599,.T.);
#14541=ORIENTED_EDGE('',*,*,#10603,.F.);
#14542=ORIENTED_EDGE('',*,*,#10604,.T.);
#14543=ORIENTED_EDGE('',*,*,#10347,.F.);
#14544=ORIENTED_EDGE('',*,*,#10604,.F.);
#14545=ORIENTED_EDGE('',*,*,#10605,.F.);
#14546=ORIENTED_EDGE('',*,*,#10606,.F.);
#14547=ORIENTED_EDGE('',*,*,#10348,.F.);
#14548=ORIENTED_EDGE('',*,*,#10607,.F.);
#14549=ORIENTED_EDGE('',*,*,#10350,.F.);
#14550=ORIENTED_EDGE('',*,*,#10608,.T.);
#14551=ORIENTED_EDGE('',*,*,#10609,.F.);
#14552=ORIENTED_EDGE('',*,*,#10606,.T.);
#14553=ORIENTED_EDGE('',*,*,#10610,.F.);
#14554=ORIENTED_EDGE('',*,*,#10608,.F.);
#14555=ORIENTED_EDGE('',*,*,#10349,.F.);
#14556=ORIENTED_EDGE('',*,*,#10607,.T.);
#14557=ORIENTED_EDGE('',*,*,#10611,.F.);
#14558=ORIENTED_EDGE('',*,*,#10612,.T.);
#14559=ORIENTED_EDGE('',*,*,#10351,.F.);
#14560=ORIENTED_EDGE('',*,*,#10612,.F.);
#14561=ORIENTED_EDGE('',*,*,#10613,.F.);
#14562=ORIENTED_EDGE('',*,*,#10614,.F.);
#14563=ORIENTED_EDGE('',*,*,#10352,.F.);
#14564=ORIENTED_EDGE('',*,*,#10615,.F.);
#14565=ORIENTED_EDGE('',*,*,#10354,.F.);
#14566=ORIENTED_EDGE('',*,*,#10616,.T.);
#14567=ORIENTED_EDGE('',*,*,#10617,.F.);
#14568=ORIENTED_EDGE('',*,*,#10614,.T.);
#14569=ORIENTED_EDGE('',*,*,#10618,.F.);
#14570=ORIENTED_EDGE('',*,*,#10616,.F.);
#14571=ORIENTED_EDGE('',*,*,#10353,.F.);
#14572=ORIENTED_EDGE('',*,*,#10615,.T.);
#14573=ORIENTED_EDGE('',*,*,#10619,.F.);
#14574=ORIENTED_EDGE('',*,*,#10620,.T.);
#14575=ORIENTED_EDGE('',*,*,#10355,.F.);
#14576=ORIENTED_EDGE('',*,*,#10620,.F.);
#14577=ORIENTED_EDGE('',*,*,#10621,.F.);
#14578=ORIENTED_EDGE('',*,*,#10622,.F.);
#14579=ORIENTED_EDGE('',*,*,#10356,.F.);
#14580=ORIENTED_EDGE('',*,*,#10623,.F.);
#14581=ORIENTED_EDGE('',*,*,#10358,.F.);
#14582=ORIENTED_EDGE('',*,*,#10624,.T.);
#14583=ORIENTED_EDGE('',*,*,#10625,.F.);
#14584=ORIENTED_EDGE('',*,*,#10622,.T.);
#14585=ORIENTED_EDGE('',*,*,#10626,.F.);
#14586=ORIENTED_EDGE('',*,*,#10624,.F.);
#14587=ORIENTED_EDGE('',*,*,#10357,.F.);
#14588=ORIENTED_EDGE('',*,*,#10623,.T.);
#14589=ORIENTED_EDGE('',*,*,#10627,.F.);
#14590=ORIENTED_EDGE('',*,*,#10628,.T.);
#14591=ORIENTED_EDGE('',*,*,#10359,.F.);
#14592=ORIENTED_EDGE('',*,*,#10628,.F.);
#14593=ORIENTED_EDGE('',*,*,#10629,.F.);
#14594=ORIENTED_EDGE('',*,*,#10630,.F.);
#14595=ORIENTED_EDGE('',*,*,#10360,.F.);
#14596=ORIENTED_EDGE('',*,*,#10631,.F.);
#14597=ORIENTED_EDGE('',*,*,#10362,.F.);
#14598=ORIENTED_EDGE('',*,*,#10632,.T.);
#14599=ORIENTED_EDGE('',*,*,#10633,.F.);
#14600=ORIENTED_EDGE('',*,*,#10630,.T.);
#14601=ORIENTED_EDGE('',*,*,#10634,.F.);
#14602=ORIENTED_EDGE('',*,*,#10632,.F.);
#14603=ORIENTED_EDGE('',*,*,#10361,.F.);
#14604=ORIENTED_EDGE('',*,*,#10631,.T.);
#14605=ORIENTED_EDGE('',*,*,#10635,.F.);
#14606=ORIENTED_EDGE('',*,*,#10636,.T.);
#14607=ORIENTED_EDGE('',*,*,#10363,.F.);
#14608=ORIENTED_EDGE('',*,*,#10636,.F.);
#14609=ORIENTED_EDGE('',*,*,#10637,.F.);
#14610=ORIENTED_EDGE('',*,*,#10638,.F.);
#14611=ORIENTED_EDGE('',*,*,#10364,.F.);
#14612=ORIENTED_EDGE('',*,*,#10639,.F.);
#14613=ORIENTED_EDGE('',*,*,#10366,.F.);
#14614=ORIENTED_EDGE('',*,*,#10640,.T.);
#14615=ORIENTED_EDGE('',*,*,#10641,.F.);
#14616=ORIENTED_EDGE('',*,*,#10638,.T.);
#14617=ORIENTED_EDGE('',*,*,#10642,.F.);
#14618=ORIENTED_EDGE('',*,*,#10640,.F.);
#14619=ORIENTED_EDGE('',*,*,#10365,.F.);
#14620=ORIENTED_EDGE('',*,*,#10639,.T.);
#14621=ORIENTED_EDGE('',*,*,#10643,.F.);
#14622=ORIENTED_EDGE('',*,*,#10644,.T.);
#14623=ORIENTED_EDGE('',*,*,#10367,.F.);
#14624=ORIENTED_EDGE('',*,*,#10644,.F.);
#14625=ORIENTED_EDGE('',*,*,#10645,.F.);
#14626=ORIENTED_EDGE('',*,*,#10646,.F.);
#14627=ORIENTED_EDGE('',*,*,#10368,.F.);
#14628=ORIENTED_EDGE('',*,*,#10647,.F.);
#14629=ORIENTED_EDGE('',*,*,#10370,.F.);
#14630=ORIENTED_EDGE('',*,*,#10648,.T.);
#14631=ORIENTED_EDGE('',*,*,#10649,.F.);
#14632=ORIENTED_EDGE('',*,*,#10646,.T.);
#14633=ORIENTED_EDGE('',*,*,#10650,.F.);
#14634=ORIENTED_EDGE('',*,*,#10648,.F.);
#14635=ORIENTED_EDGE('',*,*,#10369,.F.);
#14636=ORIENTED_EDGE('',*,*,#10647,.T.);
#14637=ORIENTED_EDGE('',*,*,#10651,.F.);
#14638=ORIENTED_EDGE('',*,*,#10652,.T.);
#14639=ORIENTED_EDGE('',*,*,#10371,.F.);
#14640=ORIENTED_EDGE('',*,*,#10652,.F.);
#14641=ORIENTED_EDGE('',*,*,#10653,.F.);
#14642=ORIENTED_EDGE('',*,*,#10654,.F.);
#14643=ORIENTED_EDGE('',*,*,#10372,.F.);
#14644=ORIENTED_EDGE('',*,*,#10655,.F.);
#14645=ORIENTED_EDGE('',*,*,#10374,.F.);
#14646=ORIENTED_EDGE('',*,*,#10656,.T.);
#14647=ORIENTED_EDGE('',*,*,#10657,.F.);
#14648=ORIENTED_EDGE('',*,*,#10654,.T.);
#14649=ORIENTED_EDGE('',*,*,#10658,.F.);
#14650=ORIENTED_EDGE('',*,*,#10656,.F.);
#14651=ORIENTED_EDGE('',*,*,#10373,.F.);
#14652=ORIENTED_EDGE('',*,*,#10655,.T.);
#14653=ORIENTED_EDGE('',*,*,#10659,.F.);
#14654=ORIENTED_EDGE('',*,*,#10660,.T.);
#14655=ORIENTED_EDGE('',*,*,#10375,.F.);
#14656=ORIENTED_EDGE('',*,*,#10660,.F.);
#14657=ORIENTED_EDGE('',*,*,#10661,.F.);
#14658=ORIENTED_EDGE('',*,*,#10662,.F.);
#14659=ORIENTED_EDGE('',*,*,#10376,.F.);
#14660=ORIENTED_EDGE('',*,*,#10663,.F.);
#14661=ORIENTED_EDGE('',*,*,#10378,.F.);
#14662=ORIENTED_EDGE('',*,*,#10664,.T.);
#14663=ORIENTED_EDGE('',*,*,#10665,.F.);
#14664=ORIENTED_EDGE('',*,*,#10662,.T.);
#14665=ORIENTED_EDGE('',*,*,#10666,.F.);
#14666=ORIENTED_EDGE('',*,*,#10664,.F.);
#14667=ORIENTED_EDGE('',*,*,#10377,.F.);
#14668=ORIENTED_EDGE('',*,*,#10663,.T.);
#14669=ORIENTED_EDGE('',*,*,#10667,.F.);
#14670=ORIENTED_EDGE('',*,*,#10668,.T.);
#14671=ORIENTED_EDGE('',*,*,#10379,.F.);
#14672=ORIENTED_EDGE('',*,*,#10668,.F.);
#14673=ORIENTED_EDGE('',*,*,#10669,.F.);
#14674=ORIENTED_EDGE('',*,*,#10670,.F.);
#14675=ORIENTED_EDGE('',*,*,#10380,.F.);
#14676=ORIENTED_EDGE('',*,*,#10671,.F.);
#14677=ORIENTED_EDGE('',*,*,#10382,.F.);
#14678=ORIENTED_EDGE('',*,*,#10672,.T.);
#14679=ORIENTED_EDGE('',*,*,#10673,.F.);
#14680=ORIENTED_EDGE('',*,*,#10670,.T.);
#14681=ORIENTED_EDGE('',*,*,#10674,.F.);
#14682=ORIENTED_EDGE('',*,*,#10672,.F.);
#14683=ORIENTED_EDGE('',*,*,#10381,.F.);
#14684=ORIENTED_EDGE('',*,*,#10671,.T.);
#14685=ORIENTED_EDGE('',*,*,#10675,.F.);
#14686=ORIENTED_EDGE('',*,*,#10676,.T.);
#14687=ORIENTED_EDGE('',*,*,#10383,.F.);
#14688=ORIENTED_EDGE('',*,*,#10676,.F.);
#14689=ORIENTED_EDGE('',*,*,#10677,.F.);
#14690=ORIENTED_EDGE('',*,*,#10678,.F.);
#14691=ORIENTED_EDGE('',*,*,#10384,.F.);
#14692=ORIENTED_EDGE('',*,*,#10679,.F.);
#14693=ORIENTED_EDGE('',*,*,#10386,.F.);
#14694=ORIENTED_EDGE('',*,*,#10680,.T.);
#14695=ORIENTED_EDGE('',*,*,#10681,.F.);
#14696=ORIENTED_EDGE('',*,*,#10678,.T.);
#14697=ORIENTED_EDGE('',*,*,#10682,.F.);
#14698=ORIENTED_EDGE('',*,*,#10680,.F.);
#14699=ORIENTED_EDGE('',*,*,#10385,.F.);
#14700=ORIENTED_EDGE('',*,*,#10679,.T.);
#14701=ORIENTED_EDGE('',*,*,#10683,.F.);
#14702=ORIENTED_EDGE('',*,*,#10684,.T.);
#14703=ORIENTED_EDGE('',*,*,#10387,.F.);
#14704=ORIENTED_EDGE('',*,*,#10684,.F.);
#14705=ORIENTED_EDGE('',*,*,#10685,.F.);
#14706=ORIENTED_EDGE('',*,*,#10686,.F.);
#14707=ORIENTED_EDGE('',*,*,#10388,.F.);
#14708=ORIENTED_EDGE('',*,*,#10687,.F.);
#14709=ORIENTED_EDGE('',*,*,#10390,.F.);
#14710=ORIENTED_EDGE('',*,*,#10688,.T.);
#14711=ORIENTED_EDGE('',*,*,#10689,.F.);
#14712=ORIENTED_EDGE('',*,*,#10686,.T.);
#14713=ORIENTED_EDGE('',*,*,#10690,.F.);
#14714=ORIENTED_EDGE('',*,*,#10688,.F.);
#14715=ORIENTED_EDGE('',*,*,#10389,.F.);
#14716=ORIENTED_EDGE('',*,*,#10687,.T.);
#14717=ORIENTED_EDGE('',*,*,#10691,.F.);
#14718=ORIENTED_EDGE('',*,*,#10692,.T.);
#14719=ORIENTED_EDGE('',*,*,#10391,.F.);
#14720=ORIENTED_EDGE('',*,*,#10692,.F.);
#14721=ORIENTED_EDGE('',*,*,#10693,.F.);
#14722=ORIENTED_EDGE('',*,*,#10694,.F.);
#14723=ORIENTED_EDGE('',*,*,#10392,.F.);
#14724=ORIENTED_EDGE('',*,*,#10695,.F.);
#14725=ORIENTED_EDGE('',*,*,#10394,.F.);
#14726=ORIENTED_EDGE('',*,*,#10696,.T.);
#14727=ORIENTED_EDGE('',*,*,#10697,.F.);
#14728=ORIENTED_EDGE('',*,*,#10694,.T.);
#14729=ORIENTED_EDGE('',*,*,#10698,.F.);
#14730=ORIENTED_EDGE('',*,*,#10696,.F.);
#14731=ORIENTED_EDGE('',*,*,#10393,.F.);
#14732=ORIENTED_EDGE('',*,*,#10695,.T.);
#14733=ORIENTED_EDGE('',*,*,#10699,.F.);
#14734=ORIENTED_EDGE('',*,*,#10700,.T.);
#14735=ORIENTED_EDGE('',*,*,#10395,.F.);
#14736=ORIENTED_EDGE('',*,*,#10700,.F.);
#14737=ORIENTED_EDGE('',*,*,#10701,.F.);
#14738=ORIENTED_EDGE('',*,*,#10702,.F.);
#14739=ORIENTED_EDGE('',*,*,#10396,.F.);
#14740=ORIENTED_EDGE('',*,*,#10703,.F.);
#14741=ORIENTED_EDGE('',*,*,#10398,.F.);
#14742=ORIENTED_EDGE('',*,*,#10704,.T.);
#14743=ORIENTED_EDGE('',*,*,#10705,.F.);
#14744=ORIENTED_EDGE('',*,*,#10702,.T.);
#14745=ORIENTED_EDGE('',*,*,#10706,.F.);
#14746=ORIENTED_EDGE('',*,*,#10704,.F.);
#14747=ORIENTED_EDGE('',*,*,#10397,.F.);
#14748=ORIENTED_EDGE('',*,*,#10703,.T.);
#14749=ORIENTED_EDGE('',*,*,#10707,.F.);
#14750=ORIENTED_EDGE('',*,*,#10708,.T.);
#14751=ORIENTED_EDGE('',*,*,#10399,.F.);
#14752=ORIENTED_EDGE('',*,*,#10708,.F.);
#14753=ORIENTED_EDGE('',*,*,#10709,.F.);
#14754=ORIENTED_EDGE('',*,*,#10710,.F.);
#14755=ORIENTED_EDGE('',*,*,#10400,.F.);
#14756=ORIENTED_EDGE('',*,*,#10711,.F.);
#14757=ORIENTED_EDGE('',*,*,#10402,.F.);
#14758=ORIENTED_EDGE('',*,*,#10712,.T.);
#14759=ORIENTED_EDGE('',*,*,#10713,.F.);
#14760=ORIENTED_EDGE('',*,*,#10710,.T.);
#14761=ORIENTED_EDGE('',*,*,#10714,.F.);
#14762=ORIENTED_EDGE('',*,*,#10712,.F.);
#14763=ORIENTED_EDGE('',*,*,#10401,.F.);
#14764=ORIENTED_EDGE('',*,*,#10711,.T.);
#14765=ORIENTED_EDGE('',*,*,#10715,.F.);
#14766=ORIENTED_EDGE('',*,*,#10716,.T.);
#14767=ORIENTED_EDGE('',*,*,#10403,.F.);
#14768=ORIENTED_EDGE('',*,*,#10716,.F.);
#14769=ORIENTED_EDGE('',*,*,#10717,.F.);
#14770=ORIENTED_EDGE('',*,*,#10718,.F.);
#14771=ORIENTED_EDGE('',*,*,#10404,.F.);
#14772=ORIENTED_EDGE('',*,*,#10719,.F.);
#14773=ORIENTED_EDGE('',*,*,#10406,.F.);
#14774=ORIENTED_EDGE('',*,*,#10720,.T.);
#14775=ORIENTED_EDGE('',*,*,#10721,.F.);
#14776=ORIENTED_EDGE('',*,*,#10718,.T.);
#14777=ORIENTED_EDGE('',*,*,#10722,.F.);
#14778=ORIENTED_EDGE('',*,*,#10720,.F.);
#14779=ORIENTED_EDGE('',*,*,#10405,.F.);
#14780=ORIENTED_EDGE('',*,*,#10719,.T.);
#14781=ORIENTED_EDGE('',*,*,#10723,.F.);
#14782=ORIENTED_EDGE('',*,*,#10724,.T.);
#14783=ORIENTED_EDGE('',*,*,#10407,.F.);
#14784=ORIENTED_EDGE('',*,*,#10724,.F.);
#14785=ORIENTED_EDGE('',*,*,#10725,.F.);
#14786=ORIENTED_EDGE('',*,*,#10726,.F.);
#14787=ORIENTED_EDGE('',*,*,#10408,.F.);
#14788=ORIENTED_EDGE('',*,*,#10727,.F.);
#14789=ORIENTED_EDGE('',*,*,#10410,.F.);
#14790=ORIENTED_EDGE('',*,*,#10728,.T.);
#14791=ORIENTED_EDGE('',*,*,#10729,.F.);
#14792=ORIENTED_EDGE('',*,*,#10726,.T.);
#14793=ORIENTED_EDGE('',*,*,#10730,.F.);
#14794=ORIENTED_EDGE('',*,*,#10728,.F.);
#14795=ORIENTED_EDGE('',*,*,#10409,.F.);
#14796=ORIENTED_EDGE('',*,*,#10727,.T.);
#14797=ORIENTED_EDGE('',*,*,#10731,.F.);
#14798=ORIENTED_EDGE('',*,*,#10732,.T.);
#14799=ORIENTED_EDGE('',*,*,#10411,.F.);
#14800=ORIENTED_EDGE('',*,*,#10732,.F.);
#14801=ORIENTED_EDGE('',*,*,#10733,.F.);
#14802=ORIENTED_EDGE('',*,*,#10734,.F.);
#14803=ORIENTED_EDGE('',*,*,#10412,.F.);
#14804=ORIENTED_EDGE('',*,*,#10734,.T.);
#14805=ORIENTED_EDGE('',*,*,#10735,.F.);
#14806=ORIENTED_EDGE('',*,*,#10736,.F.);
#14807=ORIENTED_EDGE('',*,*,#10413,.F.);
#14808=ORIENTED_EDGE('',*,*,#10737,.F.);
#14809=ORIENTED_EDGE('',*,*,#10414,.F.);
#14810=ORIENTED_EDGE('',*,*,#10736,.T.);
#14811=ORIENTED_EDGE('',*,*,#10738,.F.);
#14812=ORIENTED_EDGE('',*,*,#10737,.T.);
#14813=ORIENTED_EDGE('',*,*,#10739,.F.);
#14814=ORIENTED_EDGE('',*,*,#10740,.T.);
#14815=ORIENTED_EDGE('',*,*,#10415,.F.);
#14816=ORIENTED_EDGE('',*,*,#10741,.F.);
#14817=ORIENTED_EDGE('',*,*,#10418,.F.);
#14818=ORIENTED_EDGE('',*,*,#10742,.T.);
#14819=ORIENTED_EDGE('',*,*,#10743,.F.);
#14820=ORIENTED_EDGE('',*,*,#10740,.F.);
#14821=ORIENTED_EDGE('',*,*,#10744,.F.);
#14822=ORIENTED_EDGE('',*,*,#10745,.F.);
#14823=ORIENTED_EDGE('',*,*,#10416,.F.);
#14824=ORIENTED_EDGE('',*,*,#10745,.T.);
#14825=ORIENTED_EDGE('',*,*,#10746,.F.);
#14826=ORIENTED_EDGE('',*,*,#10742,.F.);
#14827=ORIENTED_EDGE('',*,*,#10417,.F.);
#14828=ORIENTED_EDGE('',*,*,#10433,.T.);
#14829=ORIENTED_EDGE('',*,*,#10434,.T.);
#14830=ORIENTED_EDGE('',*,*,#10429,.T.);
#14831=ORIENTED_EDGE('',*,*,#10747,.T.);
#14832=ORIENTED_EDGE('',*,*,#10743,.T.);
#14833=ORIENTED_EDGE('',*,*,#10746,.T.);
#14834=ORIENTED_EDGE('',*,*,#10744,.T.);
#14835=ORIENTED_EDGE('',*,*,#10739,.T.);
#14836=ORIENTED_EDGE('',*,*,#10738,.T.);
#14837=ORIENTED_EDGE('',*,*,#10735,.T.);
#14838=ORIENTED_EDGE('',*,*,#10733,.T.);
#14839=ORIENTED_EDGE('',*,*,#10731,.T.);
#14840=ORIENTED_EDGE('',*,*,#10729,.T.);
#14841=ORIENTED_EDGE('',*,*,#10730,.T.);
#14842=ORIENTED_EDGE('',*,*,#10725,.T.);
#14843=ORIENTED_EDGE('',*,*,#10723,.T.);
#14844=ORIENTED_EDGE('',*,*,#10721,.T.);
#14845=ORIENTED_EDGE('',*,*,#10722,.T.);
#14846=ORIENTED_EDGE('',*,*,#10717,.T.);
#14847=ORIENTED_EDGE('',*,*,#10715,.T.);
#14848=ORIENTED_EDGE('',*,*,#10713,.T.);
#14849=ORIENTED_EDGE('',*,*,#10714,.T.);
#14850=ORIENTED_EDGE('',*,*,#10709,.T.);
#14851=ORIENTED_EDGE('',*,*,#10707,.T.);
#14852=ORIENTED_EDGE('',*,*,#10705,.T.);
#14853=ORIENTED_EDGE('',*,*,#10706,.T.);
#14854=ORIENTED_EDGE('',*,*,#10701,.T.);
#14855=ORIENTED_EDGE('',*,*,#10699,.T.);
#14856=ORIENTED_EDGE('',*,*,#10697,.T.);
#14857=ORIENTED_EDGE('',*,*,#10698,.T.);
#14858=ORIENTED_EDGE('',*,*,#10693,.T.);
#14859=ORIENTED_EDGE('',*,*,#10691,.T.);
#14860=ORIENTED_EDGE('',*,*,#10689,.T.);
#14861=ORIENTED_EDGE('',*,*,#10690,.T.);
#14862=ORIENTED_EDGE('',*,*,#10685,.T.);
#14863=ORIENTED_EDGE('',*,*,#10683,.T.);
#14864=ORIENTED_EDGE('',*,*,#10681,.T.);
#14865=ORIENTED_EDGE('',*,*,#10682,.T.);
#14866=ORIENTED_EDGE('',*,*,#10677,.T.);
#14867=ORIENTED_EDGE('',*,*,#10675,.T.);
#14868=ORIENTED_EDGE('',*,*,#10673,.T.);
#14869=ORIENTED_EDGE('',*,*,#10674,.T.);
#14870=ORIENTED_EDGE('',*,*,#10669,.T.);
#14871=ORIENTED_EDGE('',*,*,#10667,.T.);
#14872=ORIENTED_EDGE('',*,*,#10665,.T.);
#14873=ORIENTED_EDGE('',*,*,#10666,.T.);
#14874=ORIENTED_EDGE('',*,*,#10661,.T.);
#14875=ORIENTED_EDGE('',*,*,#10659,.T.);
#14876=ORIENTED_EDGE('',*,*,#10657,.T.);
#14877=ORIENTED_EDGE('',*,*,#10658,.T.);
#14878=ORIENTED_EDGE('',*,*,#10653,.T.);
#14879=ORIENTED_EDGE('',*,*,#10651,.T.);
#14880=ORIENTED_EDGE('',*,*,#10649,.T.);
#14881=ORIENTED_EDGE('',*,*,#10650,.T.);
#14882=ORIENTED_EDGE('',*,*,#10645,.T.);
#14883=ORIENTED_EDGE('',*,*,#10643,.T.);
#14884=ORIENTED_EDGE('',*,*,#10641,.T.);
#14885=ORIENTED_EDGE('',*,*,#10642,.T.);
#14886=ORIENTED_EDGE('',*,*,#10637,.T.);
#14887=ORIENTED_EDGE('',*,*,#10635,.T.);
#14888=ORIENTED_EDGE('',*,*,#10633,.T.);
#14889=ORIENTED_EDGE('',*,*,#10634,.T.);
#14890=ORIENTED_EDGE('',*,*,#10629,.T.);
#14891=ORIENTED_EDGE('',*,*,#10627,.T.);
#14892=ORIENTED_EDGE('',*,*,#10625,.T.);
#14893=ORIENTED_EDGE('',*,*,#10626,.T.);
#14894=ORIENTED_EDGE('',*,*,#10621,.T.);
#14895=ORIENTED_EDGE('',*,*,#10619,.T.);
#14896=ORIENTED_EDGE('',*,*,#10617,.T.);
#14897=ORIENTED_EDGE('',*,*,#10618,.T.);
#14898=ORIENTED_EDGE('',*,*,#10613,.T.);
#14899=ORIENTED_EDGE('',*,*,#10611,.T.);
#14900=ORIENTED_EDGE('',*,*,#10609,.T.);
#14901=ORIENTED_EDGE('',*,*,#10610,.T.);
#14902=ORIENTED_EDGE('',*,*,#10605,.T.);
#14903=ORIENTED_EDGE('',*,*,#10603,.T.);
#14904=ORIENTED_EDGE('',*,*,#10601,.T.);
#14905=ORIENTED_EDGE('',*,*,#10602,.T.);
#14906=ORIENTED_EDGE('',*,*,#10597,.T.);
#14907=ORIENTED_EDGE('',*,*,#10595,.T.);
#14908=ORIENTED_EDGE('',*,*,#10593,.T.);
#14909=ORIENTED_EDGE('',*,*,#10594,.T.);
#14910=ORIENTED_EDGE('',*,*,#10589,.T.);
#14911=ORIENTED_EDGE('',*,*,#10587,.T.);
#14912=ORIENTED_EDGE('',*,*,#10585,.T.);
#14913=ORIENTED_EDGE('',*,*,#10586,.T.);
#14914=ORIENTED_EDGE('',*,*,#10581,.T.);
#14915=ORIENTED_EDGE('',*,*,#10579,.T.);
#14916=ORIENTED_EDGE('',*,*,#10577,.T.);
#14917=ORIENTED_EDGE('',*,*,#10578,.T.);
#14918=ORIENTED_EDGE('',*,*,#10573,.T.);
#14919=ORIENTED_EDGE('',*,*,#10571,.T.);
#14920=ORIENTED_EDGE('',*,*,#10569,.T.);
#14921=ORIENTED_EDGE('',*,*,#10570,.T.);
#14922=ORIENTED_EDGE('',*,*,#10565,.T.);
#14923=ORIENTED_EDGE('',*,*,#10563,.T.);
#14924=ORIENTED_EDGE('',*,*,#10561,.T.);
#14925=ORIENTED_EDGE('',*,*,#10562,.T.);
#14926=ORIENTED_EDGE('',*,*,#10557,.T.);
#14927=ORIENTED_EDGE('',*,*,#10555,.T.);
#14928=ORIENTED_EDGE('',*,*,#10553,.T.);
#14929=ORIENTED_EDGE('',*,*,#10554,.T.);
#14930=ORIENTED_EDGE('',*,*,#10549,.T.);
#14931=ORIENTED_EDGE('',*,*,#10547,.T.);
#14932=ORIENTED_EDGE('',*,*,#10545,.T.);
#14933=ORIENTED_EDGE('',*,*,#10546,.T.);
#14934=ORIENTED_EDGE('',*,*,#10541,.T.);
#14935=ORIENTED_EDGE('',*,*,#10539,.T.);
#14936=ORIENTED_EDGE('',*,*,#10537,.T.);
#14937=ORIENTED_EDGE('',*,*,#10538,.T.);
#14938=ORIENTED_EDGE('',*,*,#10533,.T.);
#14939=ORIENTED_EDGE('',*,*,#10531,.T.);
#14940=ORIENTED_EDGE('',*,*,#10529,.T.);
#14941=ORIENTED_EDGE('',*,*,#10530,.T.);
#14942=ORIENTED_EDGE('',*,*,#10525,.T.);
#14943=ORIENTED_EDGE('',*,*,#10523,.T.);
#14944=ORIENTED_EDGE('',*,*,#10521,.T.);
#14945=ORIENTED_EDGE('',*,*,#10522,.T.);
#14946=ORIENTED_EDGE('',*,*,#10517,.T.);
#14947=ORIENTED_EDGE('',*,*,#10515,.T.);
#14948=ORIENTED_EDGE('',*,*,#10513,.T.);
#14949=ORIENTED_EDGE('',*,*,#10514,.T.);
#14950=ORIENTED_EDGE('',*,*,#10509,.T.);
#14951=ORIENTED_EDGE('',*,*,#10507,.T.);
#14952=ORIENTED_EDGE('',*,*,#10505,.T.);
#14953=ORIENTED_EDGE('',*,*,#10506,.T.);
#14954=ORIENTED_EDGE('',*,*,#10501,.T.);
#14955=ORIENTED_EDGE('',*,*,#10499,.T.);
#14956=ORIENTED_EDGE('',*,*,#10497,.T.);
#14957=ORIENTED_EDGE('',*,*,#10498,.T.);
#14958=ORIENTED_EDGE('',*,*,#10493,.T.);
#14959=ORIENTED_EDGE('',*,*,#10491,.T.);
#14960=ORIENTED_EDGE('',*,*,#10489,.T.);
#14961=ORIENTED_EDGE('',*,*,#10490,.T.);
#14962=ORIENTED_EDGE('',*,*,#10485,.T.);
#14963=ORIENTED_EDGE('',*,*,#10483,.T.);
#14964=ORIENTED_EDGE('',*,*,#10481,.T.);
#14965=ORIENTED_EDGE('',*,*,#10482,.T.);
#14966=ORIENTED_EDGE('',*,*,#10477,.T.);
#14967=ORIENTED_EDGE('',*,*,#10475,.T.);
#14968=ORIENTED_EDGE('',*,*,#10473,.T.);
#14969=ORIENTED_EDGE('',*,*,#10474,.T.);
#14970=ORIENTED_EDGE('',*,*,#10469,.T.);
#14971=ORIENTED_EDGE('',*,*,#10467,.T.);
#14972=ORIENTED_EDGE('',*,*,#10465,.T.);
#14973=ORIENTED_EDGE('',*,*,#10466,.T.);
#14974=ORIENTED_EDGE('',*,*,#10461,.T.);
#14975=ORIENTED_EDGE('',*,*,#10459,.T.);
#14976=ORIENTED_EDGE('',*,*,#10457,.T.);
#14977=ORIENTED_EDGE('',*,*,#10458,.T.);
#14978=ORIENTED_EDGE('',*,*,#10453,.T.);
#14979=ORIENTED_EDGE('',*,*,#10451,.T.);
#14980=ORIENTED_EDGE('',*,*,#10449,.T.);
#14981=ORIENTED_EDGE('',*,*,#10450,.T.);
#14982=ORIENTED_EDGE('',*,*,#10445,.T.);
#14983=ORIENTED_EDGE('',*,*,#10443,.T.);
#14984=ORIENTED_EDGE('',*,*,#10441,.T.);
#14985=ORIENTED_EDGE('',*,*,#10442,.T.);
#14986=ORIENTED_EDGE('',*,*,#10437,.T.);
#14987=ORIENTED_EDGE('',*,*,#10435,.T.);
#14988=ORIENTED_EDGE('',*,*,#10427,.T.);
#14989=ORIENTED_EDGE('',*,*,#10428,.T.);
#14990=ORIENTED_EDGE('',*,*,#10419,.F.);
#14991=ORIENTED_EDGE('',*,*,#10741,.T.);
#14992=ORIENTED_EDGE('',*,*,#10747,.F.);
#14993=ORIENTED_EDGE('',*,*,#10748,.F.);
#14994=ORIENTED_EDGE('',*,*,#10749,.F.);
#14995=ORIENTED_EDGE('',*,*,#10750,.F.);
#14996=ORIENTED_EDGE('',*,*,#10751,.F.);
#14997=ORIENTED_EDGE('',*,*,#10752,.F.);
#14998=ORIENTED_EDGE('',*,*,#10753,.F.);
#14999=ORIENTED_EDGE('',*,*,#10754,.F.);
#15000=ORIENTED_EDGE('',*,*,#10755,.F.);
#15001=ORIENTED_EDGE('',*,*,#10752,.T.);
#15002=ORIENTED_EDGE('',*,*,#10756,.T.);
#15003=ORIENTED_EDGE('',*,*,#10757,.T.);
#15004=ORIENTED_EDGE('',*,*,#10758,.T.);
#15005=ORIENTED_EDGE('',*,*,#10751,.T.);
#15006=ORIENTED_EDGE('',*,*,#10759,.F.);
#15007=ORIENTED_EDGE('',*,*,#10760,.T.);
#15008=ORIENTED_EDGE('',*,*,#10756,.F.);
#15009=ORIENTED_EDGE('',*,*,#10750,.T.);
#15010=ORIENTED_EDGE('',*,*,#10761,.T.);
#15011=ORIENTED_EDGE('',*,*,#10762,.T.);
#15012=ORIENTED_EDGE('',*,*,#10759,.T.);
#15013=ORIENTED_EDGE('',*,*,#10749,.T.);
#15014=ORIENTED_EDGE('',*,*,#10763,.F.);
#15015=ORIENTED_EDGE('',*,*,#10764,.T.);
#15016=ORIENTED_EDGE('',*,*,#10761,.F.);
#15017=ORIENTED_EDGE('',*,*,#10765,.F.);
#15018=ORIENTED_EDGE('',*,*,#10766,.F.);
#15019=ORIENTED_EDGE('',*,*,#10757,.F.);
#15020=ORIENTED_EDGE('',*,*,#10760,.F.);
#15021=ORIENTED_EDGE('',*,*,#10762,.F.);
#15022=ORIENTED_EDGE('',*,*,#10764,.F.);
#15023=ORIENTED_EDGE('',*,*,#10767,.F.);
#15024=ORIENTED_EDGE('',*,*,#10768,.F.);
#15025=ORIENTED_EDGE('',*,*,#10753,.T.);
#15026=ORIENTED_EDGE('',*,*,#10758,.F.);
#15027=ORIENTED_EDGE('',*,*,#10766,.T.);
#15028=ORIENTED_EDGE('',*,*,#10769,.F.);
#15029=ORIENTED_EDGE('',*,*,#10748,.T.);
#15030=ORIENTED_EDGE('',*,*,#10770,.T.);
#15031=ORIENTED_EDGE('',*,*,#10767,.T.);
#15032=ORIENTED_EDGE('',*,*,#10763,.T.);
#15033=ORIENTED_EDGE('',*,*,#10754,.T.);
#15034=ORIENTED_EDGE('',*,*,#10769,.T.);
#15035=ORIENTED_EDGE('',*,*,#10765,.T.);
#15036=ORIENTED_EDGE('',*,*,#10771,.T.);
#15037=ORIENTED_EDGE('',*,*,#10755,.T.);
#15038=ORIENTED_EDGE('',*,*,#10771,.F.);
#15039=ORIENTED_EDGE('',*,*,#10768,.T.);
#15040=ORIENTED_EDGE('',*,*,#10770,.F.);
#15041=ORIENTED_EDGE('',*,*,#10772,.F.);
#15042=ORIENTED_EDGE('',*,*,#10773,.T.);
#15043=ORIENTED_EDGE('',*,*,#10774,.T.);
#15044=ORIENTED_EDGE('',*,*,#10775,.F.);
#15045=ORIENTED_EDGE('',*,*,#10776,.F.);
#15046=ORIENTED_EDGE('',*,*,#10777,.T.);
#15047=ORIENTED_EDGE('',*,*,#10778,.T.);
#15048=ORIENTED_EDGE('',*,*,#10773,.F.);
#15049=ORIENTED_EDGE('',*,*,#10779,.F.);
#15050=ORIENTED_EDGE('',*,*,#10780,.T.);
#15051=ORIENTED_EDGE('',*,*,#10781,.T.);
#15052=ORIENTED_EDGE('',*,*,#10777,.F.);
#15053=ORIENTED_EDGE('',*,*,#10782,.F.);
#15054=ORIENTED_EDGE('',*,*,#10783,.T.);
#15055=ORIENTED_EDGE('',*,*,#10784,.T.);
#15056=ORIENTED_EDGE('',*,*,#10780,.F.);
#15057=ORIENTED_EDGE('',*,*,#10785,.F.);
#15058=ORIENTED_EDGE('',*,*,#10786,.T.);
#15059=ORIENTED_EDGE('',*,*,#10787,.T.);
#15060=ORIENTED_EDGE('',*,*,#10783,.F.);
#15061=ORIENTED_EDGE('',*,*,#10788,.F.);
#15062=ORIENTED_EDGE('',*,*,#10775,.T.);
#15063=ORIENTED_EDGE('',*,*,#10789,.T.);
#15064=ORIENTED_EDGE('',*,*,#10786,.F.);
#15065=ORIENTED_EDGE('',*,*,#10789,.F.);
#15066=ORIENTED_EDGE('',*,*,#10774,.F.);
#15067=ORIENTED_EDGE('',*,*,#10778,.F.);
#15068=ORIENTED_EDGE('',*,*,#10781,.F.);
#15069=ORIENTED_EDGE('',*,*,#10784,.F.);
#15070=ORIENTED_EDGE('',*,*,#10787,.F.);
#15071=ORIENTED_EDGE('',*,*,#10790,.F.);
#15072=ORIENTED_EDGE('',*,*,#10772,.T.);
#15073=ORIENTED_EDGE('',*,*,#10788,.T.);
#15074=ORIENTED_EDGE('',*,*,#10785,.T.);
#15075=ORIENTED_EDGE('',*,*,#10782,.T.);
#15076=ORIENTED_EDGE('',*,*,#10779,.T.);
#15077=ORIENTED_EDGE('',*,*,#10776,.T.);
#15078=ORIENTED_EDGE('',*,*,#10791,.F.);
#15079=ORIENTED_EDGE('',*,*,#10792,.T.);
#15080=ORIENTED_EDGE('',*,*,#10790,.T.);
#15081=ORIENTED_EDGE('',*,*,#10792,.F.);
#15082=ORIENTED_EDGE('',*,*,#10793,.F.);
#15083=ORIENTED_EDGE('',*,*,#10794,.T.);
#15084=ORIENTED_EDGE('',*,*,#10791,.T.);
#15085=ORIENTED_EDGE('',*,*,#10794,.F.);
#15086=ORIENTED_EDGE('',*,*,#10795,.F.);
#15087=ORIENTED_EDGE('',*,*,#10796,.T.);
#15088=ORIENTED_EDGE('',*,*,#10793,.T.);
#15089=ORIENTED_EDGE('',*,*,#10796,.F.);
#15090=ORIENTED_EDGE('',*,*,#10795,.T.);
#15091=ORIENTED_EDGE('',*,*,#10797,.F.);
#15092=ORIENTED_EDGE('',*,*,#10798,.F.);
#15093=ORIENTED_EDGE('',*,*,#10799,.T.);
#15094=ORIENTED_EDGE('',*,*,#10797,.T.);
#15095=ORIENTED_EDGE('',*,*,#10799,.F.);
#15096=ORIENTED_EDGE('',*,*,#10800,.F.);
#15097=ORIENTED_EDGE('',*,*,#10801,.T.);
#15098=ORIENTED_EDGE('',*,*,#10798,.T.);
#15099=ORIENTED_EDGE('',*,*,#10801,.F.);
#15100=ORIENTED_EDGE('',*,*,#10802,.F.);
#15101=ORIENTED_EDGE('',*,*,#10803,.T.);
#15102=ORIENTED_EDGE('',*,*,#10800,.T.);
#15103=ORIENTED_EDGE('',*,*,#10803,.F.);
#15104=ORIENTED_EDGE('',*,*,#10802,.T.);
#15105=ORIENTED_EDGE('',*,*,#10804,.F.);
#15106=ORIENTED_EDGE('',*,*,#10805,.F.);
#15107=ORIENTED_EDGE('',*,*,#10806,.T.);
#15108=ORIENTED_EDGE('',*,*,#10804,.T.);
#15109=ORIENTED_EDGE('',*,*,#10806,.F.);
#15110=ORIENTED_EDGE('',*,*,#10807,.F.);
#15111=ORIENTED_EDGE('',*,*,#10808,.T.);
#15112=ORIENTED_EDGE('',*,*,#10805,.T.);
#15113=ORIENTED_EDGE('',*,*,#10808,.F.);
#15114=ORIENTED_EDGE('',*,*,#10809,.F.);
#15115=ORIENTED_EDGE('',*,*,#10810,.T.);
#15116=ORIENTED_EDGE('',*,*,#10807,.T.);
#15117=ORIENTED_EDGE('',*,*,#10810,.F.);
#15118=ORIENTED_EDGE('',*,*,#10809,.T.);
#15119=ORIENTED_EDGE('',*,*,#10811,.T.);
#15120=ORIENTED_EDGE('',*,*,#10812,.T.);
#15121=ORIENTED_EDGE('',*,*,#10813,.T.);
#15122=ORIENTED_EDGE('',*,*,#10814,.F.);
#15123=ORIENTED_EDGE('',*,*,#10815,.T.);
#15124=ORIENTED_EDGE('',*,*,#10816,.T.);
#15125=ORIENTED_EDGE('',*,*,#10817,.T.);
#15126=ORIENTED_EDGE('',*,*,#10812,.F.);
#15127=ORIENTED_EDGE('',*,*,#10818,.T.);
#15128=ORIENTED_EDGE('',*,*,#10819,.T.);
#15129=ORIENTED_EDGE('',*,*,#10820,.T.);
#15130=ORIENTED_EDGE('',*,*,#10816,.F.);
#15131=ORIENTED_EDGE('',*,*,#10821,.T.);
#15132=ORIENTED_EDGE('',*,*,#10822,.T.);
#15133=ORIENTED_EDGE('',*,*,#10823,.T.);
#15134=ORIENTED_EDGE('',*,*,#10819,.F.);
#15135=ORIENTED_EDGE('',*,*,#10824,.T.);
#15136=ORIENTED_EDGE('',*,*,#10825,.T.);
#15137=ORIENTED_EDGE('',*,*,#10826,.T.);
#15138=ORIENTED_EDGE('',*,*,#10822,.F.);
#15139=ORIENTED_EDGE('',*,*,#10827,.T.);
#15140=ORIENTED_EDGE('',*,*,#10814,.T.);
#15141=ORIENTED_EDGE('',*,*,#10828,.T.);
#15142=ORIENTED_EDGE('',*,*,#10825,.F.);
#15143=ORIENTED_EDGE('',*,*,#10827,.F.);
#15144=ORIENTED_EDGE('',*,*,#10824,.F.);
#15145=ORIENTED_EDGE('',*,*,#10821,.F.);
#15146=ORIENTED_EDGE('',*,*,#10818,.F.);
#15147=ORIENTED_EDGE('',*,*,#10815,.F.);
#15148=ORIENTED_EDGE('',*,*,#10811,.F.);
#15149=ORIENTED_EDGE('',*,*,#10828,.F.);
#15150=ORIENTED_EDGE('',*,*,#10813,.F.);
#15151=ORIENTED_EDGE('',*,*,#10817,.F.);
#15152=ORIENTED_EDGE('',*,*,#10820,.F.);
#15153=ORIENTED_EDGE('',*,*,#10823,.F.);
#15154=ORIENTED_EDGE('',*,*,#10826,.F.);
#15155=ORIENTED_EDGE('',*,*,#10829,.F.);
#15156=ORIENTED_EDGE('',*,*,#10830,.T.);
#15157=ORIENTED_EDGE('',*,*,#10831,.T.);
#15158=ORIENTED_EDGE('',*,*,#10830,.F.);
#15159=ORIENTED_EDGE('',*,*,#10832,.F.);
#15160=ORIENTED_EDGE('',*,*,#10833,.T.);
#15161=ORIENTED_EDGE('',*,*,#10834,.T.);
#15162=ORIENTED_EDGE('',*,*,#10833,.F.);
#15163=ORIENTED_EDGE('',*,*,#10832,.T.);
#15164=ORIENTED_EDGE('',*,*,#10829,.T.);
#15165=ORIENTED_EDGE('',*,*,#10834,.F.);
#15166=ORIENTED_EDGE('',*,*,#10831,.F.);
#15167=CYLINDRICAL_SURFACE('',#17161,0.25);
#15168=CYLINDRICAL_SURFACE('',#17164,0.25);
#15169=CYLINDRICAL_SURFACE('',#17167,0.25);
#15170=CYLINDRICAL_SURFACE('',#17177,0.225000000000001);
#15171=CYLINDRICAL_SURFACE('',#17180,0.225000000000001);
#15172=CYLINDRICAL_SURFACE('',#17183,0.164999999999999);
#15173=CYLINDRICAL_SURFACE('',#17186,0.164999999999999);
#15174=CYLINDRICAL_SURFACE('',#17189,0.164999999999999);
#15175=CYLINDRICAL_SURFACE('',#17192,0.164999999999999);
#15176=CYLINDRICAL_SURFACE('',#17195,2.35);
#15177=CYLINDRICAL_SURFACE('',#17198,0.164999999999999);
#15178=CYLINDRICAL_SURFACE('',#17201,0.164999999999999);
#15179=CYLINDRICAL_SURFACE('',#17204,0.164999999999999);
#15180=CYLINDRICAL_SURFACE('',#17207,0.164999999999999);
#15181=CYLINDRICAL_SURFACE('',#17210,1.6);
#15182=CYLINDRICAL_SURFACE('',#17213,0.165);
#15183=CYLINDRICAL_SURFACE('',#17216,0.165);
#15184=CYLINDRICAL_SURFACE('',#17219,0.165);
#15185=CYLINDRICAL_SURFACE('',#17222,0.165);
#15186=CYLINDRICAL_SURFACE('',#17225,2.35);
#15187=CYLINDRICAL_SURFACE('',#17228,0.165);
#15188=CYLINDRICAL_SURFACE('',#17231,0.165);
#15189=CYLINDRICAL_SURFACE('',#17234,0.165);
#15190=CYLINDRICAL_SURFACE('',#17237,0.165);
#15191=CYLINDRICAL_SURFACE('',#17240,1.6);
#15192=CYLINDRICAL_SURFACE('',#17243,0.33);
#15193=CYLINDRICAL_SURFACE('',#17246,0.33);
#15194=CYLINDRICAL_SURFACE('',#17249,0.329999999999998);
#15195=CYLINDRICAL_SURFACE('',#17261,0.225);
#15196=CYLINDRICAL_SURFACE('',#17264,0.225);
#15197=CYLINDRICAL_SURFACE('',#17267,0.225);
#15198=CYLINDRICAL_SURFACE('',#17270,0.225);
#15199=CYLINDRICAL_SURFACE('',#17273,1.59);
#15200=CYLINDRICAL_SURFACE('',#17278,1.2);
#15201=CYLINDRICAL_SURFACE('',#17280,2.5);
#15202=CYLINDRICAL_SURFACE('',#17286,0.225);
#15203=CYLINDRICAL_SURFACE('',#17289,0.225);
#15204=CYLINDRICAL_SURFACE('',#17292,0.225);
#15205=CYLINDRICAL_SURFACE('',#17295,0.225);
#15206=CYLINDRICAL_SURFACE('',#17298,1.59);
#15207=CYLINDRICAL_SURFACE('',#17303,1.2);
#15208=CYLINDRICAL_SURFACE('',#17305,2.5);
#15209=CYLINDRICAL_SURFACE('',#17311,0.225);
#15210=CYLINDRICAL_SURFACE('',#17314,0.225);
#15211=CYLINDRICAL_SURFACE('',#17317,0.225000000000001);
#15212=CYLINDRICAL_SURFACE('',#17320,0.225000000000001);
#15213=CYLINDRICAL_SURFACE('',#17323,2.34);
#15214=CYLINDRICAL_SURFACE('',#17328,1.9);
#15215=CYLINDRICAL_SURFACE('',#17330,3.);
#15216=CYLINDRICAL_SURFACE('',#17336,0.225);
#15217=CYLINDRICAL_SURFACE('',#17339,0.225);
#15218=CYLINDRICAL_SURFACE('',#17342,0.225000000000001);
#15219=CYLINDRICAL_SURFACE('',#17345,0.225000000000001);
#15220=CYLINDRICAL_SURFACE('',#17348,2.34);
#15221=CYLINDRICAL_SURFACE('',#17353,1.9);
#15222=CYLINDRICAL_SURFACE('',#17355,3.);
#15223=CYLINDRICAL_SURFACE('',#17375,0.5);
#15224=CYLINDRICAL_SURFACE('',#17383,0.2942);
#15225=CYLINDRICAL_SURFACE('',#17385,0.225);
#15226=CYLINDRICAL_SURFACE('',#17388,0.225);
#15227=CYLINDRICAL_SURFACE('',#17391,0.225);
#15228=CYLINDRICAL_SURFACE('',#17394,0.225);
#15229=CYLINDRICAL_SURFACE('',#17397,1.59);
#15230=CYLINDRICAL_SURFACE('',#17402,1.2);
#15231=CYLINDRICAL_SURFACE('',#17404,2.5);
#15232=CYLINDRICAL_SURFACE('',#17410,0.225);
#15233=CYLINDRICAL_SURFACE('',#17413,0.225);
#15234=CYLINDRICAL_SURFACE('',#17416,0.225);
#15235=CYLINDRICAL_SURFACE('',#17419,0.225);
#15236=CYLINDRICAL_SURFACE('',#17422,1.59);
#15237=CYLINDRICAL_SURFACE('',#17427,1.2);
#15238=CYLINDRICAL_SURFACE('',#17429,2.5);
#15239=CYLINDRICAL_SURFACE('',#17435,0.225000000000001);
#15240=CYLINDRICAL_SURFACE('',#17438,0.225000000000001);
#15241=CYLINDRICAL_SURFACE('',#17441,0.225000000000001);
#15242=CYLINDRICAL_SURFACE('',#17444,0.225000000000001);
#15243=CYLINDRICAL_SURFACE('',#17447,2.34);
#15244=CYLINDRICAL_SURFACE('',#17452,1.9);
#15245=CYLINDRICAL_SURFACE('',#17454,3.);
#15246=CYLINDRICAL_SURFACE('',#17460,0.225000000000001);
#15247=CYLINDRICAL_SURFACE('',#17463,0.225000000000001);
#15248=CYLINDRICAL_SURFACE('',#17466,0.225000000000001);
#15249=CYLINDRICAL_SURFACE('',#17469,0.225000000000001);
#15250=CYLINDRICAL_SURFACE('',#17472,2.34);
#15251=CYLINDRICAL_SURFACE('',#17477,1.9);
#15252=CYLINDRICAL_SURFACE('',#17479,3.);
#15253=CYLINDRICAL_SURFACE('',#17492,1.070235);
#15254=CYLINDRICAL_SURFACE('',#17494,0.6);
#15255=CYLINDRICAL_SURFACE('',#17500,1.070235);
#15256=CYLINDRICAL_SURFACE('',#17512,1.129765);
#15257=CYLINDRICAL_SURFACE('',#17519,1.6);
#15258=CYLINDRICAL_SURFACE('',#17524,1.129765);
#15259=CYLINDRICAL_SURFACE('',#17544,1.123812);
#15260=CYLINDRICAL_SURFACE('',#17580,1.076188);
#15261=CYLINDRICAL_SURFACE('',#17594,1.119765);
#15262=CYLINDRICAL_SURFACE('',#17598,1.085235);
#15263=CYLINDRICAL_SURFACE('',#17602,1.119765);
#15264=CYLINDRICAL_SURFACE('',#17606,1.085235);
#15265=CYLINDRICAL_SURFACE('',#17620,1.63531);
#15266=CYLINDRICAL_SURFACE('',#17622,1.);
#15267=CYLINDRICAL_SURFACE('',#17628,1.63531);
#15268=CYLINDRICAL_SURFACE('',#17640,1.71469);
#15269=CYLINDRICAL_SURFACE('',#17647,2.35);
#15270=CYLINDRICAL_SURFACE('',#17652,1.71469);
#15271=CYLINDRICAL_SURFACE('',#17674,1.706752);
#15272=CYLINDRICAL_SURFACE('',#17714,1.643248);
#15273=CYLINDRICAL_SURFACE('',#17728,1.70469);
#15274=CYLINDRICAL_SURFACE('',#17732,1.65031);
#15275=CYLINDRICAL_SURFACE('',#17736,1.70469);
#15276=CYLINDRICAL_SURFACE('',#17740,1.65031);
#15277=CYLINDRICAL_SURFACE('',#17761,0.35);
#15278=CYLINDRICAL_SURFACE('',#17769,0.1954);
#15279=CYLINDRICAL_SURFACE('',#17891,0.225000000000001);
#15280=CYLINDRICAL_SURFACE('',#17894,0.225000000000001);
#15281=CYLINDRICAL_SURFACE('',#17897,1.525);
#15282=CYLINDRICAL_SURFACE('',#17911,4.);
#15283=CYLINDRICAL_SURFACE('',#17913,0.164999999999999);
#15284=CYLINDRICAL_SURFACE('',#17916,0.5);
#15285=CYLINDRICAL_SURFACE('',#17922,0.164999999999999);
#15286=CYLINDRICAL_SURFACE('',#17925,0.5);
#15287=CYLINDRICAL_SURFACE('',#17956,0.2);
#15288=CYLINDRICAL_SURFACE('',#17963,0.35);
#15289=CYLINDRICAL_SURFACE('',#17971,0.1954);
#15290=CYLINDRICAL_SURFACE('',#17974,0.165);
#15291=CYLINDRICAL_SURFACE('',#17998,0.9);
#15292=CYLINDRICAL_SURFACE('',#17999,0.6);
#15293=CYLINDRICAL_SURFACE('',#18001,0.6);
#15294=CYLINDRICAL_SURFACE('',#18006,0.605);
#15295=CYLINDRICAL_SURFACE('',#18009,0.9);
#15296=CYLINDRICAL_SURFACE('',#18015,0.605);
#15297=CYLINDRICAL_SURFACE('',#18018,0.9);
#15298=CYLINDRICAL_SURFACE('',#18026,0.21);
#15299=CYLINDRICAL_SURFACE('',#18030,0.605);
#15300=CYLINDRICAL_SURFACE('',#18033,1.);
#15301=CYLINDRICAL_SURFACE('',#18039,0.25);
#15302=CYLINDRICAL_SURFACE('',#18048,0.6);
#15303=CYLINDRICAL_SURFACE('',#18050,1.);
#15304=CYLINDRICAL_SURFACE('',#18059,1.25);
#15305=CYLINDRICAL_SURFACE('',#18063,0.605);
#15306=CYLINDRICAL_SURFACE('',#18066,0.9);
#15307=CYLINDRICAL_SURFACE('',#18072,0.605);
#15308=CYLINDRICAL_SURFACE('',#18075,0.9);
#15309=CYLINDRICAL_SURFACE('',#18081,0.225);
#15310=CYLINDRICAL_SURFACE('',#18084,1.);
#15311=CYLINDRICAL_SURFACE('',#18090,0.33);
#15312=CYLINDRICAL_SURFACE('',#18093,0.4);
#15313=CYLINDRICAL_SURFACE('',#18099,0.32);
#15314=CYLINDRICAL_SURFACE('',#18102,0.6);
#15315=CYLINDRICAL_SURFACE('',#18119,0.3);
#15316=CYLINDRICAL_SURFACE('',#18126,0.5);
#15317=CYLINDRICAL_SURFACE('',#18134,0.2942);
#15318=CYLINDRICAL_SURFACE('',#18137,0.165);
#15319=CYLINDRICAL_SURFACE('',#18154,1.3);
#15320=CYLINDRICAL_SURFACE('',#18155,1.);
#15321=CYLINDRICAL_SURFACE('',#18157,1.);
#15322=CYLINDRICAL_SURFACE('',#18162,1.005);
#15323=CYLINDRICAL_SURFACE('',#18165,1.3);
#15324=CYLINDRICAL_SURFACE('',#18171,1.005);
#15325=CYLINDRICAL_SURFACE('',#18174,1.3);
#15326=CYLINDRICAL_SURFACE('',#18182,0.21);
#15327=CYLINDRICAL_SURFACE('',#18186,1.005);
#15328=CYLINDRICAL_SURFACE('',#18189,1.4);
#15329=CYLINDRICAL_SURFACE('',#18195,0.225);
#15330=CYLINDRICAL_SURFACE('',#18198,1.4);
#15331=CYLINDRICAL_SURFACE('',#18205,0.164999999999999);
#15332=CYLINDRICAL_SURFACE('',#18222,0.9);
#15333=CYLINDRICAL_SURFACE('',#18223,0.6);
#15334=CYLINDRICAL_SURFACE('',#18225,0.6);
#15335=CYLINDRICAL_SURFACE('',#18230,0.605);
#15336=CYLINDRICAL_SURFACE('',#18233,0.9);
#15337=CYLINDRICAL_SURFACE('',#18239,0.605);
#15338=CYLINDRICAL_SURFACE('',#18242,0.9);
#15339=CYLINDRICAL_SURFACE('',#18250,0.210000000000001);
#15340=CYLINDRICAL_SURFACE('',#18254,0.605);
#15341=CYLINDRICAL_SURFACE('',#18257,1.);
#15342=CYLINDRICAL_SURFACE('',#18263,0.225);
#15343=CYLINDRICAL_SURFACE('',#18266,1.);
#15344=CYLINDRICAL_SURFACE('',#18297,0.6);
#15345=CYLINDRICAL_SURFACE('',#18299,1.4);
#15346=CYLINDRICAL_SURFACE('',#18304,1.75);
#15347=CYLINDRICAL_SURFACE('',#18307,1.75);
#15348=CYLINDRICAL_SURFACE('',#18310,1.75);
#15349=CYLINDRICAL_SURFACE('',#18313,1.75);
#15350=CYLINDRICAL_SURFACE('',#18316,1.75);
#15351=CYLINDRICAL_SURFACE('',#18319,1.75);
#15352=CYLINDRICAL_SURFACE('',#18322,1.75);
#15353=CYLINDRICAL_SURFACE('',#18325,1.75);
#15354=CYLINDRICAL_SURFACE('',#18328,1.75);
#15355=CYLINDRICAL_SURFACE('',#18331,1.75);
#15356=CYLINDRICAL_SURFACE('',#18334,1.75);
#15357=CYLINDRICAL_SURFACE('',#18337,1.75);
#15358=CYLINDRICAL_SURFACE('',#18340,1.75);
#15359=CYLINDRICAL_SURFACE('',#18343,1.75);
#15360=CYLINDRICAL_SURFACE('',#18346,1.75);
#15361=CYLINDRICAL_SURFACE('',#18349,1.75);
#15362=CYLINDRICAL_SURFACE('',#18352,1.75);
#15363=CYLINDRICAL_SURFACE('',#18355,1.75);
#15364=CYLINDRICAL_SURFACE('',#18358,1.75);
#15365=CYLINDRICAL_SURFACE('',#18363,1.75);
#15366=CYLINDRICAL_SURFACE('',#18377,0.164999999999999);
#15367=CYLINDRICAL_SURFACE('',#18394,1.3);
#15368=CYLINDRICAL_SURFACE('',#18395,1.);
#15369=CYLINDRICAL_SURFACE('',#18397,1.);
#15370=CYLINDRICAL_SURFACE('',#18402,1.005);
#15371=CYLINDRICAL_SURFACE('',#18405,1.3);
#15372=CYLINDRICAL_SURFACE('',#18411,1.005);
#15373=CYLINDRICAL_SURFACE('',#18414,1.3);
#15374=CYLINDRICAL_SURFACE('',#18422,0.210000000000001);
#15375=CYLINDRICAL_SURFACE('',#18426,1.005);
#15376=CYLINDRICAL_SURFACE('',#18429,1.4);
#15377=CYLINDRICAL_SURFACE('',#18435,1.005);
#15378=CYLINDRICAL_SURFACE('',#18438,1.4);
#15379=CYLINDRICAL_SURFACE('',#18444,1.005);
#15380=CYLINDRICAL_SURFACE('',#18447,1.4);
#15381=CYLINDRICAL_SURFACE('',#18455,0.210000000000001);
#15382=CYLINDRICAL_SURFACE('',#18465,1.);
#15383=CYLINDRICAL_SURFACE('',#18468,1.5);
#15384=CYLINDRICAL_SURFACE('',#18474,0.225000000000001);
#15385=CYLINDRICAL_SURFACE('',#18477,1.4);
#15386=CYLINDRICAL_SURFACE('',#18528,1.);
#15387=CYLINDRICAL_SURFACE('',#18530,2.);
#15388=CYLINDRICAL_SURFACE('',#18535,3.75);
#15389=CYLINDRICAL_SURFACE('',#18538,3.75);
#15390=CYLINDRICAL_SURFACE('',#18541,3.75);
#15391=CYLINDRICAL_SURFACE('',#18544,3.75);
#15392=CYLINDRICAL_SURFACE('',#18547,3.75);
#15393=CYLINDRICAL_SURFACE('',#18550,3.75);
#15394=CYLINDRICAL_SURFACE('',#18553,3.75);
#15395=CYLINDRICAL_SURFACE('',#18556,3.75);
#15396=CYLINDRICAL_SURFACE('',#18559,3.75);
#15397=CYLINDRICAL_SURFACE('',#18562,3.75);
#15398=CYLINDRICAL_SURFACE('',#18565,3.75);
#15399=CYLINDRICAL_SURFACE('',#18568,3.75);
#15400=CYLINDRICAL_SURFACE('',#18571,3.75);
#15401=CYLINDRICAL_SURFACE('',#18574,3.75);
#15402=CYLINDRICAL_SURFACE('',#18577,3.75);
#15403=CYLINDRICAL_SURFACE('',#18580,3.75);
#15404=CYLINDRICAL_SURFACE('',#18583,3.75);
#15405=CYLINDRICAL_SURFACE('',#18586,3.75);
#15406=CYLINDRICAL_SURFACE('',#18589,3.75);
#15407=CYLINDRICAL_SURFACE('',#18592,3.75);
#15408=CYLINDRICAL_SURFACE('',#18595,3.75);
#15409=CYLINDRICAL_SURFACE('',#18598,3.75);
#15410=CYLINDRICAL_SURFACE('',#18601,3.75);
#15411=CYLINDRICAL_SURFACE('',#18604,3.75);
#15412=CYLINDRICAL_SURFACE('',#18607,3.75);
#15413=CYLINDRICAL_SURFACE('',#18610,3.75);
#15414=CYLINDRICAL_SURFACE('',#18613,3.75);
#15415=CYLINDRICAL_SURFACE('',#18616,3.75);
#15416=CYLINDRICAL_SURFACE('',#18619,3.75);
#15417=CYLINDRICAL_SURFACE('',#18622,3.75);
#15418=CYLINDRICAL_SURFACE('',#18625,3.75);
#15419=CYLINDRICAL_SURFACE('',#18628,3.75);
#15420=CYLINDRICAL_SURFACE('',#18631,3.75);
#15421=CYLINDRICAL_SURFACE('',#18634,3.75);
#15422=CYLINDRICAL_SURFACE('',#18637,3.75);
#15423=CYLINDRICAL_SURFACE('',#18640,3.75);
#15424=CYLINDRICAL_SURFACE('',#18643,3.75);
#15425=CYLINDRICAL_SURFACE('',#18646,3.75);
#15426=CYLINDRICAL_SURFACE('',#18649,3.75);
#15427=CYLINDRICAL_SURFACE('',#18654,3.75);
#15428=CYLINDRICAL_SURFACE('',#18678,0.24505);
#15429=CYLINDRICAL_SURFACE('',#18688,0.35);
#15430=CYLINDRICAL_SURFACE('',#18696,0.1954);
#15431=CYLINDRICAL_SURFACE('',#18816,0.405);
#15432=CYLINDRICAL_SURFACE('',#18819,0.9);
#15433=ADVANCED_FACE('',(#2123),#15167,.F.);
#15434=ADVANCED_FACE('',(#2124),#15168,.F.);
#15435=ADVANCED_FACE('',(#2125),#15169,.F.);
#15436=ADVANCED_FACE('',(#2126),#1633,.T.);
#15437=ADVANCED_FACE('',(#2127),#1634,.T.);
#15438=ADVANCED_FACE('',(#2128),#1635,.T.);
#15439=ADVANCED_FACE('',(#2129),#1636,.T.);
#15440=ADVANCED_FACE('',(#2130,#1342,#1343,#1344),#1637,.T.);
#15441=ADVANCED_FACE('',(#2131,#1345,#1346,#1347),#1638,.F.);
#15442=ADVANCED_FACE('',(#2132),#15170,.F.);
#15443=ADVANCED_FACE('',(#2133),#15171,.F.);
#15444=ADVANCED_FACE('',(#2134),#15172,.F.);
#15445=ADVANCED_FACE('',(#2135),#15173,.F.);
#15446=ADVANCED_FACE('',(#2136),#15174,.F.);
#15447=ADVANCED_FACE('',(#2137),#15175,.F.);
#15448=ADVANCED_FACE('',(#2138),#15176,.F.);
#15449=ADVANCED_FACE('',(#2139),#15177,.F.);
#15450=ADVANCED_FACE('',(#2140),#15178,.F.);
#15451=ADVANCED_FACE('',(#2141),#15179,.F.);
#15452=ADVANCED_FACE('',(#2142),#15180,.F.);
#15453=ADVANCED_FACE('',(#2143),#15181,.F.);
#15454=ADVANCED_FACE('',(#2144),#15182,.F.);
#15455=ADVANCED_FACE('',(#2145),#15183,.F.);
#15456=ADVANCED_FACE('',(#2146),#15184,.F.);
#15457=ADVANCED_FACE('',(#2147),#15185,.F.);
#15458=ADVANCED_FACE('',(#2148),#15186,.F.);
#15459=ADVANCED_FACE('',(#2149),#15187,.F.);
#15460=ADVANCED_FACE('',(#2150),#15188,.F.);
#15461=ADVANCED_FACE('',(#2151),#15189,.F.);
#15462=ADVANCED_FACE('',(#2152),#15190,.F.);
#15463=ADVANCED_FACE('',(#2153),#15191,.F.);
#15464=ADVANCED_FACE('',(#2154),#15192,.F.);
#15465=ADVANCED_FACE('',(#2155),#15193,.F.);
#15466=ADVANCED_FACE('',(#2156),#15194,.F.);
#15467=ADVANCED_FACE('',(#2157,#1348,#1349,#1350),#1639,.T.);
#15468=ADVANCED_FACE('',(#2158),#1640,.F.);
#15469=ADVANCED_FACE('',(#2159,#1351,#1352,#1353,#1354,#1355,#1356,#1357,
#1358,#1359,#1360,#1361,#1362,#1363,#1364,#1365,#1366,#1367,#1368,#1369,
#1370,#1371,#1372),#1641,.T.);
#15470=ADVANCED_FACE('',(#2160),#1642,.T.);
#15471=ADVANCED_FACE('',(#2161,#1373,#1374,#1375,#1376,#1377,#1378,#1379,
#1380,#1381,#1382,#1383,#1384,#1385,#1386,#1387,#1388,#1389,#1390,#1391,
#1392,#1393,#1394),#1643,.T.);
#15472=ADVANCED_FACE('',(#2162),#1644,.T.);
#15473=ADVANCED_FACE('',(#2163),#1645,.T.);
#15474=ADVANCED_FACE('',(#2164,#1395,#1396,#1397),#1646,.F.);
#15475=ADVANCED_FACE('',(#2165),#15195,.F.);
#15476=ADVANCED_FACE('',(#2166),#15196,.F.);
#15477=ADVANCED_FACE('',(#2167),#15197,.F.);
#15478=ADVANCED_FACE('',(#2168),#15198,.F.);
#15479=ADVANCED_FACE('',(#2169),#15199,.T.);
#15480=ADVANCED_FACE('',(#2170,#1398),#1647,.T.);
#15481=ADVANCED_FACE('',(#2171),#15200,.F.);
#15482=ADVANCED_FACE('',(#2172),#15201,.T.);
#15483=ADVANCED_FACE('',(#2173,#1399,#1400,#1401,#1402,#1403),#1648,.T.);
#15484=ADVANCED_FACE('',(#2174,#1404,#1405,#1406,#1407,#1408),#1649,.F.);
#15485=ADVANCED_FACE('',(#2175),#15202,.F.);
#15486=ADVANCED_FACE('',(#2176),#15203,.F.);
#15487=ADVANCED_FACE('',(#2177),#15204,.F.);
#15488=ADVANCED_FACE('',(#2178),#15205,.F.);
#15489=ADVANCED_FACE('',(#2179),#15206,.T.);
#15490=ADVANCED_FACE('',(#2180,#1409),#1650,.F.);
#15491=ADVANCED_FACE('',(#2181),#15207,.F.);
#15492=ADVANCED_FACE('',(#2182),#15208,.T.);
#15493=ADVANCED_FACE('',(#2183,#1410,#1411,#1412,#1413,#1414),#1651,.T.);
#15494=ADVANCED_FACE('',(#2184,#1415,#1416,#1417,#1418,#1419),#1652,.F.);
#15495=ADVANCED_FACE('',(#2185),#15209,.F.);
#15496=ADVANCED_FACE('',(#2186),#15210,.F.);
#15497=ADVANCED_FACE('',(#2187),#15211,.F.);
#15498=ADVANCED_FACE('',(#2188),#15212,.F.);
#15499=ADVANCED_FACE('',(#2189),#15213,.T.);
#15500=ADVANCED_FACE('',(#2190,#1420),#1653,.T.);
#15501=ADVANCED_FACE('',(#2191),#15214,.F.);
#15502=ADVANCED_FACE('',(#2192),#15215,.T.);
#15503=ADVANCED_FACE('',(#2193,#1421,#1422,#1423,#1424,#1425),#1654,.T.);
#15504=ADVANCED_FACE('',(#2194,#1426,#1427,#1428,#1429,#1430),#1655,.F.);
#15505=ADVANCED_FACE('',(#2195),#15216,.F.);
#15506=ADVANCED_FACE('',(#2196),#15217,.F.);
#15507=ADVANCED_FACE('',(#2197),#15218,.F.);
#15508=ADVANCED_FACE('',(#2198),#15219,.F.);
#15509=ADVANCED_FACE('',(#2199),#15220,.T.);
#15510=ADVANCED_FACE('',(#2200,#1431),#1656,.F.);
#15511=ADVANCED_FACE('',(#2201),#15221,.F.);
#15512=ADVANCED_FACE('',(#2202),#15222,.T.);
#15513=ADVANCED_FACE('',(#2203,#1432,#1433,#1434,#1435,#1436),#1657,.T.);
#15514=ADVANCED_FACE('',(#2204,#1437,#1438,#1439,#1440,#1441),#1658,.F.);
#15515=ADVANCED_FACE('',(#2205),#1659,.F.);
#15516=ADVANCED_FACE('',(#2206),#1660,.F.);
#15517=ADVANCED_FACE('',(#2207),#1661,.F.);
#15518=ADVANCED_FACE('',(#2208),#1662,.F.);
#15519=ADVANCED_FACE('',(#2209),#1663,.F.);
#15520=ADVANCED_FACE('',(#2210),#1664,.F.);
#15521=ADVANCED_FACE('',(#2211),#1665,.F.);
#15522=ADVANCED_FACE('',(#2212),#1666,.F.);
#15523=ADVANCED_FACE('',(#2213),#1667,.F.);
#15524=ADVANCED_FACE('',(#2214),#1668,.T.);
#15525=ADVANCED_FACE('',(#2215),#1025,.T.);
#15526=ADVANCED_FACE('',(#2216),#15223,.T.);
#15527=ADVANCED_FACE('',(#2217),#1026,.T.);
#15528=ADVANCED_FACE('',(#2218,#1442),#1669,.T.);
#15529=ADVANCED_FACE('',(#2219),#1027,.T.);
#15530=ADVANCED_FACE('',(#2220),#15224,.T.);
#15531=ADVANCED_FACE('',(#2221),#15225,.F.);
#15532=ADVANCED_FACE('',(#2222),#15226,.F.);
#15533=ADVANCED_FACE('',(#2223),#15227,.F.);
#15534=ADVANCED_FACE('',(#2224),#15228,.F.);
#15535=ADVANCED_FACE('',(#2225),#15229,.T.);
#15536=ADVANCED_FACE('',(#2226,#1443),#1670,.T.);
#15537=ADVANCED_FACE('',(#2227),#15230,.F.);
#15538=ADVANCED_FACE('',(#2228),#15231,.T.);
#15539=ADVANCED_FACE('',(#2229,#1444,#1445,#1446,#1447,#1448),#1671,.T.);
#15540=ADVANCED_FACE('',(#2230,#1449,#1450,#1451,#1452,#1453),#1672,.F.);
#15541=ADVANCED_FACE('',(#2231),#15232,.F.);
#15542=ADVANCED_FACE('',(#2232),#15233,.F.);
#15543=ADVANCED_FACE('',(#2233),#15234,.F.);
#15544=ADVANCED_FACE('',(#2234),#15235,.F.);
#15545=ADVANCED_FACE('',(#2235),#15236,.T.);
#15546=ADVANCED_FACE('',(#2236,#1454),#1673,.F.);
#15547=ADVANCED_FACE('',(#2237),#15237,.F.);
#15548=ADVANCED_FACE('',(#2238),#15238,.T.);
#15549=ADVANCED_FACE('',(#2239,#1455,#1456,#1457,#1458,#1459),#1674,.T.);
#15550=ADVANCED_FACE('',(#2240,#1460,#1461,#1462,#1463,#1464),#1675,.F.);
#15551=ADVANCED_FACE('',(#2241),#15239,.F.);
#15552=ADVANCED_FACE('',(#2242),#15240,.F.);
#15553=ADVANCED_FACE('',(#2243),#15241,.F.);
#15554=ADVANCED_FACE('',(#2244),#15242,.F.);
#15555=ADVANCED_FACE('',(#2245),#15243,.T.);
#15556=ADVANCED_FACE('',(#2246,#1465),#1676,.T.);
#15557=ADVANCED_FACE('',(#2247),#15244,.F.);
#15558=ADVANCED_FACE('',(#2248),#15245,.T.);
#15559=ADVANCED_FACE('',(#2249,#1466,#1467,#1468,#1469,#1470),#1677,.T.);
#15560=ADVANCED_FACE('',(#2250,#1471,#1472,#1473,#1474,#1475),#1678,.F.);
#15561=ADVANCED_FACE('',(#2251),#15246,.F.);
#15562=ADVANCED_FACE('',(#2252),#15247,.F.);
#15563=ADVANCED_FACE('',(#2253),#15248,.F.);
#15564=ADVANCED_FACE('',(#2254),#15249,.F.);
#15565=ADVANCED_FACE('',(#2255),#15250,.T.);
#15566=ADVANCED_FACE('',(#2256,#1476),#1679,.F.);
#15567=ADVANCED_FACE('',(#2257),#15251,.F.);
#15568=ADVANCED_FACE('',(#2258),#15252,.T.);
#15569=ADVANCED_FACE('',(#2259,#1477,#1478,#1479,#1480,#1481),#1680,.T.);
#15570=ADVANCED_FACE('',(#2260,#1482,#1483,#1484,#1485,#1486),#1681,.F.);
#15571=ADVANCED_FACE('',(#2261),#1021,.F.);
#15572=ADVANCED_FACE('',(#2262),#15253,.T.);
#15573=ADVANCED_FACE('',(#2263),#15254,.F.);
#15574=ADVANCED_FACE('',(#2264),#1028,.F.);
#15575=ADVANCED_FACE('',(#2265,#1487),#1682,.T.);
#15576=ADVANCED_FACE('',(#2266),#15255,.T.);
#15577=ADVANCED_FACE('',(#2267,#1488),#1683,.T.);
#15578=ADVANCED_FACE('',(#2268),#1029,.F.);
#15579=ADVANCED_FACE('',(#2269),#1022,.F.);
#15580=ADVANCED_FACE('',(#2270),#15256,.F.);
#15581=ADVANCED_FACE('',(#2271,#1489),#1684,.T.);
#15582=ADVANCED_FACE('',(#2272),#1030,.T.);
#15583=ADVANCED_FACE('',(#2273),#15257,.T.);
#15584=ADVANCED_FACE('',(#2274),#1031,.T.);
#15585=ADVANCED_FACE('',(#2275,#1490),#1685,.T.);
#15586=ADVANCED_FACE('',(#2276),#15258,.F.);
#15587=ADVANCED_FACE('',(#2277),#991,.T.);
#15588=ADVANCED_FACE('',(#2278),#992,.T.);
#15589=ADVANCED_FACE('',(#2279),#993,.T.);
#15590=ADVANCED_FACE('',(#2280),#994,.T.);
#15591=ADVANCED_FACE('',(#2281),#995,.T.);
#15592=ADVANCED_FACE('',(#2282),#996,.T.);
#15593=ADVANCED_FACE('',(#2283),#997,.T.);
#15594=ADVANCED_FACE('',(#2284),#998,.F.);
#15595=ADVANCED_FACE('',(#2285),#15259,.T.);
#15596=ADVANCED_FACE('',(#2286),#1686,.T.);
#15597=ADVANCED_FACE('',(#2287),#999,.F.);
#15598=ADVANCED_FACE('',(#2288),#1687,.T.);
#15599=ADVANCED_FACE('',(#2289),#1000,.F.);
#15600=ADVANCED_FACE('',(#2290),#1688,.T.);
#15601=ADVANCED_FACE('',(#2291),#1001,.F.);
#15602=ADVANCED_FACE('',(#2292),#1689,.T.);
#15603=ADVANCED_FACE('',(#2293),#1002,.F.);
#15604=ADVANCED_FACE('',(#2294),#1690,.T.);
#15605=ADVANCED_FACE('',(#2295),#1003,.F.);
#15606=ADVANCED_FACE('',(#2296),#15260,.F.);
#15607=ADVANCED_FACE('',(#2297),#1691,.T.);
#15608=ADVANCED_FACE('',(#2298),#1004,.F.);
#15609=ADVANCED_FACE('',(#2299,#1491),#1692,.T.);
#15610=ADVANCED_FACE('',(#2300),#1693,.T.);
#15611=ADVANCED_FACE('',(#2301,#1492),#1694,.T.);
#15612=ADVANCED_FACE('',(#2302),#15261,.T.);
#15613=ADVANCED_FACE('',(#2303,#1493),#1695,.T.);
#15614=ADVANCED_FACE('',(#2304),#15262,.F.);
#15615=ADVANCED_FACE('',(#2305,#1494),#1696,.T.);
#15616=ADVANCED_FACE('',(#2306),#15263,.T.);
#15617=ADVANCED_FACE('',(#2307,#1495),#1697,.T.);
#15618=ADVANCED_FACE('',(#2308),#15264,.F.);
#15619=ADVANCED_FACE('',(#2309),#1023,.F.);
#15620=ADVANCED_FACE('',(#2310),#15265,.T.);
#15621=ADVANCED_FACE('',(#2311),#15266,.F.);
#15622=ADVANCED_FACE('',(#2312),#1032,.F.);
#15623=ADVANCED_FACE('',(#2313,#1496),#1698,.T.);
#15624=ADVANCED_FACE('',(#2314),#15267,.T.);
#15625=ADVANCED_FACE('',(#2315,#1497),#1699,.T.);
#15626=ADVANCED_FACE('',(#2316),#1033,.F.);
#15627=ADVANCED_FACE('',(#2317),#1024,.F.);
#15628=ADVANCED_FACE('',(#2318),#15268,.F.);
#15629=ADVANCED_FACE('',(#2319,#1498),#1700,.T.);
#15630=ADVANCED_FACE('',(#2320),#1034,.T.);
#15631=ADVANCED_FACE('',(#2321),#15269,.T.);
#15632=ADVANCED_FACE('',(#2322),#1035,.T.);
#15633=ADVANCED_FACE('',(#2323,#1499),#1701,.T.);
#15634=ADVANCED_FACE('',(#2324),#15270,.F.);
#15635=ADVANCED_FACE('',(#2325),#1005,.T.);
#15636=ADVANCED_FACE('',(#2326),#1006,.T.);
#15637=ADVANCED_FACE('',(#2327),#1007,.T.);
#15638=ADVANCED_FACE('',(#2328),#1008,.T.);
#15639=ADVANCED_FACE('',(#2329),#1009,.T.);
#15640=ADVANCED_FACE('',(#2330),#1010,.T.);
#15641=ADVANCED_FACE('',(#2331),#1011,.T.);
#15642=ADVANCED_FACE('',(#2332),#1012,.T.);
#15643=ADVANCED_FACE('',(#2333),#1013,.F.);
#15644=ADVANCED_FACE('',(#2334),#15271,.T.);
#15645=ADVANCED_FACE('',(#2335),#1702,.T.);
#15646=ADVANCED_FACE('',(#2336),#1014,.F.);
#15647=ADVANCED_FACE('',(#2337),#1703,.T.);
#15648=ADVANCED_FACE('',(#2338),#1015,.F.);
#15649=ADVANCED_FACE('',(#2339),#1704,.T.);
#15650=ADVANCED_FACE('',(#2340),#1016,.F.);
#15651=ADVANCED_FACE('',(#2341),#1705,.T.);
#15652=ADVANCED_FACE('',(#2342),#1017,.F.);
#15653=ADVANCED_FACE('',(#2343),#1706,.T.);
#15654=ADVANCED_FACE('',(#2344),#1018,.F.);
#15655=ADVANCED_FACE('',(#2345),#1707,.T.);
#15656=ADVANCED_FACE('',(#2346),#1019,.F.);
#15657=ADVANCED_FACE('',(#2347),#15272,.F.);
#15658=ADVANCED_FACE('',(#2348),#1708,.T.);
#15659=ADVANCED_FACE('',(#2349),#1020,.F.);
#15660=ADVANCED_FACE('',(#2350,#1500),#1709,.T.);
#15661=ADVANCED_FACE('',(#2351),#1710,.T.);
#15662=ADVANCED_FACE('',(#2352,#1501),#1711,.T.);
#15663=ADVANCED_FACE('',(#2353),#15273,.T.);
#15664=ADVANCED_FACE('',(#2354,#1502),#1712,.T.);
#15665=ADVANCED_FACE('',(#2355),#15274,.F.);
#15666=ADVANCED_FACE('',(#2356,#1503),#1713,.T.);
#15667=ADVANCED_FACE('',(#2357),#15275,.T.);
#15668=ADVANCED_FACE('',(#2358,#1504),#1714,.T.);
#15669=ADVANCED_FACE('',(#2359),#15276,.F.);
#15670=ADVANCED_FACE('',(#2360),#1715,.F.);
#15671=ADVANCED_FACE('',(#2361),#1716,.F.);
#15672=ADVANCED_FACE('',(#2362),#1717,.F.);
#15673=ADVANCED_FACE('',(#2363),#1718,.F.);
#15674=ADVANCED_FACE('',(#2364),#1719,.F.);
#15675=ADVANCED_FACE('',(#2365),#1720,.F.);
#15676=ADVANCED_FACE('',(#2366),#1721,.F.);
#15677=ADVANCED_FACE('',(#2367),#1722,.F.);
#15678=ADVANCED_FACE('',(#2368),#1723,.F.);
#15679=ADVANCED_FACE('',(#2369),#1724,.T.);
#15680=ADVANCED_FACE('',(#2370),#1036,.T.);
#15681=ADVANCED_FACE('',(#2371),#15277,.T.);
#15682=ADVANCED_FACE('',(#2372),#1037,.T.);
#15683=ADVANCED_FACE('',(#2373,#1505),#1725,.T.);
#15684=ADVANCED_FACE('',(#2374),#1038,.T.);
#15685=ADVANCED_FACE('',(#2375),#15278,.T.);
#15686=ADVANCED_FACE('',(#2376),#1726,.F.);
#15687=ADVANCED_FACE('',(#2377),#1727,.F.);
#15688=ADVANCED_FACE('',(#2378),#1728,.F.);
#15689=ADVANCED_FACE('',(#2379),#1729,.F.);
#15690=ADVANCED_FACE('',(#2380),#1730,.T.);
#15691=ADVANCED_FACE('',(#2381),#1731,.F.);
#15692=ADVANCED_FACE('',(#2382),#1732,.F.);
#15693=ADVANCED_FACE('',(#2383),#1733,.F.);
#15694=ADVANCED_FACE('',(#2384),#1734,.F.);
#15695=ADVANCED_FACE('',(#2385),#1735,.T.);
#15696=ADVANCED_FACE('',(#2386),#1736,.F.);
#15697=ADVANCED_FACE('',(#2387),#1737,.F.);
#15698=ADVANCED_FACE('',(#2388),#1738,.F.);
#15699=ADVANCED_FACE('',(#2389),#1739,.F.);
#15700=ADVANCED_FACE('',(#2390),#1740,.T.);
#15701=ADVANCED_FACE('',(#2391),#1741,.F.);
#15702=ADVANCED_FACE('',(#2392),#1742,.F.);
#15703=ADVANCED_FACE('',(#2393),#1743,.F.);
#15704=ADVANCED_FACE('',(#2394),#1744,.F.);
#15705=ADVANCED_FACE('',(#2395),#1745,.T.);
#15706=ADVANCED_FACE('',(#2396),#1746,.F.);
#15707=ADVANCED_FACE('',(#2397),#1747,.F.);
#15708=ADVANCED_FACE('',(#2398),#1748,.F.);
#15709=ADVANCED_FACE('',(#2399),#1749,.F.);
#15710=ADVANCED_FACE('',(#2400),#1750,.T.);
#15711=ADVANCED_FACE('',(#2401),#1751,.F.);
#15712=ADVANCED_FACE('',(#2402),#1752,.F.);
#15713=ADVANCED_FACE('',(#2403),#1753,.F.);
#15714=ADVANCED_FACE('',(#2404),#1754,.F.);
#15715=ADVANCED_FACE('',(#2405),#1755,.T.);
#15716=ADVANCED_FACE('',(#2406),#1756,.F.);
#15717=ADVANCED_FACE('',(#2407),#1757,.F.);
#15718=ADVANCED_FACE('',(#2408),#1758,.F.);
#15719=ADVANCED_FACE('',(#2409),#1759,.F.);
#15720=ADVANCED_FACE('',(#2410),#1760,.T.);
#15721=ADVANCED_FACE('',(#2411),#1761,.F.);
#15722=ADVANCED_FACE('',(#2412),#1762,.F.);
#15723=ADVANCED_FACE('',(#2413),#1763,.F.);
#15724=ADVANCED_FACE('',(#2414),#1764,.F.);
#15725=ADVANCED_FACE('',(#2415),#1765,.T.);
#15726=ADVANCED_FACE('',(#2416),#1766,.F.);
#15727=ADVANCED_FACE('',(#2417),#1767,.F.);
#15728=ADVANCED_FACE('',(#2418),#1768,.F.);
#15729=ADVANCED_FACE('',(#2419),#1769,.F.);
#15730=ADVANCED_FACE('',(#2420),#1770,.T.);
#15731=ADVANCED_FACE('',(#2421),#1771,.F.);
#15732=ADVANCED_FACE('',(#2422),#1772,.F.);
#15733=ADVANCED_FACE('',(#2423),#1773,.F.);
#15734=ADVANCED_FACE('',(#2424),#1774,.F.);
#15735=ADVANCED_FACE('',(#2425),#1775,.T.);
#15736=ADVANCED_FACE('',(#2426),#1776,.F.);
#15737=ADVANCED_FACE('',(#2427),#1777,.F.);
#15738=ADVANCED_FACE('',(#2428),#1778,.F.);
#15739=ADVANCED_FACE('',(#2429),#1779,.F.);
#15740=ADVANCED_FACE('',(#2430),#1780,.T.);
#15741=ADVANCED_FACE('',(#2431),#1781,.F.);
#15742=ADVANCED_FACE('',(#2432),#1782,.F.);
#15743=ADVANCED_FACE('',(#2433),#1783,.F.);
#15744=ADVANCED_FACE('',(#2434),#1784,.F.);
#15745=ADVANCED_FACE('',(#2435),#1785,.T.);
#15746=ADVANCED_FACE('',(#2436),#1786,.F.);
#15747=ADVANCED_FACE('',(#2437),#1787,.F.);
#15748=ADVANCED_FACE('',(#2438),#1788,.F.);
#15749=ADVANCED_FACE('',(#2439),#1789,.F.);
#15750=ADVANCED_FACE('',(#2440),#1790,.T.);
#15751=ADVANCED_FACE('',(#2441),#1791,.F.);
#15752=ADVANCED_FACE('',(#2442),#1792,.F.);
#15753=ADVANCED_FACE('',(#2443),#1793,.F.);
#15754=ADVANCED_FACE('',(#2444),#1794,.F.);
#15755=ADVANCED_FACE('',(#2445),#1795,.T.);
#15756=ADVANCED_FACE('',(#2446),#1796,.F.);
#15757=ADVANCED_FACE('',(#2447),#1797,.F.);
#15758=ADVANCED_FACE('',(#2448),#1798,.F.);
#15759=ADVANCED_FACE('',(#2449),#1799,.F.);
#15760=ADVANCED_FACE('',(#2450),#1800,.T.);
#15761=ADVANCED_FACE('',(#2451),#1801,.F.);
#15762=ADVANCED_FACE('',(#2452),#1802,.F.);
#15763=ADVANCED_FACE('',(#2453),#1803,.F.);
#15764=ADVANCED_FACE('',(#2454),#1804,.F.);
#15765=ADVANCED_FACE('',(#2455),#1805,.T.);
#15766=ADVANCED_FACE('',(#2456),#1806,.F.);
#15767=ADVANCED_FACE('',(#2457),#1807,.F.);
#15768=ADVANCED_FACE('',(#2458),#1808,.F.);
#15769=ADVANCED_FACE('',(#2459),#1809,.F.);
#15770=ADVANCED_FACE('',(#2460),#1810,.T.);
#15771=ADVANCED_FACE('',(#2461),#1811,.F.);
#15772=ADVANCED_FACE('',(#2462),#1812,.F.);
#15773=ADVANCED_FACE('',(#2463),#1813,.F.);
#15774=ADVANCED_FACE('',(#2464),#1814,.F.);
#15775=ADVANCED_FACE('',(#2465),#1815,.T.);
#15776=ADVANCED_FACE('',(#2466),#1816,.F.);
#15777=ADVANCED_FACE('',(#2467),#1817,.F.);
#15778=ADVANCED_FACE('',(#2468),#1818,.F.);
#15779=ADVANCED_FACE('',(#2469),#1819,.F.);
#15780=ADVANCED_FACE('',(#2470),#1820,.T.);
#15781=ADVANCED_FACE('',(#2471),#1821,.F.);
#15782=ADVANCED_FACE('',(#2472),#1822,.F.);
#15783=ADVANCED_FACE('',(#2473),#1823,.F.);
#15784=ADVANCED_FACE('',(#2474),#1824,.F.);
#15785=ADVANCED_FACE('',(#2475),#1825,.T.);
#15786=ADVANCED_FACE('',(#2476),#1826,.F.);
#15787=ADVANCED_FACE('',(#2477),#1827,.F.);
#15788=ADVANCED_FACE('',(#2478),#1828,.F.);
#15789=ADVANCED_FACE('',(#2479),#1829,.F.);
#15790=ADVANCED_FACE('',(#2480),#1830,.T.);
#15791=ADVANCED_FACE('',(#2481),#1831,.F.);
#15792=ADVANCED_FACE('',(#2482),#1832,.F.);
#15793=ADVANCED_FACE('',(#2483),#1833,.F.);
#15794=ADVANCED_FACE('',(#2484),#1834,.F.);
#15795=ADVANCED_FACE('',(#2485),#1835,.T.);
#15796=ADVANCED_FACE('',(#2486),#1836,.F.);
#15797=ADVANCED_FACE('',(#2487),#1837,.F.);
#15798=ADVANCED_FACE('',(#2488),#1838,.F.);
#15799=ADVANCED_FACE('',(#2489),#1839,.F.);
#15800=ADVANCED_FACE('',(#2490),#1840,.T.);
#15801=ADVANCED_FACE('',(#2491),#1841,.F.);
#15802=ADVANCED_FACE('',(#2492),#1842,.F.);
#15803=ADVANCED_FACE('',(#2493),#1843,.F.);
#15804=ADVANCED_FACE('',(#2494),#1844,.F.);
#15805=ADVANCED_FACE('',(#2495),#1845,.T.);
#15806=ADVANCED_FACE('',(#2496),#15279,.F.);
#15807=ADVANCED_FACE('',(#2497),#15280,.F.);
#15808=ADVANCED_FACE('',(#2498),#15281,.F.);
#15809=ADVANCED_FACE('',(#2499),#1846,.T.);
#15810=ADVANCED_FACE('',(#2500),#1847,.T.);
#15811=ADVANCED_FACE('',(#2501),#1848,.T.);
#15812=ADVANCED_FACE('',(#2502),#1849,.T.);
#15813=ADVANCED_FACE('',(#2503),#1850,.T.);
#15814=ADVANCED_FACE('',(#2504),#1851,.T.);
#15815=ADVANCED_FACE('',(#2505,#1506,#1507,#1508),#1852,.F.);
#15816=ADVANCED_FACE('',(#2506),#1853,.T.);
#15817=ADVANCED_FACE('',(#2507,#1509,#1510,#1511,#1512,#1513,#1514,#1515,
#1516,#1517,#1518,#1519,#1520,#1521,#1522,#1523,#1524,#1525,#1526,#1527,
#1528,#1529,#1530,#1531,#1532,#1533,#1534,#1535),#1854,.T.);
#15818=ADVANCED_FACE('',(#2508),#15282,.T.);
#15819=ADVANCED_FACE('',(#2509),#15283,.F.);
#15820=ADVANCED_FACE('',(#2510),#15284,.T.);
#15821=ADVANCED_FACE('',(#2511,#1536),#1855,.T.);
#15822=ADVANCED_FACE('',(#2512,#1537),#1856,.F.);
#15823=ADVANCED_FACE('',(#2513),#15285,.F.);
#15824=ADVANCED_FACE('',(#2514),#15286,.T.);
#15825=ADVANCED_FACE('',(#2515,#1538),#1857,.T.);
#15826=ADVANCED_FACE('',(#2516,#1539),#1858,.F.);
#15827=ADVANCED_FACE('',(#2517),#1859,.T.);
#15828=ADVANCED_FACE('',(#2518),#1860,.T.);
#15829=ADVANCED_FACE('',(#2519),#1861,.T.);
#15830=ADVANCED_FACE('',(#2520),#1862,.T.);
#15831=ADVANCED_FACE('',(#2521),#1863,.T.);
#15832=ADVANCED_FACE('',(#2522),#1864,.F.);
#15833=ADVANCED_FACE('',(#2523),#1865,.T.);
#15834=ADVANCED_FACE('',(#2524),#1866,.T.);
#15835=ADVANCED_FACE('',(#2525),#1867,.T.);
#15836=ADVANCED_FACE('',(#2526),#1868,.T.);
#15837=ADVANCED_FACE('',(#2527),#1869,.T.);
#15838=ADVANCED_FACE('',(#2528),#1870,.F.);
#15839=ADVANCED_FACE('',(#2529),#1871,.F.);
#15840=ADVANCED_FACE('',(#2530),#1872,.F.);
#15841=ADVANCED_FACE('',(#2531),#1873,.F.);
#15842=ADVANCED_FACE('',(#2532),#1874,.F.);
#15843=ADVANCED_FACE('',(#2533),#1875,.F.);
#15844=ADVANCED_FACE('',(#2534),#1876,.F.);
#15845=ADVANCED_FACE('',(#2535),#1877,.F.);
#15846=ADVANCED_FACE('',(#2536),#1878,.F.);
#15847=ADVANCED_FACE('',(#2537,#1540),#1879,.T.);
#15848=ADVANCED_FACE('',(#2538),#15287,.T.);
#15849=ADVANCED_FACE('',(#2539),#1880,.F.);
#15850=ADVANCED_FACE('',(#2540),#1881,.T.);
#15851=ADVANCED_FACE('',(#2541),#1039,.T.);
#15852=ADVANCED_FACE('',(#2542),#15288,.T.);
#15853=ADVANCED_FACE('',(#2543),#1040,.T.);
#15854=ADVANCED_FACE('',(#2544,#1541),#1882,.T.);
#15855=ADVANCED_FACE('',(#2545),#1041,.T.);
#15856=ADVANCED_FACE('',(#2546),#15289,.T.);
#15857=ADVANCED_FACE('',(#2547),#15290,.F.);
#15858=ADVANCED_FACE('',(#2548),#1883,.T.);
#15859=ADVANCED_FACE('',(#2549),#1884,.F.);
#15860=ADVANCED_FACE('',(#2550),#1885,.T.);
#15861=ADVANCED_FACE('',(#2551),#1886,.F.);
#15862=ADVANCED_FACE('',(#2552),#1887,.F.);
#15863=ADVANCED_FACE('',(#2553),#1888,.F.);
#15864=ADVANCED_FACE('',(#2554),#1889,.F.);
#15865=ADVANCED_FACE('',(#2555),#1890,.T.);
#15866=ADVANCED_FACE('',(#2556),#1891,.F.);
#15867=ADVANCED_FACE('',(#2557),#1892,.F.);
#15868=ADVANCED_FACE('',(#2558),#1893,.F.);
#15869=ADVANCED_FACE('',(#2559,#1542),#1894,.T.);
#15870=ADVANCED_FACE('',(#2560,#1543),#1895,.F.);
#15871=ADVANCED_FACE('',(#2561),#15291,.T.);
#15872=ADVANCED_FACE('',(#2562),#15292,.T.);
#15873=ADVANCED_FACE('',(#2563,#1544,#1545),#15293,.T.);
#15874=ADVANCED_FACE('',(#2564,#1546),#1896,.T.);
#15875=ADVANCED_FACE('',(#2565),#1897,.F.);
#15876=ADVANCED_FACE('',(#2566),#15294,.F.);
#15877=ADVANCED_FACE('',(#2567),#15295,.T.);
#15878=ADVANCED_FACE('',(#2568,#1547),#1898,.T.);
#15879=ADVANCED_FACE('',(#2569,#1548),#1899,.F.);
#15880=ADVANCED_FACE('',(#2570),#15296,.F.);
#15881=ADVANCED_FACE('',(#2571),#15297,.T.);
#15882=ADVANCED_FACE('',(#2572,#1549),#1900,.T.);
#15883=ADVANCED_FACE('',(#2573,#1550),#1901,.F.);
#15884=ADVANCED_FACE('',(#2574),#1902,.T.);
#15885=ADVANCED_FACE('',(#2575),#15298,.F.);
#15886=ADVANCED_FACE('',(#2576),#1903,.T.);
#15887=ADVANCED_FACE('',(#2577,#1551),#15299,.F.);
#15888=ADVANCED_FACE('',(#2578,#1552),#15300,.T.);
#15889=ADVANCED_FACE('',(#2579,#1553),#1904,.T.);
#15890=ADVANCED_FACE('',(#2580,#1554),#1905,.F.);
#15891=ADVANCED_FACE('',(#2581),#15301,.F.);
#15892=ADVANCED_FACE('',(#2582),#1906,.F.);
#15893=ADVANCED_FACE('',(#2583),#1907,.F.);
#15894=ADVANCED_FACE('',(#2584),#1908,.F.);
#15895=ADVANCED_FACE('',(#2585,#1555),#1909,.T.);
#15896=ADVANCED_FACE('',(#2586),#15302,.F.);
#15897=ADVANCED_FACE('',(#2587),#15303,.T.);
#15898=ADVANCED_FACE('',(#2588,#1556),#1910,.F.);
#15899=ADVANCED_FACE('',(#2589),#1911,.T.);
#15900=ADVANCED_FACE('',(#2590,#1557),#1912,.T.);
#15901=ADVANCED_FACE('',(#2591),#1913,.T.);
#15902=ADVANCED_FACE('',(#2592,#1558),#15304,.T.);
#15903=ADVANCED_FACE('',(#2593,#1559),#1914,.F.);
#15904=ADVANCED_FACE('',(#2594),#15305,.F.);
#15905=ADVANCED_FACE('',(#2595),#15306,.T.);
#15906=ADVANCED_FACE('',(#2596,#1560),#1915,.T.);
#15907=ADVANCED_FACE('',(#2597,#1561),#1916,.F.);
#15908=ADVANCED_FACE('',(#2598),#15307,.F.);
#15909=ADVANCED_FACE('',(#2599),#15308,.T.);
#15910=ADVANCED_FACE('',(#2600,#1562),#1917,.T.);
#15911=ADVANCED_FACE('',(#2601,#1563),#1918,.F.);
#15912=ADVANCED_FACE('',(#2602),#15309,.F.);
#15913=ADVANCED_FACE('',(#2603),#15310,.T.);
#15914=ADVANCED_FACE('',(#2604,#1564),#1919,.T.);
#15915=ADVANCED_FACE('',(#2605,#1565),#1920,.F.);
#15916=ADVANCED_FACE('',(#2606),#15311,.F.);
#15917=ADVANCED_FACE('',(#2607),#15312,.T.);
#15918=ADVANCED_FACE('',(#2608,#1566),#1921,.T.);
#15919=ADVANCED_FACE('',(#2609,#1567),#1922,.F.);
#15920=ADVANCED_FACE('',(#2610),#15313,.F.);
#15921=ADVANCED_FACE('',(#2611),#15314,.T.);
#15922=ADVANCED_FACE('',(#2612,#1568),#1923,.T.);
#15923=ADVANCED_FACE('',(#2613,#1569),#1924,.F.);
#15924=ADVANCED_FACE('',(#2614),#1925,.F.);
#15925=ADVANCED_FACE('',(#2615),#1926,.F.);
#15926=ADVANCED_FACE('',(#2616),#1927,.F.);
#15927=ADVANCED_FACE('',(#2617),#1928,.F.);
#15928=ADVANCED_FACE('',(#2618),#1929,.F.);
#15929=ADVANCED_FACE('',(#2619),#1930,.F.);
#15930=ADVANCED_FACE('',(#2620),#1931,.F.);
#15931=ADVANCED_FACE('',(#2621),#1932,.F.);
#15932=ADVANCED_FACE('',(#2622,#1570),#1933,.T.);
#15933=ADVANCED_FACE('',(#2623),#15315,.T.);
#15934=ADVANCED_FACE('',(#2624),#1934,.F.);
#15935=ADVANCED_FACE('',(#2625),#1935,.T.);
#15936=ADVANCED_FACE('',(#2626),#1042,.T.);
#15937=ADVANCED_FACE('',(#2627),#15316,.T.);
#15938=ADVANCED_FACE('',(#2628),#1043,.T.);
#15939=ADVANCED_FACE('',(#2629,#1571),#1936,.T.);
#15940=ADVANCED_FACE('',(#2630),#1044,.T.);
#15941=ADVANCED_FACE('',(#2631),#15317,.T.);
#15942=ADVANCED_FACE('',(#2632),#15318,.F.);
#15943=ADVANCED_FACE('',(#2633),#1937,.T.);
#15944=ADVANCED_FACE('',(#2634),#1938,.F.);
#15945=ADVANCED_FACE('',(#2635),#1939,.T.);
#15946=ADVANCED_FACE('',(#2636),#1940,.F.);
#15947=ADVANCED_FACE('',(#2637),#1941,.F.);
#15948=ADVANCED_FACE('',(#2638),#1942,.F.);
#15949=ADVANCED_FACE('',(#2639,#1572),#1943,.T.);
#15950=ADVANCED_FACE('',(#2640,#1573),#1944,.F.);
#15951=ADVANCED_FACE('',(#2641),#15319,.T.);
#15952=ADVANCED_FACE('',(#2642),#15320,.T.);
#15953=ADVANCED_FACE('',(#2643,#1574),#15321,.T.);
#15954=ADVANCED_FACE('',(#2644,#1575),#1945,.T.);
#15955=ADVANCED_FACE('',(#2645),#1946,.F.);
#15956=ADVANCED_FACE('',(#2646),#15322,.F.);
#15957=ADVANCED_FACE('',(#2647),#15323,.T.);
#15958=ADVANCED_FACE('',(#2648,#1576),#1947,.T.);
#15959=ADVANCED_FACE('',(#2649,#1577),#1948,.F.);
#15960=ADVANCED_FACE('',(#2650),#15324,.F.);
#15961=ADVANCED_FACE('',(#2651),#15325,.T.);
#15962=ADVANCED_FACE('',(#2652,#1578),#1949,.T.);
#15963=ADVANCED_FACE('',(#2653,#1579),#1950,.F.);
#15964=ADVANCED_FACE('',(#2654),#1951,.T.);
#15965=ADVANCED_FACE('',(#2655),#15326,.F.);
#15966=ADVANCED_FACE('',(#2656),#1952,.T.);
#15967=ADVANCED_FACE('',(#2657,#1580),#15327,.F.);
#15968=ADVANCED_FACE('',(#2658,#1581),#15328,.T.);
#15969=ADVANCED_FACE('',(#2659,#1582),#1953,.T.);
#15970=ADVANCED_FACE('',(#2660,#1583),#1954,.F.);
#15971=ADVANCED_FACE('',(#2661),#15329,.F.);
#15972=ADVANCED_FACE('',(#2662),#15330,.T.);
#15973=ADVANCED_FACE('',(#2663,#1584),#1955,.T.);
#15974=ADVANCED_FACE('',(#2664,#1585),#1956,.F.);
#15975=ADVANCED_FACE('',(#2665),#15331,.F.);
#15976=ADVANCED_FACE('',(#2666),#1957,.T.);
#15977=ADVANCED_FACE('',(#2667),#1958,.F.);
#15978=ADVANCED_FACE('',(#2668),#1959,.T.);
#15979=ADVANCED_FACE('',(#2669),#1960,.F.);
#15980=ADVANCED_FACE('',(#2670),#1961,.F.);
#15981=ADVANCED_FACE('',(#2671),#1962,.F.);
#15982=ADVANCED_FACE('',(#2672,#1586),#1963,.T.);
#15983=ADVANCED_FACE('',(#2673,#1587),#1964,.F.);
#15984=ADVANCED_FACE('',(#2674),#15332,.T.);
#15985=ADVANCED_FACE('',(#2675),#15333,.T.);
#15986=ADVANCED_FACE('',(#2676,#1588),#15334,.T.);
#15987=ADVANCED_FACE('',(#2677,#1589),#1965,.T.);
#15988=ADVANCED_FACE('',(#2678),#1966,.F.);
#15989=ADVANCED_FACE('',(#2679),#15335,.F.);
#15990=ADVANCED_FACE('',(#2680),#15336,.T.);
#15991=ADVANCED_FACE('',(#2681,#1590),#1967,.T.);
#15992=ADVANCED_FACE('',(#2682,#1591),#1968,.F.);
#15993=ADVANCED_FACE('',(#2683),#15337,.F.);
#15994=ADVANCED_FACE('',(#2684),#15338,.T.);
#15995=ADVANCED_FACE('',(#2685,#1592),#1969,.T.);
#15996=ADVANCED_FACE('',(#2686,#1593),#1970,.F.);
#15997=ADVANCED_FACE('',(#2687),#1971,.T.);
#15998=ADVANCED_FACE('',(#2688),#15339,.F.);
#15999=ADVANCED_FACE('',(#2689),#1972,.T.);
#16000=ADVANCED_FACE('',(#2690,#1594),#15340,.F.);
#16001=ADVANCED_FACE('',(#2691,#1595),#15341,.T.);
#16002=ADVANCED_FACE('',(#2692,#1596),#1973,.T.);
#16003=ADVANCED_FACE('',(#2693,#1597),#1974,.F.);
#16004=ADVANCED_FACE('',(#2694),#15342,.F.);
#16005=ADVANCED_FACE('',(#2695),#15343,.T.);
#16006=ADVANCED_FACE('',(#2696,#1598),#1975,.T.);
#16007=ADVANCED_FACE('',(#2697,#1599),#1976,.F.);
#16008=ADVANCED_FACE('',(#2698),#1977,.F.);
#16009=ADVANCED_FACE('',(#2699),#1978,.F.);
#16010=ADVANCED_FACE('',(#2700),#1979,.F.);
#16011=ADVANCED_FACE('',(#2701,#1600),#1980,.F.);
#16012=ADVANCED_FACE('',(#2702),#15344,.F.);
#16013=ADVANCED_FACE('',(#2703),#15345,.T.);
#16014=ADVANCED_FACE('',(#2704,#1601),#1981,.T.);
#16015=ADVANCED_FACE('',(#2705),#11,.T.);
#16016=ADVANCED_FACE('',(#2706),#1982,.T.);
#16017=ADVANCED_FACE('',(#2707),#12,.T.);
#16018=ADVANCED_FACE('',(#2708),#15346,.T.);
#16019=ADVANCED_FACE('',(#2709),#13,.T.);
#16020=ADVANCED_FACE('',(#2710),#1983,.T.);
#16021=ADVANCED_FACE('',(#2711),#14,.T.);
#16022=ADVANCED_FACE('',(#2712),#15347,.T.);
#16023=ADVANCED_FACE('',(#2713),#15,.T.);
#16024=ADVANCED_FACE('',(#2714),#1984,.T.);
#16025=ADVANCED_FACE('',(#2715),#16,.T.);
#16026=ADVANCED_FACE('',(#2716),#15348,.T.);
#16027=ADVANCED_FACE('',(#2717),#17,.T.);
#16028=ADVANCED_FACE('',(#2718),#1985,.T.);
#16029=ADVANCED_FACE('',(#2719),#18,.T.);
#16030=ADVANCED_FACE('',(#2720),#15349,.T.);
#16031=ADVANCED_FACE('',(#2721),#19,.T.);
#16032=ADVANCED_FACE('',(#2722),#1986,.T.);
#16033=ADVANCED_FACE('',(#2723),#20,.T.);
#16034=ADVANCED_FACE('',(#2724),#15350,.T.);
#16035=ADVANCED_FACE('',(#2725),#21,.T.);
#16036=ADVANCED_FACE('',(#2726),#1987,.T.);
#16037=ADVANCED_FACE('',(#2727),#22,.T.);
#16038=ADVANCED_FACE('',(#2728),#15351,.T.);
#16039=ADVANCED_FACE('',(#2729),#23,.T.);
#16040=ADVANCED_FACE('',(#2730),#1988,.T.);
#16041=ADVANCED_FACE('',(#2731),#24,.T.);
#16042=ADVANCED_FACE('',(#2732),#15352,.T.);
#16043=ADVANCED_FACE('',(#2733),#25,.T.);
#16044=ADVANCED_FACE('',(#2734),#1989,.T.);
#16045=ADVANCED_FACE('',(#2735),#26,.T.);
#16046=ADVANCED_FACE('',(#2736),#15353,.T.);
#16047=ADVANCED_FACE('',(#2737),#27,.T.);
#16048=ADVANCED_FACE('',(#2738),#1990,.T.);
#16049=ADVANCED_FACE('',(#2739),#28,.T.);
#16050=ADVANCED_FACE('',(#2740),#15354,.T.);
#16051=ADVANCED_FACE('',(#2741),#29,.T.);
#16052=ADVANCED_FACE('',(#2742),#1991,.T.);
#16053=ADVANCED_FACE('',(#2743),#30,.T.);
#16054=ADVANCED_FACE('',(#2744),#15355,.T.);
#16055=ADVANCED_FACE('',(#2745),#31,.T.);
#16056=ADVANCED_FACE('',(#2746),#1992,.T.);
#16057=ADVANCED_FACE('',(#2747),#32,.T.);
#16058=ADVANCED_FACE('',(#2748),#15356,.T.);
#16059=ADVANCED_FACE('',(#2749),#33,.T.);
#16060=ADVANCED_FACE('',(#2750),#1993,.T.);
#16061=ADVANCED_FACE('',(#2751),#34,.T.);
#16062=ADVANCED_FACE('',(#2752),#15357,.T.);
#16063=ADVANCED_FACE('',(#2753),#35,.T.);
#16064=ADVANCED_FACE('',(#2754),#1994,.T.);
#16065=ADVANCED_FACE('',(#2755),#36,.T.);
#16066=ADVANCED_FACE('',(#2756),#15358,.T.);
#16067=ADVANCED_FACE('',(#2757),#37,.T.);
#16068=ADVANCED_FACE('',(#2758),#1995,.T.);
#16069=ADVANCED_FACE('',(#2759),#38,.T.);
#16070=ADVANCED_FACE('',(#2760),#15359,.T.);
#16071=ADVANCED_FACE('',(#2761),#39,.T.);
#16072=ADVANCED_FACE('',(#2762),#1996,.T.);
#16073=ADVANCED_FACE('',(#2763),#40,.T.);
#16074=ADVANCED_FACE('',(#2764),#15360,.T.);
#16075=ADVANCED_FACE('',(#2765),#41,.T.);
#16076=ADVANCED_FACE('',(#2766),#1997,.T.);
#16077=ADVANCED_FACE('',(#2767),#42,.T.);
#16078=ADVANCED_FACE('',(#2768),#15361,.T.);
#16079=ADVANCED_FACE('',(#2769),#43,.T.);
#16080=ADVANCED_FACE('',(#2770),#1998,.T.);
#16081=ADVANCED_FACE('',(#2771),#44,.T.);
#16082=ADVANCED_FACE('',(#2772),#15362,.T.);
#16083=ADVANCED_FACE('',(#2773),#45,.T.);
#16084=ADVANCED_FACE('',(#2774),#1999,.T.);
#16085=ADVANCED_FACE('',(#2775),#46,.T.);
#16086=ADVANCED_FACE('',(#2776),#15363,.T.);
#16087=ADVANCED_FACE('',(#2777),#47,.T.);
#16088=ADVANCED_FACE('',(#2778),#2000,.T.);
#16089=ADVANCED_FACE('',(#2779),#48,.T.);
#16090=ADVANCED_FACE('',(#2780),#15364,.T.);
#16091=ADVANCED_FACE('',(#2781),#49,.T.);
#16092=ADVANCED_FACE('',(#2782),#2001,.T.);
#16093=ADVANCED_FACE('',(#2783),#50,.T.);
#16094=ADVANCED_FACE('',(#2784,#1602),#2002,.T.);
#16095=ADVANCED_FACE('',(#2785),#15365,.T.);
#16096=ADVANCED_FACE('',(#2786),#2003,.T.);
#16097=ADVANCED_FACE('',(#2787),#2004,.T.);
#16098=ADVANCED_FACE('',(#2788),#2005,.T.);
#16099=ADVANCED_FACE('',(#2789),#2006,.T.);
#16100=ADVANCED_FACE('',(#2790),#2007,.T.);
#16101=ADVANCED_FACE('',(#2791),#2008,.F.);
#16102=ADVANCED_FACE('',(#2792),#2009,.T.);
#16103=ADVANCED_FACE('',(#2793),#2010,.T.);
#16104=ADVANCED_FACE('',(#2794),#2011,.T.);
#16105=ADVANCED_FACE('',(#2795),#2012,.F.);
#16106=ADVANCED_FACE('',(#2796),#15366,.F.);
#16107=ADVANCED_FACE('',(#2797),#2013,.T.);
#16108=ADVANCED_FACE('',(#2798),#2014,.F.);
#16109=ADVANCED_FACE('',(#2799),#2015,.T.);
#16110=ADVANCED_FACE('',(#2800),#2016,.F.);
#16111=ADVANCED_FACE('',(#2801),#2017,.F.);
#16112=ADVANCED_FACE('',(#2802),#2018,.F.);
#16113=ADVANCED_FACE('',(#2803,#1603),#2019,.T.);
#16114=ADVANCED_FACE('',(#2804,#1604),#2020,.F.);
#16115=ADVANCED_FACE('',(#2805),#15367,.T.);
#16116=ADVANCED_FACE('',(#2806),#15368,.T.);
#16117=ADVANCED_FACE('',(#2807,#1605),#15369,.T.);
#16118=ADVANCED_FACE('',(#2808,#1606),#2021,.T.);
#16119=ADVANCED_FACE('',(#2809),#2022,.F.);
#16120=ADVANCED_FACE('',(#2810),#15370,.F.);
#16121=ADVANCED_FACE('',(#2811),#15371,.T.);
#16122=ADVANCED_FACE('',(#2812,#1607),#2023,.T.);
#16123=ADVANCED_FACE('',(#2813,#1608),#2024,.F.);
#16124=ADVANCED_FACE('',(#2814),#15372,.F.);
#16125=ADVANCED_FACE('',(#2815),#15373,.T.);
#16126=ADVANCED_FACE('',(#2816,#1609),#2025,.T.);
#16127=ADVANCED_FACE('',(#2817,#1610),#2026,.F.);
#16128=ADVANCED_FACE('',(#2818),#2027,.T.);
#16129=ADVANCED_FACE('',(#2819),#15374,.F.);
#16130=ADVANCED_FACE('',(#2820),#2028,.T.);
#16131=ADVANCED_FACE('',(#2821,#1611),#15375,.F.);
#16132=ADVANCED_FACE('',(#2822,#1612),#15376,.T.);
#16133=ADVANCED_FACE('',(#2823,#1613),#2029,.T.);
#16134=ADVANCED_FACE('',(#2824,#1614),#2030,.F.);
#16135=ADVANCED_FACE('',(#2825),#15377,.F.);
#16136=ADVANCED_FACE('',(#2826),#15378,.T.);
#16137=ADVANCED_FACE('',(#2827,#1615),#2031,.T.);
#16138=ADVANCED_FACE('',(#2828,#1616),#2032,.F.);
#16139=ADVANCED_FACE('',(#2829),#15379,.F.);
#16140=ADVANCED_FACE('',(#2830),#15380,.T.);
#16141=ADVANCED_FACE('',(#2831,#1617),#2033,.T.);
#16142=ADVANCED_FACE('',(#2832,#1618),#2034,.F.);
#16143=ADVANCED_FACE('',(#2833),#2035,.T.);
#16144=ADVANCED_FACE('',(#2834),#15381,.F.);
#16145=ADVANCED_FACE('',(#2835),#2036,.T.);
#16146=ADVANCED_FACE('',(#2836),#2037,.T.);
#16147=ADVANCED_FACE('',(#2837),#2038,.F.);
#16148=ADVANCED_FACE('',(#2838),#2039,.T.);
#16149=ADVANCED_FACE('',(#2839),#2040,.T.);
#16150=ADVANCED_FACE('',(#2840,#1619),#15382,.F.);
#16151=ADVANCED_FACE('',(#2841,#1620,#1621),#15383,.T.);
#16152=ADVANCED_FACE('',(#2842,#1622),#2041,.T.);
#16153=ADVANCED_FACE('',(#2843,#1623),#2042,.F.);
#16154=ADVANCED_FACE('',(#2844),#15384,.F.);
#16155=ADVANCED_FACE('',(#2845),#15385,.T.);
#16156=ADVANCED_FACE('',(#2846,#1624),#2043,.T.);
#16157=ADVANCED_FACE('',(#2847,#1625),#2044,.F.);
#16158=ADVANCED_FACE('',(#2848),#2045,.F.);
#16159=ADVANCED_FACE('',(#2849),#2046,.F.);
#16160=ADVANCED_FACE('',(#2850),#2047,.F.);
#16161=ADVANCED_FACE('',(#2851,#1626),#2048,.F.);
#16162=ADVANCED_FACE('',(#2852),#15386,.F.);
#16163=ADVANCED_FACE('',(#2853),#15387,.T.);
#16164=ADVANCED_FACE('',(#2854,#1627),#2049,.T.);
#16165=ADVANCED_FACE('',(#2855),#51,.T.);
#16166=ADVANCED_FACE('',(#2856),#52,.T.);
#16167=ADVANCED_FACE('',(#2857),#2050,.T.);
#16168=ADVANCED_FACE('',(#2858),#15388,.T.);
#16169=ADVANCED_FACE('',(#2859),#53,.T.);
#16170=ADVANCED_FACE('',(#2860),#54,.T.);
#16171=ADVANCED_FACE('',(#2861),#2051,.T.);
#16172=ADVANCED_FACE('',(#2862),#15389,.T.);
#16173=ADVANCED_FACE('',(#2863),#55,.T.);
#16174=ADVANCED_FACE('',(#2864),#56,.T.);
#16175=ADVANCED_FACE('',(#2865),#2052,.T.);
#16176=ADVANCED_FACE('',(#2866),#15390,.T.);
#16177=ADVANCED_FACE('',(#2867),#57,.T.);
#16178=ADVANCED_FACE('',(#2868),#58,.T.);
#16179=ADVANCED_FACE('',(#2869),#2053,.T.);
#16180=ADVANCED_FACE('',(#2870),#15391,.T.);
#16181=ADVANCED_FACE('',(#2871),#59,.T.);
#16182=ADVANCED_FACE('',(#2872),#60,.T.);
#16183=ADVANCED_FACE('',(#2873),#2054,.T.);
#16184=ADVANCED_FACE('',(#2874),#15392,.T.);
#16185=ADVANCED_FACE('',(#2875),#61,.T.);
#16186=ADVANCED_FACE('',(#2876),#62,.T.);
#16187=ADVANCED_FACE('',(#2877),#2055,.T.);
#16188=ADVANCED_FACE('',(#2878),#15393,.T.);
#16189=ADVANCED_FACE('',(#2879),#63,.T.);
#16190=ADVANCED_FACE('',(#2880),#64,.T.);
#16191=ADVANCED_FACE('',(#2881),#2056,.T.);
#16192=ADVANCED_FACE('',(#2882),#15394,.T.);
#16193=ADVANCED_FACE('',(#2883),#65,.T.);
#16194=ADVANCED_FACE('',(#2884),#66,.T.);
#16195=ADVANCED_FACE('',(#2885),#2057,.T.);
#16196=ADVANCED_FACE('',(#2886),#15395,.T.);
#16197=ADVANCED_FACE('',(#2887),#67,.T.);
#16198=ADVANCED_FACE('',(#2888),#68,.T.);
#16199=ADVANCED_FACE('',(#2889),#2058,.T.);
#16200=ADVANCED_FACE('',(#2890),#15396,.T.);
#16201=ADVANCED_FACE('',(#2891),#69,.T.);
#16202=ADVANCED_FACE('',(#2892),#70,.T.);
#16203=ADVANCED_FACE('',(#2893),#2059,.T.);
#16204=ADVANCED_FACE('',(#2894),#15397,.T.);
#16205=ADVANCED_FACE('',(#2895),#71,.T.);
#16206=ADVANCED_FACE('',(#2896),#72,.T.);
#16207=ADVANCED_FACE('',(#2897),#2060,.T.);
#16208=ADVANCED_FACE('',(#2898),#15398,.T.);
#16209=ADVANCED_FACE('',(#2899),#73,.T.);
#16210=ADVANCED_FACE('',(#2900),#74,.T.);
#16211=ADVANCED_FACE('',(#2901),#2061,.T.);
#16212=ADVANCED_FACE('',(#2902),#15399,.T.);
#16213=ADVANCED_FACE('',(#2903),#75,.T.);
#16214=ADVANCED_FACE('',(#2904),#76,.T.);
#16215=ADVANCED_FACE('',(#2905),#2062,.T.);
#16216=ADVANCED_FACE('',(#2906),#15400,.T.);
#16217=ADVANCED_FACE('',(#2907),#77,.T.);
#16218=ADVANCED_FACE('',(#2908),#78,.T.);
#16219=ADVANCED_FACE('',(#2909),#2063,.T.);
#16220=ADVANCED_FACE('',(#2910),#15401,.T.);
#16221=ADVANCED_FACE('',(#2911),#79,.T.);
#16222=ADVANCED_FACE('',(#2912),#80,.T.);
#16223=ADVANCED_FACE('',(#2913),#2064,.T.);
#16224=ADVANCED_FACE('',(#2914),#15402,.T.);
#16225=ADVANCED_FACE('',(#2915),#81,.T.);
#16226=ADVANCED_FACE('',(#2916),#82,.T.);
#16227=ADVANCED_FACE('',(#2917),#2065,.T.);
#16228=ADVANCED_FACE('',(#2918),#15403,.T.);
#16229=ADVANCED_FACE('',(#2919),#83,.T.);
#16230=ADVANCED_FACE('',(#2920),#84,.T.);
#16231=ADVANCED_FACE('',(#2921),#2066,.T.);
#16232=ADVANCED_FACE('',(#2922),#15404,.T.);
#16233=ADVANCED_FACE('',(#2923),#85,.T.);
#16234=ADVANCED_FACE('',(#2924),#86,.T.);
#16235=ADVANCED_FACE('',(#2925),#2067,.T.);
#16236=ADVANCED_FACE('',(#2926),#15405,.T.);
#16237=ADVANCED_FACE('',(#2927),#87,.T.);
#16238=ADVANCED_FACE('',(#2928),#88,.T.);
#16239=ADVANCED_FACE('',(#2929),#2068,.T.);
#16240=ADVANCED_FACE('',(#2930),#15406,.T.);
#16241=ADVANCED_FACE('',(#2931),#89,.T.);
#16242=ADVANCED_FACE('',(#2932),#90,.T.);
#16243=ADVANCED_FACE('',(#2933),#2069,.T.);
#16244=ADVANCED_FACE('',(#2934),#15407,.T.);
#16245=ADVANCED_FACE('',(#2935),#91,.T.);
#16246=ADVANCED_FACE('',(#2936),#92,.T.);
#16247=ADVANCED_FACE('',(#2937),#2070,.T.);
#16248=ADVANCED_FACE('',(#2938),#15408,.T.);
#16249=ADVANCED_FACE('',(#2939),#93,.T.);
#16250=ADVANCED_FACE('',(#2940),#94,.T.);
#16251=ADVANCED_FACE('',(#2941),#2071,.T.);
#16252=ADVANCED_FACE('',(#2942),#15409,.T.);
#16253=ADVANCED_FACE('',(#2943),#95,.T.);
#16254=ADVANCED_FACE('',(#2944),#96,.T.);
#16255=ADVANCED_FACE('',(#2945),#2072,.T.);
#16256=ADVANCED_FACE('',(#2946),#15410,.T.);
#16257=ADVANCED_FACE('',(#2947),#97,.T.);
#16258=ADVANCED_FACE('',(#2948),#98,.T.);
#16259=ADVANCED_FACE('',(#2949),#2073,.T.);
#16260=ADVANCED_FACE('',(#2950),#15411,.T.);
#16261=ADVANCED_FACE('',(#2951),#99,.T.);
#16262=ADVANCED_FACE('',(#2952),#100,.T.);
#16263=ADVANCED_FACE('',(#2953),#2074,.T.);
#16264=ADVANCED_FACE('',(#2954),#15412,.T.);
#16265=ADVANCED_FACE('',(#2955),#101,.T.);
#16266=ADVANCED_FACE('',(#2956),#102,.T.);
#16267=ADVANCED_FACE('',(#2957),#2075,.T.);
#16268=ADVANCED_FACE('',(#2958),#15413,.T.);
#16269=ADVANCED_FACE('',(#2959),#103,.T.);
#16270=ADVANCED_FACE('',(#2960),#104,.T.);
#16271=ADVANCED_FACE('',(#2961),#2076,.T.);
#16272=ADVANCED_FACE('',(#2962),#15414,.T.);
#16273=ADVANCED_FACE('',(#2963),#105,.T.);
#16274=ADVANCED_FACE('',(#2964),#106,.T.);
#16275=ADVANCED_FACE('',(#2965),#2077,.T.);
#16276=ADVANCED_FACE('',(#2966),#15415,.T.);
#16277=ADVANCED_FACE('',(#2967),#107,.T.);
#16278=ADVANCED_FACE('',(#2968),#108,.T.);
#16279=ADVANCED_FACE('',(#2969),#2078,.T.);
#16280=ADVANCED_FACE('',(#2970),#15416,.T.);
#16281=ADVANCED_FACE('',(#2971),#109,.T.);
#16282=ADVANCED_FACE('',(#2972),#110,.T.);
#16283=ADVANCED_FACE('',(#2973),#2079,.T.);
#16284=ADVANCED_FACE('',(#2974),#15417,.T.);
#16285=ADVANCED_FACE('',(#2975),#111,.T.);
#16286=ADVANCED_FACE('',(#2976),#112,.T.);
#16287=ADVANCED_FACE('',(#2977),#2080,.T.);
#16288=ADVANCED_FACE('',(#2978),#15418,.T.);
#16289=ADVANCED_FACE('',(#2979),#113,.T.);
#16290=ADVANCED_FACE('',(#2980),#114,.T.);
#16291=ADVANCED_FACE('',(#2981),#2081,.T.);
#16292=ADVANCED_FACE('',(#2982),#15419,.T.);
#16293=ADVANCED_FACE('',(#2983),#115,.T.);
#16294=ADVANCED_FACE('',(#2984),#116,.T.);
#16295=ADVANCED_FACE('',(#2985),#2082,.T.);
#16296=ADVANCED_FACE('',(#2986),#15420,.T.);
#16297=ADVANCED_FACE('',(#2987),#117,.T.);
#16298=ADVANCED_FACE('',(#2988),#118,.T.);
#16299=ADVANCED_FACE('',(#2989),#2083,.T.);
#16300=ADVANCED_FACE('',(#2990),#15421,.T.);
#16301=ADVANCED_FACE('',(#2991),#119,.T.);
#16302=ADVANCED_FACE('',(#2992),#120,.T.);
#16303=ADVANCED_FACE('',(#2993),#2084,.T.);
#16304=ADVANCED_FACE('',(#2994),#15422,.T.);
#16305=ADVANCED_FACE('',(#2995),#121,.T.);
#16306=ADVANCED_FACE('',(#2996),#122,.T.);
#16307=ADVANCED_FACE('',(#2997),#2085,.T.);
#16308=ADVANCED_FACE('',(#2998),#15423,.T.);
#16309=ADVANCED_FACE('',(#2999),#123,.T.);
#16310=ADVANCED_FACE('',(#3000),#124,.T.);
#16311=ADVANCED_FACE('',(#3001),#2086,.T.);
#16312=ADVANCED_FACE('',(#3002),#15424,.T.);
#16313=ADVANCED_FACE('',(#3003),#125,.T.);
#16314=ADVANCED_FACE('',(#3004),#126,.T.);
#16315=ADVANCED_FACE('',(#3005),#2087,.T.);
#16316=ADVANCED_FACE('',(#3006),#15425,.T.);
#16317=ADVANCED_FACE('',(#3007),#127,.T.);
#16318=ADVANCED_FACE('',(#3008),#2088,.T.);
#16319=ADVANCED_FACE('',(#3009),#128,.T.);
#16320=ADVANCED_FACE('',(#3010),#15426,.T.);
#16321=ADVANCED_FACE('',(#3011),#129,.T.);
#16322=ADVANCED_FACE('',(#3012),#130,.T.);
#16323=ADVANCED_FACE('',(#3013),#2089,.T.);
#16324=ADVANCED_FACE('',(#3014,#1628),#2090,.T.);
#16325=ADVANCED_FACE('',(#3015),#15427,.T.);
#16326=ADVANCED_FACE('',(#3016),#2091,.F.);
#16327=ADVANCED_FACE('',(#3017),#2092,.T.);
#16328=ADVANCED_FACE('',(#3018),#2093,.T.);
#16329=ADVANCED_FACE('',(#3019),#2094,.T.);
#16330=ADVANCED_FACE('',(#3020),#2095,.T.);
#16331=ADVANCED_FACE('',(#3021),#2096,.T.);
#16332=ADVANCED_FACE('',(#3022),#2097,.F.);
#16333=ADVANCED_FACE('',(#3023),#2098,.T.);
#16334=ADVANCED_FACE('',(#3024),#2099,.T.);
#16335=ADVANCED_FACE('',(#3025),#2100,.T.);
#16336=ADVANCED_FACE('',(#3026),#2101,.F.);
#16337=ADVANCED_FACE('',(#3027),#2102,.F.);
#16338=ADVANCED_FACE('',(#3028),#2103,.F.);
#16339=ADVANCED_FACE('',(#3029),#2104,.F.);
#16340=ADVANCED_FACE('',(#3030),#2105,.F.);
#16341=ADVANCED_FACE('',(#3031),#2106,.F.);
#16342=ADVANCED_FACE('',(#3032),#2107,.F.);
#16343=ADVANCED_FACE('',(#3033,#1629),#2108,.T.);
#16344=ADVANCED_FACE('',(#3034),#1045,.T.);
#16345=ADVANCED_FACE('',(#3035),#15428,.T.);
#16346=ADVANCED_FACE('',(#3036),#1046,.T.);
#16347=ADVANCED_FACE('',(#3037),#2109,.T.);
#16348=ADVANCED_FACE('',(#3038),#2110,.T.);
#16349=ADVANCED_FACE('',(#3039),#1047,.T.);
#16350=ADVANCED_FACE('',(#3040),#15429,.T.);
#16351=ADVANCED_FACE('',(#3041),#1048,.T.);
#16352=ADVANCED_FACE('',(#3042,#1630),#2111,.T.);
#16353=ADVANCED_FACE('',(#3043),#1049,.T.);
#16354=ADVANCED_FACE('',(#3044),#15430,.T.);
#16355=ADVANCED_FACE('',(#3045),#1050,.T.);
#16356=ADVANCED_FACE('',(#3046),#2112,.T.);
#16357=ADVANCED_FACE('',(#3047),#2113,.F.);
#16358=ADVANCED_FACE('',(#3048),#2114,.F.);
#16359=ADVANCED_FACE('',(#3049),#2115,.F.);
#16360=ADVANCED_FACE('',(#3050),#2116,.F.);
#16361=ADVANCED_FACE('',(#3051),#2117,.F.);
#16362=ADVANCED_FACE('',(#3052),#2118,.F.);
#16363=ADVANCED_FACE('',(#3053),#2119,.F.);
#16364=ADVANCED_FACE('',(#3054),#2120,.F.);
#16365=ADVANCED_FACE('',(#3055),#15431,.F.);
#16366=ADVANCED_FACE('',(#3056),#15432,.T.);
#16367=ADVANCED_FACE('',(#3057,#1631),#2121,.T.);
#16368=ADVANCED_FACE('',(#3058,#1632),#2122,.F.);
#16369=CLOSED_SHELL('',(#15433,#15434,#15435,#15436,#15437,#15438,#15439,
#15440,#15441));
#16370=CLOSED_SHELL('',(#15442,#15443,#15444,#15445,#15446,#15447,#15448,
#15449,#15450,#15451,#15452,#15453,#15454,#15455,#15456,#15457,#15458,#15459,
#15460,#15461,#15462,#15463,#15464,#15465,#15466,#15467,#15468,#15469,#15470,
#15471,#15472,#15473,#15474));
#16371=CLOSED_SHELL('',(#15475,#15476,#15477,#15478,#15479,#15480,#15481,
#15482,#15483,#15484));
#16372=CLOSED_SHELL('',(#15485,#15486,#15487,#15488,#15489,#15490,#15491,
#15492,#15493,#15494));
#16373=CLOSED_SHELL('',(#15495,#15496,#15497,#15498,#15499,#15500,#15501,
#15502,#15503,#15504));
#16374=CLOSED_SHELL('',(#15505,#15506,#15507,#15508,#15509,#15510,#15511,
#15512,#15513,#15514));
#16375=CLOSED_SHELL('',(#15515,#15516,#15517,#15518,#15519,#15520,#15521,
#15522));
#16376=CLOSED_SHELL('',(#15523,#15524,#15525,#15526,#15527,#15528,#15529,
#15530));
#16377=CLOSED_SHELL('',(#15531,#15532,#15533,#15534,#15535,#15536,#15537,
#15538,#15539,#15540));
#16378=CLOSED_SHELL('',(#15541,#15542,#15543,#15544,#15545,#15546,#15547,
#15548,#15549,#15550));
#16379=CLOSED_SHELL('',(#15551,#15552,#15553,#15554,#15555,#15556,#15557,
#15558,#15559,#15560));
#16380=CLOSED_SHELL('',(#15561,#15562,#15563,#15564,#15565,#15566,#15567,
#15568,#15569,#15570));
#16381=CLOSED_SHELL('',(#15571,#15572,#15573,#15574,#15575,#15576,#15577,
#15578));
#16382=CLOSED_SHELL('',(#15579,#15580,#15581,#15582,#15583,#15584,#15585,
#15586));
#16383=CLOSED_SHELL('',(#15587));
#16384=CLOSED_SHELL('',(#15588));
#16385=CLOSED_SHELL('',(#15589));
#16386=CLOSED_SHELL('',(#15590));
#16387=CLOSED_SHELL('',(#15591));
#16388=CLOSED_SHELL('',(#15592));
#16389=CLOSED_SHELL('',(#15593));
#16390=CLOSED_SHELL('',(#15594,#15595,#15596,#15597,#15598,#15599,#15600,
#15601,#15602,#15603,#15604,#15605,#15606,#15607,#15608,#15609,#15610));
#16391=CLOSED_SHELL('',(#15611,#15612,#15613,#15614));
#16392=CLOSED_SHELL('',(#15615,#15616,#15617,#15618));
#16393=CLOSED_SHELL('',(#15619,#15620,#15621,#15622,#15623,#15624,#15625,
#15626));
#16394=CLOSED_SHELL('',(#15627,#15628,#15629,#15630,#15631,#15632,#15633,
#15634));
#16395=CLOSED_SHELL('',(#15635));
#16396=CLOSED_SHELL('',(#15636));
#16397=CLOSED_SHELL('',(#15637));
#16398=CLOSED_SHELL('',(#15638));
#16399=CLOSED_SHELL('',(#15639));
#16400=CLOSED_SHELL('',(#15640));
#16401=CLOSED_SHELL('',(#15641));
#16402=CLOSED_SHELL('',(#15642));
#16403=CLOSED_SHELL('',(#15643,#15644,#15645,#15646,#15647,#15648,#15649,
#15650,#15651,#15652,#15653,#15654,#15655,#15656,#15657,#15658,#15659,#15660,
#15661));
#16404=CLOSED_SHELL('',(#15662,#15663,#15664,#15665));
#16405=CLOSED_SHELL('',(#15666,#15667,#15668,#15669));
#16406=CLOSED_SHELL('',(#15670,#15671,#15672,#15673,#15674,#15675,#15676,
#15677));
#16407=CLOSED_SHELL('',(#15678,#15679,#15680,#15681,#15682,#15683,#15684,
#15685));
#16408=CLOSED_SHELL('',(#15686,#15687,#15688,#15689,#15690,#15691,#15692,
#15693,#15694,#15695,#15696,#15697,#15698,#15699,#15700,#15701,#15702,#15703,
#15704,#15705,#15706,#15707,#15708,#15709,#15710,#15711,#15712,#15713,#15714,
#15715,#15716,#15717,#15718,#15719,#15720,#15721,#15722,#15723,#15724,#15725,
#15726,#15727,#15728,#15729,#15730,#15731,#15732,#15733,#15734,#15735,#15736,
#15737,#15738,#15739,#15740,#15741,#15742,#15743,#15744,#15745,#15746,#15747,
#15748,#15749,#15750,#15751,#15752,#15753,#15754,#15755,#15756,#15757,#15758,
#15759,#15760,#15761,#15762,#15763,#15764,#15765,#15766,#15767,#15768,#15769,
#15770,#15771,#15772,#15773,#15774,#15775,#15776,#15777,#15778,#15779,#15780,
#15781,#15782,#15783,#15784,#15785,#15786,#15787,#15788,#15789,#15790,#15791,
#15792,#15793,#15794,#15795,#15796,#15797,#15798,#15799,#15800,#15801,#15802,
#15803,#15804,#15805,#15806,#15807,#15808,#15809,#15810,#15811,#15812,#15813,
#15814,#15815,#15816,#15817,#15818));
#16409=CLOSED_SHELL('',(#15819,#15820,#15821,#15822));
#16410=CLOSED_SHELL('',(#15823,#15824,#15825,#15826));
#16411=CLOSED_SHELL('',(#15827,#15828,#15829,#15830,#15831,#15832));
#16412=CLOSED_SHELL('',(#15833,#15834,#15835,#15836,#15837,#15838));
#16413=CLOSED_SHELL('',(#15839,#15840,#15841,#15842,#15843,#15844,#15845,
#15846));
#16414=CLOSED_SHELL('',(#15847,#15848,#15849,#15850,#15851,#15852,#15853,
#15854,#15855,#15856));
#16415=CLOSED_SHELL('',(#15857,#15858,#15859,#15860,#15861,#15862,#15863,
#15864,#15865,#15866,#15867,#15868,#15869,#15870,#15871,#15872,#15873,#15874,
#15875));
#16416=CLOSED_SHELL('',(#15876,#15877,#15878,#15879));
#16417=CLOSED_SHELL('',(#15880,#15881,#15882,#15883));
#16418=CLOSED_SHELL('',(#15884,#15885,#15886,#15887,#15888,#15889,#15890));
#16419=CLOSED_SHELL('',(#15891,#15892,#15893,#15894,#15895,#15896,#15897,
#15898,#15899,#15900,#15901,#15902,#15903));
#16420=CLOSED_SHELL('',(#15904,#15905,#15906,#15907));
#16421=CLOSED_SHELL('',(#15908,#15909,#15910,#15911));
#16422=CLOSED_SHELL('',(#15912,#15913,#15914,#15915));
#16423=CLOSED_SHELL('',(#15916,#15917,#15918,#15919));
#16424=CLOSED_SHELL('',(#15920,#15921,#15922,#15923));
#16425=CLOSED_SHELL('',(#15924,#15925,#15926,#15927,#15928,#15929,#15930,
#15931));
#16426=CLOSED_SHELL('',(#15932,#15933,#15934,#15935,#15936,#15937,#15938,
#15939,#15940,#15941));
#16427=CLOSED_SHELL('',(#15942,#15943,#15944,#15945,#15946,#15947,#15948,
#15949,#15950,#15951,#15952,#15953,#15954,#15955));
#16428=CLOSED_SHELL('',(#15956,#15957,#15958,#15959));
#16429=CLOSED_SHELL('',(#15960,#15961,#15962,#15963));
#16430=CLOSED_SHELL('',(#15964,#15965,#15966,#15967,#15968,#15969,#15970));
#16431=CLOSED_SHELL('',(#15971,#15972,#15973,#15974));
#16432=CLOSED_SHELL('',(#15975,#15976,#15977,#15978,#15979,#15980,#15981,
#15982,#15983,#15984,#15985,#15986,#15987,#15988));
#16433=CLOSED_SHELL('',(#15989,#15990,#15991,#15992));
#16434=CLOSED_SHELL('',(#15993,#15994,#15995,#15996));
#16435=CLOSED_SHELL('',(#15997,#15998,#15999,#16000,#16001,#16002,#16003));
#16436=CLOSED_SHELL('',(#16004,#16005,#16006,#16007));
#16437=CLOSED_SHELL('',(#16008,#16009,#16010,#16011,#16012,#16013,#16014,
#16015,#16016,#16017,#16018,#16019,#16020,#16021,#16022,#16023,#16024,#16025,
#16026,#16027,#16028,#16029,#16030,#16031,#16032,#16033,#16034,#16035,#16036,
#16037,#16038,#16039,#16040,#16041,#16042,#16043,#16044,#16045,#16046,#16047,
#16048,#16049,#16050,#16051,#16052,#16053,#16054,#16055,#16056,#16057,#16058,
#16059,#16060,#16061,#16062,#16063,#16064,#16065,#16066,#16067,#16068,#16069,
#16070,#16071,#16072,#16073,#16074,#16075,#16076,#16077,#16078,#16079,#16080,
#16081,#16082,#16083,#16084,#16085,#16086,#16087,#16088,#16089,#16090,#16091,
#16092,#16093,#16094,#16095));
#16438=CLOSED_SHELL('',(#16096,#16097,#16098,#16099,#16100,#16101,#16102,
#16103,#16104,#16105));
#16439=CLOSED_SHELL('',(#16106,#16107,#16108,#16109,#16110,#16111,#16112,
#16113,#16114,#16115,#16116,#16117,#16118,#16119));
#16440=CLOSED_SHELL('',(#16120,#16121,#16122,#16123));
#16441=CLOSED_SHELL('',(#16124,#16125,#16126,#16127));
#16442=CLOSED_SHELL('',(#16128,#16129,#16130,#16131,#16132,#16133,#16134));
#16443=CLOSED_SHELL('',(#16135,#16136,#16137,#16138));
#16444=CLOSED_SHELL('',(#16139,#16140,#16141,#16142));
#16445=CLOSED_SHELL('',(#16143,#16144,#16145,#16146,#16147,#16148,#16149,
#16150,#16151,#16152,#16153));
#16446=CLOSED_SHELL('',(#16154,#16155,#16156,#16157));
#16447=CLOSED_SHELL('',(#16158,#16159,#16160,#16161,#16162,#16163,#16164,
#16165,#16166,#16167,#16168,#16169,#16170,#16171,#16172,#16173,#16174,#16175,
#16176,#16177,#16178,#16179,#16180,#16181,#16182,#16183,#16184,#16185,#16186,
#16187,#16188,#16189,#16190,#16191,#16192,#16193,#16194,#16195,#16196,#16197,
#16198,#16199,#16200,#16201,#16202,#16203,#16204,#16205,#16206,#16207,#16208,
#16209,#16210,#16211,#16212,#16213,#16214,#16215,#16216,#16217,#16218,#16219,
#16220,#16221,#16222,#16223,#16224,#16225,#16226,#16227,#16228,#16229,#16230,
#16231,#16232,#16233,#16234,#16235,#16236,#16237,#16238,#16239,#16240,#16241,
#16242,#16243,#16244,#16245,#16246,#16247,#16248,#16249,#16250,#16251,#16252,
#16253,#16254,#16255,#16256,#16257,#16258,#16259,#16260,#16261,#16262,#16263,
#16264,#16265,#16266,#16267,#16268,#16269,#16270,#16271,#16272,#16273,#16274,
#16275,#16276,#16277,#16278,#16279,#16280,#16281,#16282,#16283,#16284,#16285,
#16286,#16287,#16288,#16289,#16290,#16291,#16292,#16293,#16294,#16295,#16296,
#16297,#16298,#16299,#16300,#16301,#16302,#16303,#16304,#16305,#16306,#16307,
#16308,#16309,#16310,#16311,#16312,#16313,#16314,#16315,#16316,#16317,#16318,
#16319,#16320,#16321,#16322,#16323,#16324,#16325));
#16448=CLOSED_SHELL('',(#16326,#16327,#16328,#16329,#16330,#16331,#16332,
#16333,#16334,#16335));
#16449=CLOSED_SHELL('',(#16336,#16337,#16338,#16339,#16340,#16341,#16342,
#16343,#16344,#16345,#16346,#16347));
#16450=CLOSED_SHELL('',(#16348,#16349,#16350,#16351,#16352,#16353,#16354,
#16355,#16356));
#16451=CLOSED_SHELL('',(#16357,#16358,#16359,#16360,#16361,#16362,#16363,
#16364));
#16452=CLOSED_SHELL('',(#16365,#16366,#16367,#16368));
#16453=DERIVED_UNIT_ELEMENT(#16581,1.);
#16454=DERIVED_UNIT_ELEMENT(#62760,-3.);
#16455=DERIVED_UNIT_ELEMENT(#16581,1.);
#16456=DERIVED_UNIT_ELEMENT(#62760,-3.);
#16457=DERIVED_UNIT_ELEMENT(#16581,1.);
#16458=DERIVED_UNIT_ELEMENT(#62760,-3.);
#16459=DERIVED_UNIT_ELEMENT(#16581,1.);
#16460=DERIVED_UNIT_ELEMENT(#62760,-3.);
#16461=DERIVED_UNIT_ELEMENT(#16581,1.);
#16462=DERIVED_UNIT_ELEMENT(#62760,-3.);
#16463=DERIVED_UNIT_ELEMENT(#16581,1.);
#16464=DERIVED_UNIT_ELEMENT(#62760,-3.);
#16465=DERIVED_UNIT_ELEMENT(#16581,1.);
#16466=DERIVED_UNIT_ELEMENT(#62760,-3.);
#16467=DERIVED_UNIT_ELEMENT(#16581,1.);
#16468=DERIVED_UNIT_ELEMENT(#62760,-3.);
#16469=DERIVED_UNIT_ELEMENT(#16581,1.);
#16470=DERIVED_UNIT_ELEMENT(#62760,-3.);
#16471=DERIVED_UNIT_ELEMENT(#16581,1.);
#16472=DERIVED_UNIT_ELEMENT(#62760,-3.);
#16473=DERIVED_UNIT_ELEMENT(#16581,1.);
#16474=DERIVED_UNIT_ELEMENT(#62760,-3.);
#16475=DERIVED_UNIT_ELEMENT(#16581,1.);
#16476=DERIVED_UNIT_ELEMENT(#62760,-3.);
#16477=DERIVED_UNIT_ELEMENT(#16581,1.);
#16478=DERIVED_UNIT_ELEMENT(#62760,-3.);
#16479=DERIVED_UNIT_ELEMENT(#16581,1.);
#16480=DERIVED_UNIT_ELEMENT(#62760,-3.);
#16481=DERIVED_UNIT_ELEMENT(#16581,1.);
#16482=DERIVED_UNIT_ELEMENT(#62760,-3.);
#16483=DERIVED_UNIT_ELEMENT(#16581,1.);
#16484=DERIVED_UNIT_ELEMENT(#62760,-3.);
#16485=DERIVED_UNIT_ELEMENT(#16581,1.);
#16486=DERIVED_UNIT_ELEMENT(#62760,-3.);
#16487=DERIVED_UNIT_ELEMENT(#16581,1.);
#16488=DERIVED_UNIT_ELEMENT(#62760,-3.);
#16489=DERIVED_UNIT_ELEMENT(#16581,1.);
#16490=DERIVED_UNIT_ELEMENT(#62760,-3.);
#16491=DERIVED_UNIT_ELEMENT(#16581,1.);
#16492=DERIVED_UNIT_ELEMENT(#62760,-3.);
#16493=DERIVED_UNIT_ELEMENT(#16581,1.);
#16494=DERIVED_UNIT_ELEMENT(#62760,-3.);
#16495=DERIVED_UNIT_ELEMENT(#16581,1.);
#16496=DERIVED_UNIT_ELEMENT(#62760,-3.);
#16497=DERIVED_UNIT_ELEMENT(#16581,1.);
#16498=DERIVED_UNIT_ELEMENT(#62760,-3.);
#16499=DERIVED_UNIT_ELEMENT(#16581,1.);
#16500=DERIVED_UNIT_ELEMENT(#62760,-3.);
#16501=DERIVED_UNIT_ELEMENT(#16581,1.);
#16502=DERIVED_UNIT_ELEMENT(#62760,-3.);
#16503=DERIVED_UNIT_ELEMENT(#16581,1.);
#16504=DERIVED_UNIT_ELEMENT(#62760,-3.);
#16505=DERIVED_UNIT_ELEMENT(#16581,1.);
#16506=DERIVED_UNIT_ELEMENT(#62760,-3.);
#16507=DERIVED_UNIT_ELEMENT(#16581,1.);
#16508=DERIVED_UNIT_ELEMENT(#62760,-3.);
#16509=DERIVED_UNIT_ELEMENT(#16581,1.);
#16510=DERIVED_UNIT_ELEMENT(#62760,-3.);
#16511=DERIVED_UNIT_ELEMENT(#16581,1.);
#16512=DERIVED_UNIT_ELEMENT(#62760,-3.);
#16513=DERIVED_UNIT_ELEMENT(#16581,1.);
#16514=DERIVED_UNIT_ELEMENT(#62760,-3.);
#16515=DERIVED_UNIT_ELEMENT(#16581,1.);
#16516=DERIVED_UNIT_ELEMENT(#62760,-3.);
#16517=DERIVED_UNIT_ELEMENT(#16581,1.);
#16518=DERIVED_UNIT_ELEMENT(#62760,-3.);
#16519=DERIVED_UNIT_ELEMENT(#16581,1.);
#16520=DERIVED_UNIT_ELEMENT(#62760,-3.);
#16521=DERIVED_UNIT_ELEMENT(#16581,1.);
#16522=DERIVED_UNIT_ELEMENT(#62760,-3.);
#16523=DERIVED_UNIT_ELEMENT(#16581,1.);
#16524=DERIVED_UNIT_ELEMENT(#62760,-3.);
#16525=DERIVED_UNIT_ELEMENT(#16581,1.);
#16526=DERIVED_UNIT_ELEMENT(#62760,-3.);
#16527=DERIVED_UNIT_ELEMENT(#16581,1.);
#16528=DERIVED_UNIT_ELEMENT(#62760,-3.);
#16529=DERIVED_UNIT_ELEMENT(#16581,1.);
#16530=DERIVED_UNIT_ELEMENT(#62760,-3.);
#16531=DERIVED_UNIT_ELEMENT(#16581,1.);
#16532=DERIVED_UNIT_ELEMENT(#62760,-3.);
#16533=DERIVED_UNIT_ELEMENT(#16581,1.);
#16534=DERIVED_UNIT_ELEMENT(#62760,-3.);
#16535=DERIVED_UNIT_ELEMENT(#16581,1.);
#16536=DERIVED_UNIT_ELEMENT(#62760,-3.);
#16537=DERIVED_UNIT_ELEMENT(#16581,1.);
#16538=DERIVED_UNIT_ELEMENT(#62760,-3.);
#16539=DERIVED_UNIT_ELEMENT(#16581,1.);
#16540=DERIVED_UNIT_ELEMENT(#62760,-3.);
#16541=DERIVED_UNIT_ELEMENT(#16581,1.);
#16542=DERIVED_UNIT_ELEMENT(#62760,-3.);
#16543=DERIVED_UNIT_ELEMENT(#16581,1.);
#16544=DERIVED_UNIT_ELEMENT(#62760,-3.);
#16545=DERIVED_UNIT_ELEMENT(#16581,1.);
#16546=DERIVED_UNIT_ELEMENT(#62760,-3.);
#16547=DERIVED_UNIT_ELEMENT(#16581,1.);
#16548=DERIVED_UNIT_ELEMENT(#62760,-3.);
#16549=DERIVED_UNIT_ELEMENT(#16581,1.);
#16550=DERIVED_UNIT_ELEMENT(#62760,-3.);
#16551=DERIVED_UNIT_ELEMENT(#16581,1.);
#16552=DERIVED_UNIT_ELEMENT(#62760,-3.);
#16553=DERIVED_UNIT_ELEMENT(#16581,1.);
#16554=DERIVED_UNIT_ELEMENT(#62760,-3.);
#16555=DERIVED_UNIT_ELEMENT(#16581,1.);
#16556=DERIVED_UNIT_ELEMENT(#62760,-3.);
#16557=DERIVED_UNIT_ELEMENT(#16581,1.);
#16558=DERIVED_UNIT_ELEMENT(#62760,-3.);
#16559=DERIVED_UNIT_ELEMENT(#16581,1.);
#16560=DERIVED_UNIT_ELEMENT(#62760,-3.);
#16561=DERIVED_UNIT_ELEMENT(#16581,1.);
#16562=DERIVED_UNIT_ELEMENT(#62760,-3.);
#16563=DERIVED_UNIT_ELEMENT(#16581,1.);
#16564=DERIVED_UNIT_ELEMENT(#62760,-3.);
#16565=DERIVED_UNIT_ELEMENT(#16581,1.);
#16566=DERIVED_UNIT_ELEMENT(#62760,-3.);
#16567=DERIVED_UNIT_ELEMENT(#16581,1.);
#16568=DERIVED_UNIT_ELEMENT(#62760,-3.);
#16569=DERIVED_UNIT_ELEMENT(#16581,1.);
#16570=DERIVED_UNIT_ELEMENT(#62760,-3.);
#16571=DERIVED_UNIT_ELEMENT(#16581,1.);
#16572=DERIVED_UNIT_ELEMENT(#62760,-3.);
#16573=DERIVED_UNIT_ELEMENT(#16581,1.);
#16574=DERIVED_UNIT_ELEMENT(#62760,-3.);
#16575=DERIVED_UNIT_ELEMENT(#16581,1.);
#16576=DERIVED_UNIT_ELEMENT(#62760,-3.);
#16577=DERIVED_UNIT_ELEMENT(#16581,1.);
#16578=DERIVED_UNIT_ELEMENT(#62760,-3.);
#16579=DERIVED_UNIT_ELEMENT(#16581,1.);
#16580=DERIVED_UNIT_ELEMENT(#62760,-3.);
#16581=(
MASS_UNIT()
NAMED_UNIT(*)
SI_UNIT(.KILO.,.GRAM.)
);
#16582=DERIVED_UNIT((#16453,#16454));
#16583=DERIVED_UNIT((#16455,#16456));
#16584=DERIVED_UNIT((#16457,#16458));
#16585=DERIVED_UNIT((#16459,#16460));
#16586=DERIVED_UNIT((#16461,#16462));
#16587=DERIVED_UNIT((#16463,#16464));
#16588=DERIVED_UNIT((#16465,#16466));
#16589=DERIVED_UNIT((#16467,#16468));
#16590=DERIVED_UNIT((#16469,#16470));
#16591=DERIVED_UNIT((#16471,#16472));
#16592=DERIVED_UNIT((#16473,#16474));
#16593=DERIVED_UNIT((#16475,#16476));
#16594=DERIVED_UNIT((#16477,#16478));
#16595=DERIVED_UNIT((#16479,#16480));
#16596=DERIVED_UNIT((#16481,#16482));
#16597=DERIVED_UNIT((#16483,#16484));
#16598=DERIVED_UNIT((#16485,#16486));
#16599=DERIVED_UNIT((#16487,#16488));
#16600=DERIVED_UNIT((#16489,#16490));
#16601=DERIVED_UNIT((#16491,#16492));
#16602=DERIVED_UNIT((#16493,#16494));
#16603=DERIVED_UNIT((#16495,#16496));
#16604=DERIVED_UNIT((#16497,#16498));
#16605=DERIVED_UNIT((#16499,#16500));
#16606=DERIVED_UNIT((#16501,#16502));
#16607=DERIVED_UNIT((#16503,#16504));
#16608=DERIVED_UNIT((#16505,#16506));
#16609=DERIVED_UNIT((#16507,#16508));
#16610=DERIVED_UNIT((#16509,#16510));
#16611=DERIVED_UNIT((#16511,#16512));
#16612=DERIVED_UNIT((#16513,#16514));
#16613=DERIVED_UNIT((#16515,#16516));
#16614=DERIVED_UNIT((#16517,#16518));
#16615=DERIVED_UNIT((#16519,#16520));
#16616=DERIVED_UNIT((#16521,#16522));
#16617=DERIVED_UNIT((#16523,#16524));
#16618=DERIVED_UNIT((#16525,#16526));
#16619=DERIVED_UNIT((#16527,#16528));
#16620=DERIVED_UNIT((#16529,#16530));
#16621=DERIVED_UNIT((#16531,#16532));
#16622=DERIVED_UNIT((#16533,#16534));
#16623=DERIVED_UNIT((#16535,#16536));
#16624=DERIVED_UNIT((#16537,#16538));
#16625=DERIVED_UNIT((#16539,#16540));
#16626=DERIVED_UNIT((#16541,#16542));
#16627=DERIVED_UNIT((#16543,#16544));
#16628=DERIVED_UNIT((#16545,#16546));
#16629=DERIVED_UNIT((#16547,#16548));
#16630=DERIVED_UNIT((#16549,#16550));
#16631=DERIVED_UNIT((#16551,#16552));
#16632=DERIVED_UNIT((#16553,#16554));
#16633=DERIVED_UNIT((#16555,#16556));
#16634=DERIVED_UNIT((#16557,#16558));
#16635=DERIVED_UNIT((#16559,#16560));
#16636=DERIVED_UNIT((#16561,#16562));
#16637=DERIVED_UNIT((#16563,#16564));
#16638=DERIVED_UNIT((#16565,#16566));
#16639=DERIVED_UNIT((#16567,#16568));
#16640=DERIVED_UNIT((#16569,#16570));
#16641=DERIVED_UNIT((#16571,#16572));
#16642=DERIVED_UNIT((#16573,#16574));
#16643=DERIVED_UNIT((#16575,#16576));
#16644=DERIVED_UNIT((#16577,#16578));
#16645=DERIVED_UNIT((#16579,#16580));
#16646=MEASURE_REPRESENTATION_ITEM('density measure',
POSITIVE_RATIO_MEASURE(7850.),#16582);
#16647=MEASURE_REPRESENTATION_ITEM('density measure',
POSITIVE_RATIO_MEASURE(7850.),#16583);
#16648=MEASURE_REPRESENTATION_ITEM('density measure',
POSITIVE_RATIO_MEASURE(7850.),#16584);
#16649=MEASURE_REPRESENTATION_ITEM('density measure',
POSITIVE_RATIO_MEASURE(7850.),#16585);
#16650=MEASURE_REPRESENTATION_ITEM('density measure',
POSITIVE_RATIO_MEASURE(7850.),#16586);
#16651=MEASURE_REPRESENTATION_ITEM('density measure',
POSITIVE_RATIO_MEASURE(7850.),#16587);
#16652=MEASURE_REPRESENTATION_ITEM('density measure',
POSITIVE_RATIO_MEASURE(7850.),#16588);
#16653=MEASURE_REPRESENTATION_ITEM('density measure',
POSITIVE_RATIO_MEASURE(7850.),#16589);
#16654=MEASURE_REPRESENTATION_ITEM('density measure',
POSITIVE_RATIO_MEASURE(7850.),#16590);
#16655=MEASURE_REPRESENTATION_ITEM('density measure',
POSITIVE_RATIO_MEASURE(7850.),#16591);
#16656=MEASURE_REPRESENTATION_ITEM('density measure',
POSITIVE_RATIO_MEASURE(7850.),#16592);
#16657=MEASURE_REPRESENTATION_ITEM('density measure',
POSITIVE_RATIO_MEASURE(7850.),#16593);
#16658=MEASURE_REPRESENTATION_ITEM('density measure',
POSITIVE_RATIO_MEASURE(7850.),#16594);
#16659=MEASURE_REPRESENTATION_ITEM('density measure',
POSITIVE_RATIO_MEASURE(7850.),#16595);
#16660=MEASURE_REPRESENTATION_ITEM('density measure',
POSITIVE_RATIO_MEASURE(7850.),#16596);
#16661=MEASURE_REPRESENTATION_ITEM('density measure',
POSITIVE_RATIO_MEASURE(7850.),#16597);
#16662=MEASURE_REPRESENTATION_ITEM('density measure',
POSITIVE_RATIO_MEASURE(7850.),#16598);
#16663=MEASURE_REPRESENTATION_ITEM('density measure',
POSITIVE_RATIO_MEASURE(7850.),#16599);
#16664=MEASURE_REPRESENTATION_ITEM('density measure',
POSITIVE_RATIO_MEASURE(7850.),#16600);
#16665=MEASURE_REPRESENTATION_ITEM('density measure',
POSITIVE_RATIO_MEASURE(7850.),#16601);
#16666=MEASURE_REPRESENTATION_ITEM('density measure',
POSITIVE_RATIO_MEASURE(7850.),#16602);
#16667=MEASURE_REPRESENTATION_ITEM('density measure',
POSITIVE_RATIO_MEASURE(7850.),#16603);
#16668=MEASURE_REPRESENTATION_ITEM('density measure',
POSITIVE_RATIO_MEASURE(7850.),#16604);
#16669=MEASURE_REPRESENTATION_ITEM('density measure',
POSITIVE_RATIO_MEASURE(7850.),#16605);
#16670=MEASURE_REPRESENTATION_ITEM('density measure',
POSITIVE_RATIO_MEASURE(7850.),#16606);
#16671=MEASURE_REPRESENTATION_ITEM('density measure',
POSITIVE_RATIO_MEASURE(7850.),#16607);
#16672=MEASURE_REPRESENTATION_ITEM('density measure',
POSITIVE_RATIO_MEASURE(7850.),#16608);
#16673=MEASURE_REPRESENTATION_ITEM('density measure',
POSITIVE_RATIO_MEASURE(7850.),#16609);
#16674=MEASURE_REPRESENTATION_ITEM('density measure',
POSITIVE_RATIO_MEASURE(7850.),#16610);
#16675=MEASURE_REPRESENTATION_ITEM('density measure',
POSITIVE_RATIO_MEASURE(7850.),#16611);
#16676=MEASURE_REPRESENTATION_ITEM('density measure',
POSITIVE_RATIO_MEASURE(7850.),#16612);
#16677=MEASURE_REPRESENTATION_ITEM('density measure',
POSITIVE_RATIO_MEASURE(7850.),#16613);
#16678=MEASURE_REPRESENTATION_ITEM('density measure',
POSITIVE_RATIO_MEASURE(7850.),#16614);
#16679=MEASURE_REPRESENTATION_ITEM('density measure',
POSITIVE_RATIO_MEASURE(7850.),#16615);
#16680=MEASURE_REPRESENTATION_ITEM('density measure',
POSITIVE_RATIO_MEASURE(7850.),#16616);
#16681=MEASURE_REPRESENTATION_ITEM('density measure',
POSITIVE_RATIO_MEASURE(7850.),#16617);
#16682=MEASURE_REPRESENTATION_ITEM('density measure',
POSITIVE_RATIO_MEASURE(7850.),#16618);
#16683=MEASURE_REPRESENTATION_ITEM('density measure',
POSITIVE_RATIO_MEASURE(7850.),#16619);
#16684=MEASURE_REPRESENTATION_ITEM('density measure',
POSITIVE_RATIO_MEASURE(7850.),#16620);
#16685=MEASURE_REPRESENTATION_ITEM('density measure',
POSITIVE_RATIO_MEASURE(7850.),#16621);
#16686=MEASURE_REPRESENTATION_ITEM('density measure',
POSITIVE_RATIO_MEASURE(7850.),#16622);
#16687=MEASURE_REPRESENTATION_ITEM('density measure',
POSITIVE_RATIO_MEASURE(7850.),#16623);
#16688=MEASURE_REPRESENTATION_ITEM('density measure',
POSITIVE_RATIO_MEASURE(7850.),#16624);
#16689=MEASURE_REPRESENTATION_ITEM('density measure',
POSITIVE_RATIO_MEASURE(7850.),#16625);
#16690=MEASURE_REPRESENTATION_ITEM('density measure',
POSITIVE_RATIO_MEASURE(7850.),#16626);
#16691=MEASURE_REPRESENTATION_ITEM('density measure',
POSITIVE_RATIO_MEASURE(7850.),#16627);
#16692=MEASURE_REPRESENTATION_ITEM('density measure',
POSITIVE_RATIO_MEASURE(7850.),#16628);
#16693=MEASURE_REPRESENTATION_ITEM('density measure',
POSITIVE_RATIO_MEASURE(7850.),#16629);
#16694=MEASURE_REPRESENTATION_ITEM('density measure',
POSITIVE_RATIO_MEASURE(7850.),#16630);
#16695=MEASURE_REPRESENTATION_ITEM('density measure',
POSITIVE_RATIO_MEASURE(7850.),#16631);
#16696=MEASURE_REPRESENTATION_ITEM('density measure',
POSITIVE_RATIO_MEASURE(7850.),#16632);
#16697=MEASURE_REPRESENTATION_ITEM('density measure',
POSITIVE_RATIO_MEASURE(7850.),#16633);
#16698=MEASURE_REPRESENTATION_ITEM('density measure',
POSITIVE_RATIO_MEASURE(7850.),#16634);
#16699=MEASURE_REPRESENTATION_ITEM('density measure',
POSITIVE_RATIO_MEASURE(7850.),#16635);
#16700=MEASURE_REPRESENTATION_ITEM('density measure',
POSITIVE_RATIO_MEASURE(7850.),#16636);
#16701=MEASURE_REPRESENTATION_ITEM('density measure',
POSITIVE_RATIO_MEASURE(7850.),#16637);
#16702=MEASURE_REPRESENTATION_ITEM('density measure',
POSITIVE_RATIO_MEASURE(7850.),#16638);
#16703=MEASURE_REPRESENTATION_ITEM('density measure',
POSITIVE_RATIO_MEASURE(7850.),#16639);
#16704=MEASURE_REPRESENTATION_ITEM('density measure',
POSITIVE_RATIO_MEASURE(7850.),#16640);
#16705=MEASURE_REPRESENTATION_ITEM('density measure',
POSITIVE_RATIO_MEASURE(7850.),#16641);
#16706=MEASURE_REPRESENTATION_ITEM('density measure',
POSITIVE_RATIO_MEASURE(7850.),#16642);
#16707=MEASURE_REPRESENTATION_ITEM('density measure',
POSITIVE_RATIO_MEASURE(7850.),#16643);
#16708=MEASURE_REPRESENTATION_ITEM('density measure',
POSITIVE_RATIO_MEASURE(7850.),#16644);
#16709=MEASURE_REPRESENTATION_ITEM('density measure',
POSITIVE_RATIO_MEASURE(7850.),#16645);
#16710=PROPERTY_DEFINITION_REPRESENTATION(#17030,#16838);
#16711=PROPERTY_DEFINITION_REPRESENTATION(#17031,#16839);
#16712=PROPERTY_DEFINITION_REPRESENTATION(#17032,#16840);
#16713=PROPERTY_DEFINITION_REPRESENTATION(#17033,#16841);
#16714=PROPERTY_DEFINITION_REPRESENTATION(#17034,#16842);
#16715=PROPERTY_DEFINITION_REPRESENTATION(#17035,#16843);
#16716=PROPERTY_DEFINITION_REPRESENTATION(#17036,#16844);
#16717=PROPERTY_DEFINITION_REPRESENTATION(#17037,#16845);
#16718=PROPERTY_DEFINITION_REPRESENTATION(#17038,#16846);
#16719=PROPERTY_DEFINITION_REPRESENTATION(#17039,#16847);
#16720=PROPERTY_DEFINITION_REPRESENTATION(#17040,#16848);
#16721=PROPERTY_DEFINITION_REPRESENTATION(#17041,#16849);
#16722=PROPERTY_DEFINITION_REPRESENTATION(#17042,#16850);
#16723=PROPERTY_DEFINITION_REPRESENTATION(#17043,#16851);
#16724=PROPERTY_DEFINITION_REPRESENTATION(#17044,#16852);
#16725=PROPERTY_DEFINITION_REPRESENTATION(#17045,#16853);
#16726=PROPERTY_DEFINITION_REPRESENTATION(#17046,#16854);
#16727=PROPERTY_DEFINITION_REPRESENTATION(#17047,#16855);
#16728=PROPERTY_DEFINITION_REPRESENTATION(#17048,#16856);
#16729=PROPERTY_DEFINITION_REPRESENTATION(#17049,#16857);
#16730=PROPERTY_DEFINITION_REPRESENTATION(#17050,#16858);
#16731=PROPERTY_DEFINITION_REPRESENTATION(#17051,#16859);
#16732=PROPERTY_DEFINITION_REPRESENTATION(#17052,#16860);
#16733=PROPERTY_DEFINITION_REPRESENTATION(#17053,#16861);
#16734=PROPERTY_DEFINITION_REPRESENTATION(#17054,#16862);
#16735=PROPERTY_DEFINITION_REPRESENTATION(#17055,#16863);
#16736=PROPERTY_DEFINITION_REPRESENTATION(#17056,#16864);
#16737=PROPERTY_DEFINITION_REPRESENTATION(#17057,#16865);
#16738=PROPERTY_DEFINITION_REPRESENTATION(#17058,#16866);
#16739=PROPERTY_DEFINITION_REPRESENTATION(#17059,#16867);
#16740=PROPERTY_DEFINITION_REPRESENTATION(#17060,#16868);
#16741=PROPERTY_DEFINITION_REPRESENTATION(#17061,#16869);
#16742=PROPERTY_DEFINITION_REPRESENTATION(#17062,#16870);
#16743=PROPERTY_DEFINITION_REPRESENTATION(#17063,#16871);
#16744=PROPERTY_DEFINITION_REPRESENTATION(#17064,#16872);
#16745=PROPERTY_DEFINITION_REPRESENTATION(#17065,#16873);
#16746=PROPERTY_DEFINITION_REPRESENTATION(#17066,#16874);
#16747=PROPERTY_DEFINITION_REPRESENTATION(#17067,#16875);
#16748=PROPERTY_DEFINITION_REPRESENTATION(#17068,#16876);
#16749=PROPERTY_DEFINITION_REPRESENTATION(#17069,#16877);
#16750=PROPERTY_DEFINITION_REPRESENTATION(#17070,#16878);
#16751=PROPERTY_DEFINITION_REPRESENTATION(#17071,#16879);
#16752=PROPERTY_DEFINITION_REPRESENTATION(#17072,#16880);
#16753=PROPERTY_DEFINITION_REPRESENTATION(#17073,#16881);
#16754=PROPERTY_DEFINITION_REPRESENTATION(#17074,#16882);
#16755=PROPERTY_DEFINITION_REPRESENTATION(#17075,#16883);
#16756=PROPERTY_DEFINITION_REPRESENTATION(#17076,#16884);
#16757=PROPERTY_DEFINITION_REPRESENTATION(#17077,#16885);
#16758=PROPERTY_DEFINITION_REPRESENTATION(#17078,#16886);
#16759=PROPERTY_DEFINITION_REPRESENTATION(#17079,#16887);
#16760=PROPERTY_DEFINITION_REPRESENTATION(#17080,#16888);
#16761=PROPERTY_DEFINITION_REPRESENTATION(#17081,#16889);
#16762=PROPERTY_DEFINITION_REPRESENTATION(#17082,#16890);
#16763=PROPERTY_DEFINITION_REPRESENTATION(#17083,#16891);
#16764=PROPERTY_DEFINITION_REPRESENTATION(#17084,#16892);
#16765=PROPERTY_DEFINITION_REPRESENTATION(#17085,#16893);
#16766=PROPERTY_DEFINITION_REPRESENTATION(#17086,#16894);
#16767=PROPERTY_DEFINITION_REPRESENTATION(#17087,#16895);
#16768=PROPERTY_DEFINITION_REPRESENTATION(#17088,#16896);
#16769=PROPERTY_DEFINITION_REPRESENTATION(#17089,#16897);
#16770=PROPERTY_DEFINITION_REPRESENTATION(#17090,#16898);
#16771=PROPERTY_DEFINITION_REPRESENTATION(#17091,#16899);
#16772=PROPERTY_DEFINITION_REPRESENTATION(#17092,#16900);
#16773=PROPERTY_DEFINITION_REPRESENTATION(#17093,#16901);
#16774=PROPERTY_DEFINITION_REPRESENTATION(#17094,#16902);
#16775=PROPERTY_DEFINITION_REPRESENTATION(#17095,#16903);
#16776=PROPERTY_DEFINITION_REPRESENTATION(#17096,#16904);
#16777=PROPERTY_DEFINITION_REPRESENTATION(#17097,#16905);
#16778=PROPERTY_DEFINITION_REPRESENTATION(#17098,#16906);
#16779=PROPERTY_DEFINITION_REPRESENTATION(#17099,#16907);
#16780=PROPERTY_DEFINITION_REPRESENTATION(#17100,#16908);
#16781=PROPERTY_DEFINITION_REPRESENTATION(#17101,#16909);
#16782=PROPERTY_DEFINITION_REPRESENTATION(#17102,#16910);
#16783=PROPERTY_DEFINITION_REPRESENTATION(#17103,#16911);
#16784=PROPERTY_DEFINITION_REPRESENTATION(#17104,#16912);
#16785=PROPERTY_DEFINITION_REPRESENTATION(#17105,#16913);
#16786=PROPERTY_DEFINITION_REPRESENTATION(#17106,#16914);
#16787=PROPERTY_DEFINITION_REPRESENTATION(#17107,#16915);
#16788=PROPERTY_DEFINITION_REPRESENTATION(#17108,#16916);
#16789=PROPERTY_DEFINITION_REPRESENTATION(#17109,#16917);
#16790=PROPERTY_DEFINITION_REPRESENTATION(#17110,#16918);
#16791=PROPERTY_DEFINITION_REPRESENTATION(#17111,#16919);
#16792=PROPERTY_DEFINITION_REPRESENTATION(#17112,#16920);
#16793=PROPERTY_DEFINITION_REPRESENTATION(#17113,#16921);
#16794=PROPERTY_DEFINITION_REPRESENTATION(#17114,#16922);
#16795=PROPERTY_DEFINITION_REPRESENTATION(#17115,#16923);
#16796=PROPERTY_DEFINITION_REPRESENTATION(#17116,#16924);
#16797=PROPERTY_DEFINITION_REPRESENTATION(#17117,#16925);
#16798=PROPERTY_DEFINITION_REPRESENTATION(#17118,#16926);
#16799=PROPERTY_DEFINITION_REPRESENTATION(#17119,#16927);
#16800=PROPERTY_DEFINITION_REPRESENTATION(#17120,#16928);
#16801=PROPERTY_DEFINITION_REPRESENTATION(#17121,#16929);
#16802=PROPERTY_DEFINITION_REPRESENTATION(#17122,#16930);
#16803=PROPERTY_DEFINITION_REPRESENTATION(#17123,#16931);
#16804=PROPERTY_DEFINITION_REPRESENTATION(#17124,#16932);
#16805=PROPERTY_DEFINITION_REPRESENTATION(#17125,#16933);
#16806=PROPERTY_DEFINITION_REPRESENTATION(#17126,#16934);
#16807=PROPERTY_DEFINITION_REPRESENTATION(#17127,#16935);
#16808=PROPERTY_DEFINITION_REPRESENTATION(#17128,#16936);
#16809=PROPERTY_DEFINITION_REPRESENTATION(#17129,#16937);
#16810=PROPERTY_DEFINITION_REPRESENTATION(#17130,#16938);
#16811=PROPERTY_DEFINITION_REPRESENTATION(#17131,#16939);
#16812=PROPERTY_DEFINITION_REPRESENTATION(#17132,#16940);
#16813=PROPERTY_DEFINITION_REPRESENTATION(#17133,#16941);
#16814=PROPERTY_DEFINITION_REPRESENTATION(#17134,#16942);
#16815=PROPERTY_DEFINITION_REPRESENTATION(#17135,#16943);
#16816=PROPERTY_DEFINITION_REPRESENTATION(#17136,#16944);
#16817=PROPERTY_DEFINITION_REPRESENTATION(#17137,#16945);
#16818=PROPERTY_DEFINITION_REPRESENTATION(#17138,#16946);
#16819=PROPERTY_DEFINITION_REPRESENTATION(#17139,#16947);
#16820=PROPERTY_DEFINITION_REPRESENTATION(#17140,#16948);
#16821=PROPERTY_DEFINITION_REPRESENTATION(#17141,#16949);
#16822=PROPERTY_DEFINITION_REPRESENTATION(#17142,#16950);
#16823=PROPERTY_DEFINITION_REPRESENTATION(#17143,#16951);
#16824=PROPERTY_DEFINITION_REPRESENTATION(#17144,#16952);
#16825=PROPERTY_DEFINITION_REPRESENTATION(#17145,#16953);
#16826=PROPERTY_DEFINITION_REPRESENTATION(#17146,#16954);
#16827=PROPERTY_DEFINITION_REPRESENTATION(#17147,#16955);
#16828=PROPERTY_DEFINITION_REPRESENTATION(#17148,#16956);
#16829=PROPERTY_DEFINITION_REPRESENTATION(#17149,#16957);
#16830=PROPERTY_DEFINITION_REPRESENTATION(#17150,#16958);
#16831=PROPERTY_DEFINITION_REPRESENTATION(#17151,#16959);
#16832=PROPERTY_DEFINITION_REPRESENTATION(#17152,#16960);
#16833=PROPERTY_DEFINITION_REPRESENTATION(#17153,#16961);
#16834=PROPERTY_DEFINITION_REPRESENTATION(#17154,#16962);
#16835=PROPERTY_DEFINITION_REPRESENTATION(#17155,#16963);
#16836=PROPERTY_DEFINITION_REPRESENTATION(#17156,#16964);
#16837=PROPERTY_DEFINITION_REPRESENTATION(#17157,#16965);
#16838=REPRESENTATION('material name',(#16966),#62687);
#16839=REPRESENTATION('density',(#16646),#62687);
#16840=REPRESENTATION('material name',(#16967),#62688);
#16841=REPRESENTATION('density',(#16647),#62688);
#16842=REPRESENTATION('material name',(#16968),#62689);
#16843=REPRESENTATION('density',(#16648),#62689);
#16844=REPRESENTATION('material name',(#16969),#62690);
#16845=REPRESENTATION('density',(#16649),#62690);
#16846=REPRESENTATION('material name',(#16970),#62691);
#16847=REPRESENTATION('density',(#16650),#62691);
#16848=REPRESENTATION('material name',(#16971),#62692);
#16849=REPRESENTATION('density',(#16651),#62692);
#16850=REPRESENTATION('material name',(#16972),#62693);
#16851=REPRESENTATION('density',(#16652),#62693);
#16852=REPRESENTATION('material name',(#16973),#62694);
#16853=REPRESENTATION('density',(#16653),#62694);
#16854=REPRESENTATION('material name',(#16974),#62695);
#16855=REPRESENTATION('density',(#16654),#62695);
#16856=REPRESENTATION('material name',(#16975),#62696);
#16857=REPRESENTATION('density',(#16655),#62696);
#16858=REPRESENTATION('material name',(#16976),#62697);
#16859=REPRESENTATION('density',(#16656),#62697);
#16860=REPRESENTATION('material name',(#16977),#62699);
#16861=REPRESENTATION('density',(#16657),#62699);
#16862=REPRESENTATION('material name',(#16978),#62700);
#16863=REPRESENTATION('density',(#16658),#62700);
#16864=REPRESENTATION('material name',(#16979),#62701);
#16865=REPRESENTATION('density',(#16659),#62701);
#16866=REPRESENTATION('material name',(#16980),#62702);
#16867=REPRESENTATION('density',(#16660),#62702);
#16868=REPRESENTATION('material name',(#16981),#62703);
#16869=REPRESENTATION('density',(#16661),#62703);
#16870=REPRESENTATION('material name',(#16982),#62705);
#16871=REPRESENTATION('density',(#16662),#62705);
#16872=REPRESENTATION('material name',(#16983),#62706);
#16873=REPRESENTATION('density',(#16663),#62706);
#16874=REPRESENTATION('material name',(#16984),#62707);
#16875=REPRESENTATION('density',(#16664),#62707);
#16876=REPRESENTATION('material name',(#16985),#62708);
#16877=REPRESENTATION('density',(#16665),#62708);
#16878=REPRESENTATION('material name',(#16986),#62709);
#16879=REPRESENTATION('density',(#16666),#62709);
#16880=REPRESENTATION('material name',(#16987),#62710);
#16881=REPRESENTATION('density',(#16667),#62710);
#16882=REPRESENTATION('material name',(#16988),#62711);
#16883=REPRESENTATION('density',(#16668),#62711);
#16884=REPRESENTATION('material name',(#16989),#62712);
#16885=REPRESENTATION('density',(#16669),#62712);
#16886=REPRESENTATION('material name',(#16990),#62713);
#16887=REPRESENTATION('density',(#16670),#62713);
#16888=REPRESENTATION('material name',(#16991),#62714);
#16889=REPRESENTATION('density',(#16671),#62714);
#16890=REPRESENTATION('material name',(#16992),#62715);
#16891=REPRESENTATION('density',(#16672),#62715);
#16892=REPRESENTATION('material name',(#16993),#62716);
#16893=REPRESENTATION('density',(#16673),#62716);
#16894=REPRESENTATION('material name',(#16994),#62718);
#16895=REPRESENTATION('density',(#16674),#62718);
#16896=REPRESENTATION('material name',(#16995),#62719);
#16897=REPRESENTATION('density',(#16675),#62719);
#16898=REPRESENTATION('material name',(#16996),#62720);
#16899=REPRESENTATION('density',(#16676),#62720);
#16900=REPRESENTATION('material name',(#16997),#62721);
#16901=REPRESENTATION('density',(#16677),#62721);
#16902=REPRESENTATION('material name',(#16998),#62722);
#16903=REPRESENTATION('density',(#16678),#62722);
#16904=REPRESENTATION('material name',(#16999),#62723);
#16905=REPRESENTATION('density',(#16679),#62723);
#16906=REPRESENTATION('material name',(#17000),#62724);
#16907=REPRESENTATION('density',(#16680),#62724);
#16908=REPRESENTATION('material name',(#17001),#62725);
#16909=REPRESENTATION('density',(#16681),#62725);
#16910=REPRESENTATION('material name',(#17002),#62726);
#16911=REPRESENTATION('density',(#16682),#62726);
#16912=REPRESENTATION('material name',(#17003),#62727);
#16913=REPRESENTATION('density',(#16683),#62727);
#16914=REPRESENTATION('material name',(#17004),#62728);
#16915=REPRESENTATION('density',(#16684),#62728);
#16916=REPRESENTATION('material name',(#17005),#62730);
#16917=REPRESENTATION('density',(#16685),#62730);
#16918=REPRESENTATION('material name',(#17006),#62731);
#16919=REPRESENTATION('density',(#16686),#62731);
#16920=REPRESENTATION('material name',(#17007),#62732);
#16921=REPRESENTATION('density',(#16687),#62732);
#16922=REPRESENTATION('material name',(#17008),#62733);
#16923=REPRESENTATION('density',(#16688),#62733);
#16924=REPRESENTATION('material name',(#17009),#62734);
#16925=REPRESENTATION('density',(#16689),#62734);
#16926=REPRESENTATION('material name',(#17010),#62736);
#16927=REPRESENTATION('density',(#16690),#62736);
#16928=REPRESENTATION('material name',(#17011),#62737);
#16929=REPRESENTATION('density',(#16691),#62737);
#16930=REPRESENTATION('material name',(#17012),#62738);
#16931=REPRESENTATION('density',(#16692),#62738);
#16932=REPRESENTATION('material name',(#17013),#62739);
#16933=REPRESENTATION('density',(#16693),#62739);
#16934=REPRESENTATION('material name',(#17014),#62740);
#16935=REPRESENTATION('density',(#16694),#62740);
#16936=REPRESENTATION('material name',(#17015),#62741);
#16937=REPRESENTATION('density',(#16695),#62741);
#16938=REPRESENTATION('material name',(#17016),#62742);
#16939=REPRESENTATION('density',(#16696),#62742);
#16940=REPRESENTATION('material name',(#17017),#62744);
#16941=REPRESENTATION('density',(#16697),#62744);
#16942=REPRESENTATION('material name',(#17018),#62745);
#16943=REPRESENTATION('density',(#16698),#62745);
#16944=REPRESENTATION('material name',(#17019),#62746);
#16945=REPRESENTATION('density',(#16699),#62746);
#16946=REPRESENTATION('material name',(#17020),#62747);
#16947=REPRESENTATION('density',(#16700),#62747);
#16948=REPRESENTATION('material name',(#17021),#62748);
#16949=REPRESENTATION('density',(#16701),#62748);
#16950=REPRESENTATION('material name',(#17022),#62749);
#16951=REPRESENTATION('density',(#16702),#62749);
#16952=REPRESENTATION('material name',(#17023),#62750);
#16953=REPRESENTATION('density',(#16703),#62750);
#16954=REPRESENTATION('material name',(#17024),#62751);
#16955=REPRESENTATION('density',(#16704),#62751);
#16956=REPRESENTATION('material name',(#17025),#62752);
#16957=REPRESENTATION('density',(#16705),#62752);
#16958=REPRESENTATION('material name',(#17026),#62753);
#16959=REPRESENTATION('density',(#16706),#62753);
#16960=REPRESENTATION('material name',(#17027),#62754);
#16961=REPRESENTATION('density',(#16707),#62754);
#16962=REPRESENTATION('material name',(#17028),#62755);
#16963=REPRESENTATION('density',(#16708),#62755);
#16964=REPRESENTATION('material name',(#17029),#62757);
#16965=REPRESENTATION('density',(#16709),#62757);
#16966=DESCRIPTIVE_REPRESENTATION_ITEM('Steel','Steel');
#16967=DESCRIPTIVE_REPRESENTATION_ITEM('Steel','Steel');
#16968=DESCRIPTIVE_REPRESENTATION_ITEM('Steel','Steel');
#16969=DESCRIPTIVE_REPRESENTATION_ITEM('Steel','Steel');
#16970=DESCRIPTIVE_REPRESENTATION_ITEM('Steel','Steel');
#16971=DESCRIPTIVE_REPRESENTATION_ITEM('Steel','Steel');
#16972=DESCRIPTIVE_REPRESENTATION_ITEM('Steel','Steel');
#16973=DESCRIPTIVE_REPRESENTATION_ITEM('Steel','Steel');
#16974=DESCRIPTIVE_REPRESENTATION_ITEM('Steel','Steel');
#16975=DESCRIPTIVE_REPRESENTATION_ITEM('Steel','Steel');
#16976=DESCRIPTIVE_REPRESENTATION_ITEM('Steel','Steel');
#16977=DESCRIPTIVE_REPRESENTATION_ITEM('Steel','Steel');
#16978=DESCRIPTIVE_REPRESENTATION_ITEM('Steel','Steel');
#16979=DESCRIPTIVE_REPRESENTATION_ITEM('Steel','Steel');
#16980=DESCRIPTIVE_REPRESENTATION_ITEM('Steel','Steel');
#16981=DESCRIPTIVE_REPRESENTATION_ITEM('Steel','Steel');
#16982=DESCRIPTIVE_REPRESENTATION_ITEM('Steel','Steel');
#16983=DESCRIPTIVE_REPRESENTATION_ITEM('Steel','Steel');
#16984=DESCRIPTIVE_REPRESENTATION_ITEM('Steel','Steel');
#16985=DESCRIPTIVE_REPRESENTATION_ITEM('Steel','Steel');
#16986=DESCRIPTIVE_REPRESENTATION_ITEM('Steel','Steel');
#16987=DESCRIPTIVE_REPRESENTATION_ITEM('Steel','Steel');
#16988=DESCRIPTIVE_REPRESENTATION_ITEM('Steel','Steel');
#16989=DESCRIPTIVE_REPRESENTATION_ITEM('Steel','Steel');
#16990=DESCRIPTIVE_REPRESENTATION_ITEM('Steel','Steel');
#16991=DESCRIPTIVE_REPRESENTATION_ITEM('Steel','Steel');
#16992=DESCRIPTIVE_REPRESENTATION_ITEM('Steel','Steel');
#16993=DESCRIPTIVE_REPRESENTATION_ITEM('Steel','Steel');
#16994=DESCRIPTIVE_REPRESENTATION_ITEM('Steel','Steel');
#16995=DESCRIPTIVE_REPRESENTATION_ITEM('Steel','Steel');
#16996=DESCRIPTIVE_REPRESENTATION_ITEM('Steel','Steel');
#16997=DESCRIPTIVE_REPRESENTATION_ITEM('Steel','Steel');
#16998=DESCRIPTIVE_REPRESENTATION_ITEM('Steel','Steel');
#16999=DESCRIPTIVE_REPRESENTATION_ITEM('Steel','Steel');
#17000=DESCRIPTIVE_REPRESENTATION_ITEM('Steel','Steel');
#17001=DESCRIPTIVE_REPRESENTATION_ITEM('Steel','Steel');
#17002=DESCRIPTIVE_REPRESENTATION_ITEM('Steel','Steel');
#17003=DESCRIPTIVE_REPRESENTATION_ITEM('Steel','Steel');
#17004=DESCRIPTIVE_REPRESENTATION_ITEM('Steel','Steel');
#17005=DESCRIPTIVE_REPRESENTATION_ITEM('Steel','Steel');
#17006=DESCRIPTIVE_REPRESENTATION_ITEM('Steel','Steel');
#17007=DESCRIPTIVE_REPRESENTATION_ITEM('Steel','Steel');
#17008=DESCRIPTIVE_REPRESENTATION_ITEM('Steel','Steel');
#17009=DESCRIPTIVE_REPRESENTATION_ITEM('Steel','Steel');
#17010=DESCRIPTIVE_REPRESENTATION_ITEM('Steel','Steel');
#17011=DESCRIPTIVE_REPRESENTATION_ITEM('Steel','Steel');
#17012=DESCRIPTIVE_REPRESENTATION_ITEM('Steel','Steel');
#17013=DESCRIPTIVE_REPRESENTATION_ITEM('Steel','Steel');
#17014=DESCRIPTIVE_REPRESENTATION_ITEM('Steel','Steel');
#17015=DESCRIPTIVE_REPRESENTATION_ITEM('Steel','Steel');
#17016=DESCRIPTIVE_REPRESENTATION_ITEM('Steel','Steel');
#17017=DESCRIPTIVE_REPRESENTATION_ITEM('Steel','Steel');
#17018=DESCRIPTIVE_REPRESENTATION_ITEM('Steel','Steel');
#17019=DESCRIPTIVE_REPRESENTATION_ITEM('Steel','Steel');
#17020=DESCRIPTIVE_REPRESENTATION_ITEM('Steel','Steel');
#17021=DESCRIPTIVE_REPRESENTATION_ITEM('Steel','Steel');
#17022=DESCRIPTIVE_REPRESENTATION_ITEM('Steel','Steel');
#17023=DESCRIPTIVE_REPRESENTATION_ITEM('Steel','Steel');
#17024=DESCRIPTIVE_REPRESENTATION_ITEM('Steel','Steel');
#17025=DESCRIPTIVE_REPRESENTATION_ITEM('Steel','Steel');
#17026=DESCRIPTIVE_REPRESENTATION_ITEM('Steel','Steel');
#17027=DESCRIPTIVE_REPRESENTATION_ITEM('Steel','Steel');
#17028=DESCRIPTIVE_REPRESENTATION_ITEM('Steel','Steel');
#17029=DESCRIPTIVE_REPRESENTATION_ITEM('Steel','Steel');
#17030=PROPERTY_DEFINITION('material property','material name',#63107);
#17031=PROPERTY_DEFINITION('material property','density of part',#63107);
#17032=PROPERTY_DEFINITION('material property','material name',#63108);
#17033=PROPERTY_DEFINITION('material property','density of part',#63108);
#17034=PROPERTY_DEFINITION('material property','material name',#63109);
#17035=PROPERTY_DEFINITION('material property','density of part',#63109);
#17036=PROPERTY_DEFINITION('material property','material name',#63110);
#17037=PROPERTY_DEFINITION('material property','density of part',#63110);
#17038=PROPERTY_DEFINITION('material property','material name',#63111);
#17039=PROPERTY_DEFINITION('material property','density of part',#63111);
#17040=PROPERTY_DEFINITION('material property','material name',#63112);
#17041=PROPERTY_DEFINITION('material property','density of part',#63112);
#17042=PROPERTY_DEFINITION('material property','material name',#63113);
#17043=PROPERTY_DEFINITION('material property','density of part',#63113);
#17044=PROPERTY_DEFINITION('material property','material name',#63114);
#17045=PROPERTY_DEFINITION('material property','density of part',#63114);
#17046=PROPERTY_DEFINITION('material property','material name',#63115);
#17047=PROPERTY_DEFINITION('material property','density of part',#63115);
#17048=PROPERTY_DEFINITION('material property','material name',#63116);
#17049=PROPERTY_DEFINITION('material property','density of part',#63116);
#17050=PROPERTY_DEFINITION('material property','material name',#63117);
#17051=PROPERTY_DEFINITION('material property','density of part',#63117);
#17052=PROPERTY_DEFINITION('material property','material name',#63119);
#17053=PROPERTY_DEFINITION('material property','density of part',#63119);
#17054=PROPERTY_DEFINITION('material property','material name',#63120);
#17055=PROPERTY_DEFINITION('material property','density of part',#63120);
#17056=PROPERTY_DEFINITION('material property','material name',#63121);
#17057=PROPERTY_DEFINITION('material property','density of part',#63121);
#17058=PROPERTY_DEFINITION('material property','material name',#63122);
#17059=PROPERTY_DEFINITION('material property','density of part',#63122);
#17060=PROPERTY_DEFINITION('material property','material name',#63123);
#17061=PROPERTY_DEFINITION('material property','density of part',#63123);
#17062=PROPERTY_DEFINITION('material property','material name',#63125);
#17063=PROPERTY_DEFINITION('material property','density of part',#63125);
#17064=PROPERTY_DEFINITION('material property','material name',#63126);
#17065=PROPERTY_DEFINITION('material property','density of part',#63126);
#17066=PROPERTY_DEFINITION('material property','material name',#63127);
#17067=PROPERTY_DEFINITION('material property','density of part',#63127);
#17068=PROPERTY_DEFINITION('material property','material name',#63128);
#17069=PROPERTY_DEFINITION('material property','density of part',#63128);
#17070=PROPERTY_DEFINITION('material property','material name',#63129);
#17071=PROPERTY_DEFINITION('material property','density of part',#63129);
#17072=PROPERTY_DEFINITION('material property','material name',#63130);
#17073=PROPERTY_DEFINITION('material property','density of part',#63130);
#17074=PROPERTY_DEFINITION('material property','material name',#63131);
#17075=PROPERTY_DEFINITION('material property','density of part',#63131);
#17076=PROPERTY_DEFINITION('material property','material name',#63132);
#17077=PROPERTY_DEFINITION('material property','density of part',#63132);
#17078=PROPERTY_DEFINITION('material property','material name',#63133);
#17079=PROPERTY_DEFINITION('material property','density of part',#63133);
#17080=PROPERTY_DEFINITION('material property','material name',#63134);
#17081=PROPERTY_DEFINITION('material property','density of part',#63134);
#17082=PROPERTY_DEFINITION('material property','material name',#63135);
#17083=PROPERTY_DEFINITION('material property','density of part',#63135);
#17084=PROPERTY_DEFINITION('material property','material name',#63136);
#17085=PROPERTY_DEFINITION('material property','density of part',#63136);
#17086=PROPERTY_DEFINITION('material property','material name',#63138);
#17087=PROPERTY_DEFINITION('material property','density of part',#63138);
#17088=PROPERTY_DEFINITION('material property','material name',#63139);
#17089=PROPERTY_DEFINITION('material property','density of part',#63139);
#17090=PROPERTY_DEFINITION('material property','material name',#63140);
#17091=PROPERTY_DEFINITION('material property','density of part',#63140);
#17092=PROPERTY_DEFINITION('material property','material name',#63141);
#17093=PROPERTY_DEFINITION('material property','density of part',#63141);
#17094=PROPERTY_DEFINITION('material property','material name',#63142);
#17095=PROPERTY_DEFINITION('material property','density of part',#63142);
#17096=PROPERTY_DEFINITION('material property','material name',#63143);
#17097=PROPERTY_DEFINITION('material property','density of part',#63143);
#17098=PROPERTY_DEFINITION('material property','material name',#63144);
#17099=PROPERTY_DEFINITION('material property','density of part',#63144);
#17100=PROPERTY_DEFINITION('material property','material name',#63145);
#17101=PROPERTY_DEFINITION('material property','density of part',#63145);
#17102=PROPERTY_DEFINITION('material property','material name',#63146);
#17103=PROPERTY_DEFINITION('material property','density of part',#63146);
#17104=PROPERTY_DEFINITION('material property','material name',#63147);
#17105=PROPERTY_DEFINITION('material property','density of part',#63147);
#17106=PROPERTY_DEFINITION('material property','material name',#63148);
#17107=PROPERTY_DEFINITION('material property','density of part',#63148);
#17108=PROPERTY_DEFINITION('material property','material name',#63150);
#17109=PROPERTY_DEFINITION('material property','density of part',#63150);
#17110=PROPERTY_DEFINITION('material property','material name',#63151);
#17111=PROPERTY_DEFINITION('material property','density of part',#63151);
#17112=PROPERTY_DEFINITION('material property','material name',#63152);
#17113=PROPERTY_DEFINITION('material property','density of part',#63152);
#17114=PROPERTY_DEFINITION('material property','material name',#63153);
#17115=PROPERTY_DEFINITION('material property','density of part',#63153);
#17116=PROPERTY_DEFINITION('material property','material name',#63154);
#17117=PROPERTY_DEFINITION('material property','density of part',#63154);
#17118=PROPERTY_DEFINITION('material property','material name',#63156);
#17119=PROPERTY_DEFINITION('material property','density of part',#63156);
#17120=PROPERTY_DEFINITION('material property','material name',#63157);
#17121=PROPERTY_DEFINITION('material property','density of part',#63157);
#17122=PROPERTY_DEFINITION('material property','material name',#63158);
#17123=PROPERTY_DEFINITION('material property','density of part',#63158);
#17124=PROPERTY_DEFINITION('material property','material name',#63159);
#17125=PROPERTY_DEFINITION('material property','density of part',#63159);
#17126=PROPERTY_DEFINITION('material property','material name',#63160);
#17127=PROPERTY_DEFINITION('material property','density of part',#63160);
#17128=PROPERTY_DEFINITION('material property','material name',#63161);
#17129=PROPERTY_DEFINITION('material property','density of part',#63161);
#17130=PROPERTY_DEFINITION('material property','material name',#63162);
#17131=PROPERTY_DEFINITION('material property','density of part',#63162);
#17132=PROPERTY_DEFINITION('material property','material name',#63164);
#17133=PROPERTY_DEFINITION('material property','density of part',#63164);
#17134=PROPERTY_DEFINITION('material property','material name',#63165);
#17135=PROPERTY_DEFINITION('material property','density of part',#63165);
#17136=PROPERTY_DEFINITION('material property','material name',#63166);
#17137=PROPERTY_DEFINITION('material property','density of part',#63166);
#17138=PROPERTY_DEFINITION('material property','material name',#63167);
#17139=PROPERTY_DEFINITION('material property','density of part',#63167);
#17140=PROPERTY_DEFINITION('material property','material name',#63168);
#17141=PROPERTY_DEFINITION('material property','density of part',#63168);
#17142=PROPERTY_DEFINITION('material property','material name',#63169);
#17143=PROPERTY_DEFINITION('material property','density of part',#63169);
#17144=PROPERTY_DEFINITION('material property','material name',#63170);
#17145=PROPERTY_DEFINITION('material property','density of part',#63170);
#17146=PROPERTY_DEFINITION('material property','material name',#63171);
#17147=PROPERTY_DEFINITION('material property','density of part',#63171);
#17148=PROPERTY_DEFINITION('material property','material name',#63172);
#17149=PROPERTY_DEFINITION('material property','density of part',#63172);
#17150=PROPERTY_DEFINITION('material property','material name',#63173);
#17151=PROPERTY_DEFINITION('material property','density of part',#63173);
#17152=PROPERTY_DEFINITION('material property','material name',#63174);
#17153=PROPERTY_DEFINITION('material property','density of part',#63174);
#17154=PROPERTY_DEFINITION('material property','material name',#63175);
#17155=PROPERTY_DEFINITION('material property','density of part',#63175);
#17156=PROPERTY_DEFINITION('material property','material name',#63177);
#17157=PROPERTY_DEFINITION('material property','density of part',#63177);
#17158=AXIS2_PLACEMENT_3D('',#23309,#18831,#18832);
#17159=AXIS2_PLACEMENT_3D('',#23310,#18833,#18834);
#17160=AXIS2_PLACEMENT_3D('',#23311,#18835,#18836);
#17161=AXIS2_PLACEMENT_3D('',#23312,#18837,#18838);
#17162=AXIS2_PLACEMENT_3D('',#23314,#18839,#18840);
#17163=AXIS2_PLACEMENT_3D('',#23317,#18842,#18843);
#17164=AXIS2_PLACEMENT_3D('',#23318,#18844,#18845);
#17165=AXIS2_PLACEMENT_3D('',#23320,#18846,#18847);
#17166=AXIS2_PLACEMENT_3D('',#23323,#18849,#18850);
#17167=AXIS2_PLACEMENT_3D('',#23324,#18851,#18852);
#17168=AXIS2_PLACEMENT_3D('',#23326,#18853,#18854);
#17169=AXIS2_PLACEMENT_3D('',#23329,#18856,#18857);
#17170=AXIS2_PLACEMENT_3D('',#23330,#18858,#18859);
#17171=AXIS2_PLACEMENT_3D('',#23339,#18864,#18865);
#17172=AXIS2_PLACEMENT_3D('',#23345,#18869,#18870);
#17173=AXIS2_PLACEMENT_3D('',#23351,#18874,#18875);
#17174=AXIS2_PLACEMENT_3D('',#23354,#18878,#18879);
#17175=AXIS2_PLACEMENT_3D('',#23355,#18880,#18881);
#17176=AXIS2_PLACEMENT_3D('',#23356,#18882,#18883);
#17177=AXIS2_PLACEMENT_3D('',#23357,#18884,#18885);
#17178=AXIS2_PLACEMENT_3D('',#23359,#18886,#18887);
#17179=AXIS2_PLACEMENT_3D('',#23362,#18889,#18890);
#17180=AXIS2_PLACEMENT_3D('',#23363,#18891,#18892);
#17181=AXIS2_PLACEMENT_3D('',#23365,#18893,#18894);
#17182=AXIS2_PLACEMENT_3D('',#23368,#18896,#18897);
#17183=AXIS2_PLACEMENT_3D('',#23369,#18898,#18899);
#17184=AXIS2_PLACEMENT_3D('',#23371,#18900,#18901);
#17185=AXIS2_PLACEMENT_3D('',#23374,#18903,#18904);
#17186=AXIS2_PLACEMENT_3D('',#23375,#18905,#18906);
#17187=AXIS2_PLACEMENT_3D('',#23377,#18907,#18908);
#17188=AXIS2_PLACEMENT_3D('',#23380,#18910,#18911);
#17189=AXIS2_PLACEMENT_3D('',#23381,#18912,#18913);
#17190=AXIS2_PLACEMENT_3D('',#23383,#18914,#18915);
#17191=AXIS2_PLACEMENT_3D('',#23386,#18917,#18918);
#17192=AXIS2_PLACEMENT_3D('',#23387,#18919,#18920);
#17193=AXIS2_PLACEMENT_3D('',#23389,#18921,#18922);
#17194=AXIS2_PLACEMENT_3D('',#23392,#18924,#18925);
#17195=AXIS2_PLACEMENT_3D('',#23393,#18926,#18927);
#17196=AXIS2_PLACEMENT_3D('',#23395,#18928,#18929);
#17197=AXIS2_PLACEMENT_3D('',#23398,#18931,#18932);
#17198=AXIS2_PLACEMENT_3D('',#23399,#18933,#18934);
#17199=AXIS2_PLACEMENT_3D('',#23401,#18935,#18936);
#17200=AXIS2_PLACEMENT_3D('',#23404,#18938,#18939);
#17201=AXIS2_PLACEMENT_3D('',#23405,#18940,#18941);
#17202=AXIS2_PLACEMENT_3D('',#23407,#18942,#18943);
#17203=AXIS2_PLACEMENT_3D('',#23410,#18945,#18946);
#17204=AXIS2_PLACEMENT_3D('',#23411,#18947,#18948);
#17205=AXIS2_PLACEMENT_3D('',#23413,#18949,#18950);
#17206=AXIS2_PLACEMENT_3D('',#23416,#18952,#18953);
#17207=AXIS2_PLACEMENT_3D('',#23417,#18954,#18955);
#17208=AXIS2_PLACEMENT_3D('',#23419,#18956,#18957);
#17209=AXIS2_PLACEMENT_3D('',#23422,#18959,#18960);
#17210=AXIS2_PLACEMENT_3D('',#23423,#18961,#18962);
#17211=AXIS2_PLACEMENT_3D('',#23425,#18963,#18964);
#17212=AXIS2_PLACEMENT_3D('',#23428,#18966,#18967);
#17213=AXIS2_PLACEMENT_3D('',#23429,#18968,#18969);
#17214=AXIS2_PLACEMENT_3D('',#23431,#18970,#18971);
#17215=AXIS2_PLACEMENT_3D('',#23434,#18973,#18974);
#17216=AXIS2_PLACEMENT_3D('',#23435,#18975,#18976);
#17217=AXIS2_PLACEMENT_3D('',#23437,#18977,#18978);
#17218=AXIS2_PLACEMENT_3D('',#23440,#18980,#18981);
#17219=AXIS2_PLACEMENT_3D('',#23441,#18982,#18983);
#17220=AXIS2_PLACEMENT_3D('',#23443,#18984,#18985);
#17221=AXIS2_PLACEMENT_3D('',#23446,#18987,#18988);
#17222=AXIS2_PLACEMENT_3D('',#23447,#18989,#18990);
#17223=AXIS2_PLACEMENT_3D('',#23449,#18991,#18992);
#17224=AXIS2_PLACEMENT_3D('',#23452,#18994,#18995);
#17225=AXIS2_PLACEMENT_3D('',#23453,#18996,#18997);
#17226=AXIS2_PLACEMENT_3D('',#23455,#18998,#18999);
#17227=AXIS2_PLACEMENT_3D('',#23458,#19001,#19002);
#17228=AXIS2_PLACEMENT_3D('',#23459,#19003,#19004);
#17229=AXIS2_PLACEMENT_3D('',#23461,#19005,#19006);
#17230=AXIS2_PLACEMENT_3D('',#23464,#19008,#19009);
#17231=AXIS2_PLACEMENT_3D('',#23465,#19010,#19011);
#17232=AXIS2_PLACEMENT_3D('',#23467,#19012,#19013);
#17233=AXIS2_PLACEMENT_3D('',#23470,#19015,#19016);
#17234=AXIS2_PLACEMENT_3D('',#23471,#19017,#19018);
#17235=AXIS2_PLACEMENT_3D('',#23473,#19019,#19020);
#17236=AXIS2_PLACEMENT_3D('',#23476,#19022,#19023);
#17237=AXIS2_PLACEMENT_3D('',#23477,#19024,#19025);
#17238=AXIS2_PLACEMENT_3D('',#23479,#19026,#19027);
#17239=AXIS2_PLACEMENT_3D('',#23482,#19029,#19030);
#17240=AXIS2_PLACEMENT_3D('',#23483,#19031,#19032);
#17241=AXIS2_PLACEMENT_3D('',#23485,#19033,#19034);
#17242=AXIS2_PLACEMENT_3D('',#23488,#19036,#19037);
#17243=AXIS2_PLACEMENT_3D('',#23489,#19038,#19039);
#17244=AXIS2_PLACEMENT_3D('',#23491,#19040,#19041);
#17245=AXIS2_PLACEMENT_3D('',#23494,#19043,#19044);
#17246=AXIS2_PLACEMENT_3D('',#23495,#19045,#19046);
#17247=AXIS2_PLACEMENT_3D('',#23497,#19047,#19048);
#17248=AXIS2_PLACEMENT_3D('',#23500,#19050,#19051);
#17249=AXIS2_PLACEMENT_3D('',#23501,#19052,#19053);
#17250=AXIS2_PLACEMENT_3D('',#23503,#19054,#19055);
#17251=AXIS2_PLACEMENT_3D('',#23506,#19057,#19058);
#17252=AXIS2_PLACEMENT_3D('',#23507,#19059,#19060);
#17253=AXIS2_PLACEMENT_3D('',#23516,#19065,#19066);
#17254=AXIS2_PLACEMENT_3D('',#23522,#19070,#19071);
#17255=AXIS2_PLACEMENT_3D('',#23531,#19076,#19077);
#17256=AXIS2_PLACEMENT_3D('',#23536,#19081,#19082);
#17257=AXIS2_PLACEMENT_3D('',#23540,#19085,#19086);
#17258=AXIS2_PLACEMENT_3D('',#23543,#19089,#19090);
#17259=AXIS2_PLACEMENT_3D('',#23544,#19091,#19092);
#17260=AXIS2_PLACEMENT_3D('',#23545,#19093,#19094);
#17261=AXIS2_PLACEMENT_3D('',#23546,#19095,#19096);
#17262=AXIS2_PLACEMENT_3D('',#23548,#19097,#19098);
#17263=AXIS2_PLACEMENT_3D('',#23551,#19100,#19101);
#17264=AXIS2_PLACEMENT_3D('',#23552,#19102,#19103);
#17265=AXIS2_PLACEMENT_3D('',#23554,#19104,#19105);
#17266=AXIS2_PLACEMENT_3D('',#23557,#19107,#19108);
#17267=AXIS2_PLACEMENT_3D('',#23558,#19109,#19110);
#17268=AXIS2_PLACEMENT_3D('',#23560,#19111,#19112);
#17269=AXIS2_PLACEMENT_3D('',#23563,#19114,#19115);
#17270=AXIS2_PLACEMENT_3D('',#23564,#19116,#19117);
#17271=AXIS2_PLACEMENT_3D('',#23566,#19118,#19119);
#17272=AXIS2_PLACEMENT_3D('',#23569,#19121,#19122);
#17273=AXIS2_PLACEMENT_3D('',#23570,#19123,#19124);
#17274=AXIS2_PLACEMENT_3D('',#23572,#19125,#19126);
#17275=AXIS2_PLACEMENT_3D('',#23575,#19128,#19129);
#17276=AXIS2_PLACEMENT_3D('',#23576,#19130,#19131);
#17277=AXIS2_PLACEMENT_3D('',#23578,#19132,#19133);
#17278=AXIS2_PLACEMENT_3D('',#23579,#19134,#19135);
#17279=AXIS2_PLACEMENT_3D('',#23582,#19137,#19138);
#17280=AXIS2_PLACEMENT_3D('',#23583,#19139,#19140);
#17281=AXIS2_PLACEMENT_3D('',#23585,#19141,#19142);
#17282=AXIS2_PLACEMENT_3D('',#23588,#19144,#19145);
#17283=AXIS2_PLACEMENT_3D('',#23589,#19146,#19147);
#17284=AXIS2_PLACEMENT_3D('',#23590,#19148,#19149);
#17285=AXIS2_PLACEMENT_3D('',#23591,#19150,#19151);
#17286=AXIS2_PLACEMENT_3D('',#23592,#19152,#19153);
#17287=AXIS2_PLACEMENT_3D('',#23594,#19154,#19155);
#17288=AXIS2_PLACEMENT_3D('',#23597,#19157,#19158);
#17289=AXIS2_PLACEMENT_3D('',#23598,#19159,#19160);
#17290=AXIS2_PLACEMENT_3D('',#23600,#19161,#19162);
#17291=AXIS2_PLACEMENT_3D('',#23603,#19164,#19165);
#17292=AXIS2_PLACEMENT_3D('',#23604,#19166,#19167);
#17293=AXIS2_PLACEMENT_3D('',#23606,#19168,#19169);
#17294=AXIS2_PLACEMENT_3D('',#23609,#19171,#19172);
#17295=AXIS2_PLACEMENT_3D('',#23610,#19173,#19174);
#17296=AXIS2_PLACEMENT_3D('',#23612,#19175,#19176);
#17297=AXIS2_PLACEMENT_3D('',#23615,#19178,#19179);
#17298=AXIS2_PLACEMENT_3D('',#23616,#19180,#19181);
#17299=AXIS2_PLACEMENT_3D('',#23618,#19182,#19183);
#17300=AXIS2_PLACEMENT_3D('',#23621,#19185,#19186);
#17301=AXIS2_PLACEMENT_3D('',#23622,#19187,#19188);
#17302=AXIS2_PLACEMENT_3D('',#23624,#19189,#19190);
#17303=AXIS2_PLACEMENT_3D('',#23625,#19191,#19192);
#17304=AXIS2_PLACEMENT_3D('',#23627,#19193,#19194);
#17305=AXIS2_PLACEMENT_3D('',#23629,#19196,#19197);
#17306=AXIS2_PLACEMENT_3D('',#23631,#19198,#19199);
#17307=AXIS2_PLACEMENT_3D('',#23634,#19201,#19202);
#17308=AXIS2_PLACEMENT_3D('',#23635,#19203,#19204);
#17309=AXIS2_PLACEMENT_3D('',#23636,#19205,#19206);
#17310=AXIS2_PLACEMENT_3D('',#23637,#19207,#19208);
#17311=AXIS2_PLACEMENT_3D('',#23638,#19209,#19210);
#17312=AXIS2_PLACEMENT_3D('',#23640,#19211,#19212);
#17313=AXIS2_PLACEMENT_3D('',#23643,#19214,#19215);
#17314=AXIS2_PLACEMENT_3D('',#23644,#19216,#19217);
#17315=AXIS2_PLACEMENT_3D('',#23646,#19218,#19219);
#17316=AXIS2_PLACEMENT_3D('',#23649,#19221,#19222);
#17317=AXIS2_PLACEMENT_3D('',#23650,#19223,#19224);
#17318=AXIS2_PLACEMENT_3D('',#23652,#19225,#19226);
#17319=AXIS2_PLACEMENT_3D('',#23655,#19228,#19229);
#17320=AXIS2_PLACEMENT_3D('',#23656,#19230,#19231);
#17321=AXIS2_PLACEMENT_3D('',#23658,#19232,#19233);
#17322=AXIS2_PLACEMENT_3D('',#23661,#19235,#19236);
#17323=AXIS2_PLACEMENT_3D('',#23662,#19237,#19238);
#17324=AXIS2_PLACEMENT_3D('',#23664,#19239,#19240);
#17325=AXIS2_PLACEMENT_3D('',#23667,#19242,#19243);
#17326=AXIS2_PLACEMENT_3D('',#23668,#19244,#19245);
#17327=AXIS2_PLACEMENT_3D('',#23670,#19246,#19247);
#17328=AXIS2_PLACEMENT_3D('',#23671,#19248,#19249);
#17329=AXIS2_PLACEMENT_3D('',#23674,#19251,#19252);
#17330=AXIS2_PLACEMENT_3D('',#23675,#19253,#19254);
#17331=AXIS2_PLACEMENT_3D('',#23677,#19255,#19256);
#17332=AXIS2_PLACEMENT_3D('',#23680,#19258,#19259);
#17333=AXIS2_PLACEMENT_3D('',#23681,#19260,#19261);
#17334=AXIS2_PLACEMENT_3D('',#23682,#19262,#19263);
#17335=AXIS2_PLACEMENT_3D('',#23683,#19264,#19265);
#17336=AXIS2_PLACEMENT_3D('',#23684,#19266,#19267);
#17337=AXIS2_PLACEMENT_3D('',#23686,#19268,#19269);
#17338=AXIS2_PLACEMENT_3D('',#23689,#19271,#19272);
#17339=AXIS2_PLACEMENT_3D('',#23690,#19273,#19274);
#17340=AXIS2_PLACEMENT_3D('',#23692,#19275,#19276);
#17341=AXIS2_PLACEMENT_3D('',#23695,#19278,#19279);
#17342=AXIS2_PLACEMENT_3D('',#23696,#19280,#19281);
#17343=AXIS2_PLACEMENT_3D('',#23698,#19282,#19283);
#17344=AXIS2_PLACEMENT_3D('',#23701,#19285,#19286);
#17345=AXIS2_PLACEMENT_3D('',#23702,#19287,#19288);
#17346=AXIS2_PLACEMENT_3D('',#23704,#19289,#19290);
#17347=AXIS2_PLACEMENT_3D('',#23707,#19292,#19293);
#17348=AXIS2_PLACEMENT_3D('',#23708,#19294,#19295);
#17349=AXIS2_PLACEMENT_3D('',#23710,#19296,#19297);
#17350=AXIS2_PLACEMENT_3D('',#23713,#19299,#19300);
#17351=AXIS2_PLACEMENT_3D('',#23714,#19301,#19302);
#17352=AXIS2_PLACEMENT_3D('',#23716,#19303,#19304);
#17353=AXIS2_PLACEMENT_3D('',#23717,#19305,#19306);
#17354=AXIS2_PLACEMENT_3D('',#23719,#19307,#19308);
#17355=AXIS2_PLACEMENT_3D('',#23721,#19310,#19311);
#17356=AXIS2_PLACEMENT_3D('',#23723,#19312,#19313);
#17357=AXIS2_PLACEMENT_3D('',#23726,#19315,#19316);
#17358=AXIS2_PLACEMENT_3D('',#23727,#19317,#19318);
#17359=AXIS2_PLACEMENT_3D('',#23728,#19319,#19320);
#17360=AXIS2_PLACEMENT_3D('',#23729,#19321,#19322);
#17361=AXIS2_PLACEMENT_3D('',#23730,#19323,#19324);
#17362=AXIS2_PLACEMENT_3D('',#23739,#19329,#19330);
#17363=AXIS2_PLACEMENT_3D('',#23745,#19334,#19335);
#17364=AXIS2_PLACEMENT_3D('',#23751,#19339,#19340);
#17365=AXIS2_PLACEMENT_3D('',#23757,#19344,#19345);
#17366=AXIS2_PLACEMENT_3D('',#23763,#19349,#19350);
#17367=AXIS2_PLACEMENT_3D('',#23766,#19353,#19354);
#17368=AXIS2_PLACEMENT_3D('',#23767,#19355,#19356);
#17369=AXIS2_PLACEMENT_3D('',#23768,#19357,#19358);
#17370=AXIS2_PLACEMENT_3D('',#23770,#19359,#19360);
#17371=AXIS2_PLACEMENT_3D('',#23771,#19361,#19362);
#17372=AXIS2_PLACEMENT_3D('',#23773,#19363,#19364);
#17373=AXIS2_PLACEMENT_3D('',#23774,#19365,#19366);
#17374=AXIS2_PLACEMENT_3D('',#23776,#19367,#19368);
#17375=AXIS2_PLACEMENT_3D('',#23778,#19370,#19371);
#17376=AXIS2_PLACEMENT_3D('',#23780,#19372,#19373);
#17377=AXIS2_PLACEMENT_3D('',#23782,#19375,#19376);
#17378=AXIS2_PLACEMENT_3D('',#23784,#19377,#19378);
#17379=AXIS2_PLACEMENT_3D('',#23786,#19380,#19381);
#17380=AXIS2_PLACEMENT_3D('',#23788,#19382,#19383);
#17381=AXIS2_PLACEMENT_3D('',#23789,#19384,#19385);
#17382=AXIS2_PLACEMENT_3D('',#23791,#19386,#19387);
#17383=AXIS2_PLACEMENT_3D('',#23793,#19389,#19390);
#17384=AXIS2_PLACEMENT_3D('',#23795,#19392,#19393);
#17385=AXIS2_PLACEMENT_3D('',#23796,#19394,#19395);
#17386=AXIS2_PLACEMENT_3D('',#23798,#19396,#19397);
#17387=AXIS2_PLACEMENT_3D('',#23801,#19399,#19400);
#17388=AXIS2_PLACEMENT_3D('',#23802,#19401,#19402);
#17389=AXIS2_PLACEMENT_3D('',#23804,#19403,#19404);
#17390=AXIS2_PLACEMENT_3D('',#23807,#19406,#19407);
#17391=AXIS2_PLACEMENT_3D('',#23808,#19408,#19409);
#17392=AXIS2_PLACEMENT_3D('',#23810,#19410,#19411);
#17393=AXIS2_PLACEMENT_3D('',#23813,#19413,#19414);
#17394=AXIS2_PLACEMENT_3D('',#23814,#19415,#19416);
#17395=AXIS2_PLACEMENT_3D('',#23816,#19417,#19418);
#17396=AXIS2_PLACEMENT_3D('',#23819,#19420,#19421);
#17397=AXIS2_PLACEMENT_3D('',#23820,#19422,#19423);
#17398=AXIS2_PLACEMENT_3D('',#23822,#19424,#19425);
#17399=AXIS2_PLACEMENT_3D('',#23825,#19427,#19428);
#17400=AXIS2_PLACEMENT_3D('',#23826,#19429,#19430);
#17401=AXIS2_PLACEMENT_3D('',#23828,#19431,#19432);
#17402=AXIS2_PLACEMENT_3D('',#23829,#19433,#19434);
#17403=AXIS2_PLACEMENT_3D('',#23832,#19436,#19437);
#17404=AXIS2_PLACEMENT_3D('',#23833,#19438,#19439);
#17405=AXIS2_PLACEMENT_3D('',#23835,#19440,#19441);
#17406=AXIS2_PLACEMENT_3D('',#23838,#19443,#19444);
#17407=AXIS2_PLACEMENT_3D('',#23839,#19445,#19446);
#17408=AXIS2_PLACEMENT_3D('',#23840,#19447,#19448);
#17409=AXIS2_PLACEMENT_3D('',#23841,#19449,#19450);
#17410=AXIS2_PLACEMENT_3D('',#23842,#19451,#19452);
#17411=AXIS2_PLACEMENT_3D('',#23844,#19453,#19454);
#17412=AXIS2_PLACEMENT_3D('',#23847,#19456,#19457);
#17413=AXIS2_PLACEMENT_3D('',#23848,#19458,#19459);
#17414=AXIS2_PLACEMENT_3D('',#23850,#19460,#19461);
#17415=AXIS2_PLACEMENT_3D('',#23853,#19463,#19464);
#17416=AXIS2_PLACEMENT_3D('',#23854,#19465,#19466);
#17417=AXIS2_PLACEMENT_3D('',#23856,#19467,#19468);
#17418=AXIS2_PLACEMENT_3D('',#23859,#19470,#19471);
#17419=AXIS2_PLACEMENT_3D('',#23860,#19472,#19473);
#17420=AXIS2_PLACEMENT_3D('',#23862,#19474,#19475);
#17421=AXIS2_PLACEMENT_3D('',#23865,#19477,#19478);
#17422=AXIS2_PLACEMENT_3D('',#23866,#19479,#19480);
#17423=AXIS2_PLACEMENT_3D('',#23868,#19481,#19482);
#17424=AXIS2_PLACEMENT_3D('',#23871,#19484,#19485);
#17425=AXIS2_PLACEMENT_3D('',#23872,#19486,#19487);
#17426=AXIS2_PLACEMENT_3D('',#23874,#19488,#19489);
#17427=AXIS2_PLACEMENT_3D('',#23875,#19490,#19491);
#17428=AXIS2_PLACEMENT_3D('',#23877,#19492,#19493);
#17429=AXIS2_PLACEMENT_3D('',#23879,#19495,#19496);
#17430=AXIS2_PLACEMENT_3D('',#23881,#19497,#19498);
#17431=AXIS2_PLACEMENT_3D('',#23884,#19500,#19501);
#17432=AXIS2_PLACEMENT_3D('',#23885,#19502,#19503);
#17433=AXIS2_PLACEMENT_3D('',#23886,#19504,#19505);
#17434=AXIS2_PLACEMENT_3D('',#23887,#19506,#19507);
#17435=AXIS2_PLACEMENT_3D('',#23888,#19508,#19509);
#17436=AXIS2_PLACEMENT_3D('',#23890,#19510,#19511);
#17437=AXIS2_PLACEMENT_3D('',#23893,#19513,#19514);
#17438=AXIS2_PLACEMENT_3D('',#23894,#19515,#19516);
#17439=AXIS2_PLACEMENT_3D('',#23896,#19517,#19518);
#17440=AXIS2_PLACEMENT_3D('',#23899,#19520,#19521);
#17441=AXIS2_PLACEMENT_3D('',#23900,#19522,#19523);
#17442=AXIS2_PLACEMENT_3D('',#23902,#19524,#19525);
#17443=AXIS2_PLACEMENT_3D('',#23905,#19527,#19528);
#17444=AXIS2_PLACEMENT_3D('',#23906,#19529,#19530);
#17445=AXIS2_PLACEMENT_3D('',#23908,#19531,#19532);
#17446=AXIS2_PLACEMENT_3D('',#23911,#19534,#19535);
#17447=AXIS2_PLACEMENT_3D('',#23912,#19536,#19537);
#17448=AXIS2_PLACEMENT_3D('',#23914,#19538,#19539);
#17449=AXIS2_PLACEMENT_3D('',#23917,#19541,#19542);
#17450=AXIS2_PLACEMENT_3D('',#23918,#19543,#19544);
#17451=AXIS2_PLACEMENT_3D('',#23920,#19545,#19546);
#17452=AXIS2_PLACEMENT_3D('',#23921,#19547,#19548);
#17453=AXIS2_PLACEMENT_3D('',#23924,#19550,#19551);
#17454=AXIS2_PLACEMENT_3D('',#23925,#19552,#19553);
#17455=AXIS2_PLACEMENT_3D('',#23927,#19554,#19555);
#17456=AXIS2_PLACEMENT_3D('',#23930,#19557,#19558);
#17457=AXIS2_PLACEMENT_3D('',#23931,#19559,#19560);
#17458=AXIS2_PLACEMENT_3D('',#23932,#19561,#19562);
#17459=AXIS2_PLACEMENT_3D('',#23933,#19563,#19564);
#17460=AXIS2_PLACEMENT_3D('',#23934,#19565,#19566);
#17461=AXIS2_PLACEMENT_3D('',#23936,#19567,#19568);
#17462=AXIS2_PLACEMENT_3D('',#23939,#19570,#19571);
#17463=AXIS2_PLACEMENT_3D('',#23940,#19572,#19573);
#17464=AXIS2_PLACEMENT_3D('',#23942,#19574,#19575);
#17465=AXIS2_PLACEMENT_3D('',#23945,#19577,#19578);
#17466=AXIS2_PLACEMENT_3D('',#23946,#19579,#19580);
#17467=AXIS2_PLACEMENT_3D('',#23948,#19581,#19582);
#17468=AXIS2_PLACEMENT_3D('',#23951,#19584,#19585);
#17469=AXIS2_PLACEMENT_3D('',#23952,#19586,#19587);
#17470=AXIS2_PLACEMENT_3D('',#23954,#19588,#19589);
#17471=AXIS2_PLACEMENT_3D('',#23957,#19591,#19592);
#17472=AXIS2_PLACEMENT_3D('',#23958,#19593,#19594);
#17473=AXIS2_PLACEMENT_3D('',#23960,#19595,#19596);
#17474=AXIS2_PLACEMENT_3D('',#23963,#19598,#19599);
#17475=AXIS2_PLACEMENT_3D('',#23964,#19600,#19601);
#17476=AXIS2_PLACEMENT_3D('',#23966,#19602,#19603);
#17477=AXIS2_PLACEMENT_3D('',#23967,#19604,#19605);
#17478=AXIS2_PLACEMENT_3D('',#23969,#19606,#19607);
#17479=AXIS2_PLACEMENT_3D('',#23971,#19609,#19610);
#17480=AXIS2_PLACEMENT_3D('',#23973,#19611,#19612);
#17481=AXIS2_PLACEMENT_3D('',#23976,#19614,#19615);
#17482=AXIS2_PLACEMENT_3D('',#23977,#19616,#19617);
#17483=AXIS2_PLACEMENT_3D('',#23978,#19618,#19619);
#17484=AXIS2_PLACEMENT_3D('',#23979,#19620,#19621);
#17485=AXIS2_PLACEMENT_3D('',#23980,#19622,#19623);
#17486=AXIS2_PLACEMENT_3D('',#23981,#19624,#19625);
#17487=AXIS2_PLACEMENT_3D('',#23984,#19626,#19627);
#17488=AXIS2_PLACEMENT_3D('',#23985,#19628,#19629);
#17489=AXIS2_PLACEMENT_3D('',#23987,#19630,#19631);
#17490=AXIS2_PLACEMENT_3D('',#23989,#19632,#19633);
#17491=AXIS2_PLACEMENT_3D('',#23990,#19634,#19635);
#17492=AXIS2_PLACEMENT_3D('',#23991,#19636,#19637);
#17493=AXIS2_PLACEMENT_3D('',#23994,#19639,#19640);
#17494=AXIS2_PLACEMENT_3D('',#23995,#19641,#19642);
#17495=AXIS2_PLACEMENT_3D('',#23997,#19643,#19644);
#17496=AXIS2_PLACEMENT_3D('',#24000,#19646,#19647);
#17497=AXIS2_PLACEMENT_3D('',#24001,#19648,#19649);
#17498=AXIS2_PLACEMENT_3D('',#24004,#19651,#19652);
#17499=AXIS2_PLACEMENT_3D('',#24005,#19653,#19654);
#17500=AXIS2_PLACEMENT_3D('',#24006,#19655,#19656);
#17501=AXIS2_PLACEMENT_3D('',#24008,#19657,#19658);
#17502=AXIS2_PLACEMENT_3D('',#24010,#19660,#19661);
#17503=AXIS2_PLACEMENT_3D('',#24012,#19662,#19663);
#17504=AXIS2_PLACEMENT_3D('',#24013,#19664,#19665);
#17505=AXIS2_PLACEMENT_3D('',#24015,#19667,#19668);
#17506=AXIS2_PLACEMENT_3D('',#24016,#19669,#19670);
#17507=AXIS2_PLACEMENT_3D('',#24019,#19671,#19672);
#17508=AXIS2_PLACEMENT_3D('',#24020,#19673,#19674);
#17509=AXIS2_PLACEMENT_3D('',#24022,#19675,#19676);
#17510=AXIS2_PLACEMENT_3D('',#24024,#19677,#19678);
#17511=AXIS2_PLACEMENT_3D('',#24025,#19679,#19680);
#17512=AXIS2_PLACEMENT_3D('',#24026,#19681,#19682);
#17513=AXIS2_PLACEMENT_3D('',#24028,#19683,#19684);
#17514=AXIS2_PLACEMENT_3D('',#24030,#19686,#19687);
#17515=AXIS2_PLACEMENT_3D('',#24032,#19688,#19689);
#17516=AXIS2_PLACEMENT_3D('',#24034,#19690,#19691);
#17517=AXIS2_PLACEMENT_3D('',#24035,#19692,#19693);
#17518=AXIS2_PLACEMENT_3D('',#24037,#19694,#19695);
#17519=AXIS2_PLACEMENT_3D('',#24039,#19697,#19698);
#17520=AXIS2_PLACEMENT_3D('',#24041,#19699,#19700);
#17521=AXIS2_PLACEMENT_3D('',#24043,#19702,#19703);
#17522=AXIS2_PLACEMENT_3D('',#24045,#19704,#19705);
#17523=AXIS2_PLACEMENT_3D('',#24047,#19707,#19708);
#17524=AXIS2_PLACEMENT_3D('',#24048,#19709,#19710);
#17525=AXIS2_PLACEMENT_3D('',#24050,#19712,#19713);
#17526=AXIS2_PLACEMENT_3D('',#24051,#19714,#19715);
#17527=AXIS2_PLACEMENT_3D('',#24054,#19716,#19717);
#17528=AXIS2_PLACEMENT_3D('',#24055,#19718,#19719);
#17529=AXIS2_PLACEMENT_3D('',#24058,#19720,#19721);
#17530=AXIS2_PLACEMENT_3D('',#24059,#19722,#19723);
#17531=AXIS2_PLACEMENT_3D('',#24062,#19724,#19725);
#17532=AXIS2_PLACEMENT_3D('',#24063,#19726,#19727);
#17533=AXIS2_PLACEMENT_3D('',#24066,#19728,#19729);
#17534=AXIS2_PLACEMENT_3D('',#24067,#19730,#19731);
#17535=AXIS2_PLACEMENT_3D('',#24070,#19732,#19733);
#17536=AXIS2_PLACEMENT_3D('',#24071,#19734,#19735);
#17537=AXIS2_PLACEMENT_3D('',#24074,#19736,#19737);
#17538=AXIS2_PLACEMENT_3D('',#24075,#19738,#19739);
#17539=AXIS2_PLACEMENT_3D('',#24078,#19740,#19741);
#17540=AXIS2_PLACEMENT_3D('',#24079,#19742,#19743);
#17541=AXIS2_PLACEMENT_3D('',#24080,#19744,#19745);
#17542=AXIS2_PLACEMENT_3D('',#24106,#19746,#19747);
#17543=AXIS2_PLACEMENT_3D('',#24130,#19748,#19749);
#17544=AXIS2_PLACEMENT_3D('',#24131,#19750,#19751);
#17545=AXIS2_PLACEMENT_3D('',#24133,#19752,#19753);
#17546=AXIS2_PLACEMENT_3D('',#24158,#19754,#19755);
#17547=AXIS2_PLACEMENT_3D('',#24183,#19756,#19757);
#17548=AXIS2_PLACEMENT_3D('',#24186,#19759,#19760);
#17549=AXIS2_PLACEMENT_3D('',#24188,#19761,#19762);
#17550=AXIS2_PLACEMENT_3D('',#24213,#19763,#19764);
#17551=AXIS2_PLACEMENT_3D('',#24238,#19765,#19766);
#17552=AXIS2_PLACEMENT_3D('',#24263,#19767,#19768);
#17553=AXIS2_PLACEMENT_3D('',#24287,#19769,#19770);
#17554=AXIS2_PLACEMENT_3D('',#24288,#19771,#19772);
#17555=AXIS2_PLACEMENT_3D('',#24290,#19773,#19774);
#17556=AXIS2_PLACEMENT_3D('',#24291,#19775,#19776);
#17557=AXIS2_PLACEMENT_3D('',#24292,#19777,#19778);
#17558=AXIS2_PLACEMENT_3D('',#24316,#19779,#19780);
#17559=AXIS2_PLACEMENT_3D('',#24317,#19781,#19782);
#17560=AXIS2_PLACEMENT_3D('',#24319,#19783,#19784);
#17561=AXIS2_PLACEMENT_3D('',#24320,#19785,#19786);
#17562=AXIS2_PLACEMENT_3D('',#24321,#19787,#19788);
#17563=AXIS2_PLACEMENT_3D('',#24345,#19789,#19790);
#17564=AXIS2_PLACEMENT_3D('',#24346,#19791,#19792);
#17565=AXIS2_PLACEMENT_3D('',#24348,#19793,#19794);
#17566=AXIS2_PLACEMENT_3D('',#24350,#19795,#19796);
#17567=AXIS2_PLACEMENT_3D('',#24351,#19797,#19798);
#17568=AXIS2_PLACEMENT_3D('',#24352,#19799,#19800);
#17569=AXIS2_PLACEMENT_3D('',#24376,#19801,#19802);
#17570=AXIS2_PLACEMENT_3D('',#24377,#19803,#19804);
#17571=AXIS2_PLACEMENT_3D('',#24379,#19805,#19806);
#17572=AXIS2_PLACEMENT_3D('',#24380,#19807,#19808);
#17573=AXIS2_PLACEMENT_3D('',#24381,#19809,#19810);
#17574=AXIS2_PLACEMENT_3D('',#24405,#19811,#19812);
#17575=AXIS2_PLACEMENT_3D('',#24406,#19813,#19814);
#17576=AXIS2_PLACEMENT_3D('',#24408,#19815,#19816);
#17577=AXIS2_PLACEMENT_3D('',#24409,#19817,#19818);
#17578=AXIS2_PLACEMENT_3D('',#24410,#19819,#19820);
#17579=AXIS2_PLACEMENT_3D('',#24434,#19821,#19822);
#17580=AXIS2_PLACEMENT_3D('',#24435,#19823,#19824);
#17581=AXIS2_PLACEMENT_3D('',#24437,#19825,#19826);
#17582=AXIS2_PLACEMENT_3D('',#24440,#19828,#19829);
#17583=AXIS2_PLACEMENT_3D('',#24464,#19830,#19831);
#17584=AXIS2_PLACEMENT_3D('',#24465,#19832,#19833);
#17585=AXIS2_PLACEMENT_3D('',#24466,#19834,#19835);
#17586=AXIS2_PLACEMENT_3D('',#24467,#19836,#19837);
#17587=AXIS2_PLACEMENT_3D('',#24468,#19838,#19839);
#17588=AXIS2_PLACEMENT_3D('',#24469,#19840,#19841);
#17589=AXIS2_PLACEMENT_3D('',#24470,#19842,#19843);
#17590=AXIS2_PLACEMENT_3D('',#24471,#19844,#19845);
#17591=AXIS2_PLACEMENT_3D('',#24472,#19846,#19847);
#17592=AXIS2_PLACEMENT_3D('',#24474,#19848,#19849);
#17593=AXIS2_PLACEMENT_3D('',#24476,#19850,#19851);
#17594=AXIS2_PLACEMENT_3D('',#24477,#19852,#19853);
#17595=AXIS2_PLACEMENT_3D('',#24479,#19854,#19855);
#17596=AXIS2_PLACEMENT_3D('',#24481,#19857,#19858);
#17597=AXIS2_PLACEMENT_3D('',#24483,#19859,#19860);
#17598=AXIS2_PLACEMENT_3D('',#24484,#19861,#19862);
#17599=AXIS2_PLACEMENT_3D('',#24486,#19864,#19865);
#17600=AXIS2_PLACEMENT_3D('',#24488,#19866,#19867);
#17601=AXIS2_PLACEMENT_3D('',#24490,#19868,#19869);
#17602=AXIS2_PLACEMENT_3D('',#24491,#19870,#19871);
#17603=AXIS2_PLACEMENT_3D('',#24493,#19872,#19873);
#17604=AXIS2_PLACEMENT_3D('',#24495,#19875,#19876);
#17605=AXIS2_PLACEMENT_3D('',#24497,#19877,#19878);
#17606=AXIS2_PLACEMENT_3D('',#24498,#19879,#19880);
#17607=AXIS2_PLACEMENT_3D('',#24500,#19882,#19883);
#17608=AXIS2_PLACEMENT_3D('',#24501,#19884,#19885);
#17609=AXIS2_PLACEMENT_3D('',#24502,#19886,#19887);
#17610=AXIS2_PLACEMENT_3D('',#24503,#19888,#19889);
#17611=AXIS2_PLACEMENT_3D('',#24504,#19890,#19891);
#17612=AXIS2_PLACEMENT_3D('',#24505,#19892,#19893);
#17613=AXIS2_PLACEMENT_3D('',#24506,#19894,#19895);
#17614=AXIS2_PLACEMENT_3D('',#24507,#19896,#19897);
#17615=AXIS2_PLACEMENT_3D('',#24510,#19898,#19899);
#17616=AXIS2_PLACEMENT_3D('',#24511,#19900,#19901);
#17617=AXIS2_PLACEMENT_3D('',#24513,#19902,#19903);
#17618=AXIS2_PLACEMENT_3D('',#24515,#19904,#19905);
#17619=AXIS2_PLACEMENT_3D('',#24516,#19906,#19907);
#17620=AXIS2_PLACEMENT_3D('',#24517,#19908,#19909);
#17621=AXIS2_PLACEMENT_3D('',#24520,#19911,#19912);
#17622=AXIS2_PLACEMENT_3D('',#24521,#19913,#19914);
#17623=AXIS2_PLACEMENT_3D('',#24523,#19915,#19916);
#17624=AXIS2_PLACEMENT_3D('',#24526,#19918,#19919);
#17625=AXIS2_PLACEMENT_3D('',#24527,#19920,#19921);
#17626=AXIS2_PLACEMENT_3D('',#24530,#19923,#19924);
#17627=AXIS2_PLACEMENT_3D('',#24531,#19925,#19926);
#17628=AXIS2_PLACEMENT_3D('',#24532,#19927,#19928);
#17629=AXIS2_PLACEMENT_3D('',#24534,#19929,#19930);
#17630=AXIS2_PLACEMENT_3D('',#24536,#19932,#19933);
#17631=AXIS2_PLACEMENT_3D('',#24538,#19934,#19935);
#17632=AXIS2_PLACEMENT_3D('',#24539,#19936,#19937);
#17633=AXIS2_PLACEMENT_3D('',#24541,#19939,#19940);
#17634=AXIS2_PLACEMENT_3D('',#24542,#19941,#19942);
#17635=AXIS2_PLACEMENT_3D('',#24545,#19943,#19944);
#17636=AXIS2_PLACEMENT_3D('',#24546,#19945,#19946);
#17637=AXIS2_PLACEMENT_3D('',#24548,#19947,#19948);
#17638=AXIS2_PLACEMENT_3D('',#24550,#19949,#19950);
#17639=AXIS2_PLACEMENT_3D('',#24551,#19951,#19952);
#17640=AXIS2_PLACEMENT_3D('',#24552,#19953,#19954);
#17641=AXIS2_PLACEMENT_3D('',#24554,#19955,#19956);
#17642=AXIS2_PLACEMENT_3D('',#24556,#19958,#19959);
#17643=AXIS2_PLACEMENT_3D('',#24558,#19960,#19961);
#17644=AXIS2_PLACEMENT_3D('',#24560,#19962,#19963);
#17645=AXIS2_PLACEMENT_3D('',#24561,#19964,#19965);
#17646=AXIS2_PLACEMENT_3D('',#24563,#19966,#19967);
#17647=AXIS2_PLACEMENT_3D('',#24565,#19969,#19970);
#17648=AXIS2_PLACEMENT_3D('',#24567,#19971,#19972);
#17649=AXIS2_PLACEMENT_3D('',#24569,#19974,#19975);
#17650=AXIS2_PLACEMENT_3D('',#24571,#19976,#19977);
#17651=AXIS2_PLACEMENT_3D('',#24573,#19979,#19980);
#17652=AXIS2_PLACEMENT_3D('',#24574,#19981,#19982);
#17653=AXIS2_PLACEMENT_3D('',#24576,#19984,#19985);
#17654=AXIS2_PLACEMENT_3D('',#24577,#19986,#19987);
#17655=AXIS2_PLACEMENT_3D('',#24580,#19988,#19989);
#17656=AXIS2_PLACEMENT_3D('',#24581,#19990,#19991);
#17657=AXIS2_PLACEMENT_3D('',#24584,#19992,#19993);
#17658=AXIS2_PLACEMENT_3D('',#24585,#19994,#19995);
#17659=AXIS2_PLACEMENT_3D('',#24588,#19996,#19997);
#17660=AXIS2_PLACEMENT_3D('',#24589,#19998,#19999);
#17661=AXIS2_PLACEMENT_3D('',#24592,#20000,#20001);
#17662=AXIS2_PLACEMENT_3D('',#24593,#20002,#20003);
#17663=AXIS2_PLACEMENT_3D('',#24596,#20004,#20005);
#17664=AXIS2_PLACEMENT_3D('',#24597,#20006,#20007);
#17665=AXIS2_PLACEMENT_3D('',#24600,#20008,#20009);
#17666=AXIS2_PLACEMENT_3D('',#24601,#20010,#20011);
#17667=AXIS2_PLACEMENT_3D('',#24604,#20012,#20013);
#17668=AXIS2_PLACEMENT_3D('',#24605,#20014,#20015);
#17669=AXIS2_PLACEMENT_3D('',#24608,#20016,#20017);
#17670=AXIS2_PLACEMENT_3D('',#24609,#20018,#20019);
#17671=AXIS2_PLACEMENT_3D('',#24610,#20020,#20021);
#17672=AXIS2_PLACEMENT_3D('',#24636,#20022,#20023);
#17673=AXIS2_PLACEMENT_3D('',#24660,#20024,#20025);
#17674=AXIS2_PLACEMENT_3D('',#24661,#20026,#20027);
#17675=AXIS2_PLACEMENT_3D('',#24663,#20028,#20029);
#17676=AXIS2_PLACEMENT_3D('',#24688,#20030,#20031);
#17677=AXIS2_PLACEMENT_3D('',#24713,#20032,#20033);
#17678=AXIS2_PLACEMENT_3D('',#24729,#20035,#20036);
#17679=AXIS2_PLACEMENT_3D('',#24744,#20037,#20038);
#17680=AXIS2_PLACEMENT_3D('',#24769,#20039,#20040);
#17681=AXIS2_PLACEMENT_3D('',#24794,#20041,#20042);
#17682=AXIS2_PLACEMENT_3D('',#24819,#20043,#20044);
#17683=AXIS2_PLACEMENT_3D('',#24843,#20045,#20046);
#17684=AXIS2_PLACEMENT_3D('',#24844,#20047,#20048);
#17685=AXIS2_PLACEMENT_3D('',#24846,#20049,#20050);
#17686=AXIS2_PLACEMENT_3D('',#24847,#20051,#20052);
#17687=AXIS2_PLACEMENT_3D('',#24848,#20053,#20054);
#17688=AXIS2_PLACEMENT_3D('',#24872,#20055,#20056);
#17689=AXIS2_PLACEMENT_3D('',#24873,#20057,#20058);
#17690=AXIS2_PLACEMENT_3D('',#24875,#20059,#20060);
#17691=AXIS2_PLACEMENT_3D('',#24876,#20061,#20062);
#17692=AXIS2_PLACEMENT_3D('',#24877,#20063,#20064);
#17693=AXIS2_PLACEMENT_3D('',#24901,#20065,#20066);
#17694=AXIS2_PLACEMENT_3D('',#24902,#20067,#20068);
#17695=AXIS2_PLACEMENT_3D('',#24904,#20069,#20070);
#17696=AXIS2_PLACEMENT_3D('',#24905,#20071,#20072);
#17697=AXIS2_PLACEMENT_3D('',#24906,#20073,#20074);
#17698=AXIS2_PLACEMENT_3D('',#24921,#20075,#20076);
#17699=AXIS2_PLACEMENT_3D('',#24934,#20077,#20078);
#17700=AXIS2_PLACEMENT_3D('',#24936,#20079,#20080);
#17701=AXIS2_PLACEMENT_3D('',#24937,#20081,#20082);
#17702=AXIS2_PLACEMENT_3D('',#24938,#20083,#20084);
#17703=AXIS2_PLACEMENT_3D('',#24962,#20085,#20086);
#17704=AXIS2_PLACEMENT_3D('',#24963,#20087,#20088);
#17705=AXIS2_PLACEMENT_3D('',#24965,#20089,#20090);
#17706=AXIS2_PLACEMENT_3D('',#24966,#20091,#20092);
#17707=AXIS2_PLACEMENT_3D('',#24967,#20093,#20094);
#17708=AXIS2_PLACEMENT_3D('',#24991,#20095,#20096);
#17709=AXIS2_PLACEMENT_3D('',#24992,#20097,#20098);
#17710=AXIS2_PLACEMENT_3D('',#24994,#20099,#20100);
#17711=AXIS2_PLACEMENT_3D('',#24995,#20101,#20102);
#17712=AXIS2_PLACEMENT_3D('',#24996,#20103,#20104);
#17713=AXIS2_PLACEMENT_3D('',#25020,#20105,#20106);
#17714=AXIS2_PLACEMENT_3D('',#25021,#20107,#20108);
#17715=AXIS2_PLACEMENT_3D('',#25023,#20109,#20110);
#17716=AXIS2_PLACEMENT_3D('',#25026,#20112,#20113);
#17717=AXIS2_PLACEMENT_3D('',#25050,#20114,#20115);
#17718=AXIS2_PLACEMENT_3D('',#25051,#20116,#20117);
#17719=AXIS2_PLACEMENT_3D('',#25052,#20118,#20119);
#17720=AXIS2_PLACEMENT_3D('',#25053,#20120,#20121);
#17721=AXIS2_PLACEMENT_3D('',#25054,#20122,#20123);
#17722=AXIS2_PLACEMENT_3D('',#25055,#20124,#20125);
#17723=AXIS2_PLACEMENT_3D('',#25056,#20126,#20127);
#17724=AXIS2_PLACEMENT_3D('',#25057,#20128,#20129);
#17725=AXIS2_PLACEMENT_3D('',#25058,#20130,#20131);
#17726=AXIS2_PLACEMENT_3D('',#25060,#20132,#20133);
#17727=AXIS2_PLACEMENT_3D('',#25062,#20134,#20135);
#17728=AXIS2_PLACEMENT_3D('',#25063,#20136,#20137);
#17729=AXIS2_PLACEMENT_3D('',#25065,#20138,#20139);
#17730=AXIS2_PLACEMENT_3D('',#25067,#20141,#20142);
#17731=AXIS2_PLACEMENT_3D('',#25069,#20143,#20144);
#17732=AXIS2_PLACEMENT_3D('',#25070,#20145,#20146);
#17733=AXIS2_PLACEMENT_3D('',#25072,#20148,#20149);
#17734=AXIS2_PLACEMENT_3D('',#25074,#20150,#20151);
#17735=AXIS2_PLACEMENT_3D('',#25076,#20152,#20153);
#17736=AXIS2_PLACEMENT_3D('',#25077,#20154,#20155);
#17737=AXIS2_PLACEMENT_3D('',#25079,#20156,#20157);
#17738=AXIS2_PLACEMENT_3D('',#25081,#20159,#20160);
#17739=AXIS2_PLACEMENT_3D('',#25083,#20161,#20162);
#17740=AXIS2_PLACEMENT_3D('',#25084,#20163,#20164);
#17741=AXIS2_PLACEMENT_3D('',#25086,#20166,#20167);
#17742=AXIS2_PLACEMENT_3D('',#25087,#20168,#20169);
#17743=AXIS2_PLACEMENT_3D('',#25088,#20170,#20171);
#17744=AXIS2_PLACEMENT_3D('',#25089,#20172,#20173);
#17745=AXIS2_PLACEMENT_3D('',#25090,#20174,#20175);
#17746=AXIS2_PLACEMENT_3D('',#25091,#20176,#20177);
#17747=AXIS2_PLACEMENT_3D('',#25092,#20178,#20179);
#17748=AXIS2_PLACEMENT_3D('',#25101,#20184,#20185);
#17749=AXIS2_PLACEMENT_3D('',#25107,#20189,#20190);
#17750=AXIS2_PLACEMENT_3D('',#25113,#20194,#20195);
#17751=AXIS2_PLACEMENT_3D('',#25119,#20199,#20200);
#17752=AXIS2_PLACEMENT_3D('',#25125,#20204,#20205);
#17753=AXIS2_PLACEMENT_3D('',#25128,#20208,#20209);
#17754=AXIS2_PLACEMENT_3D('',#25129,#20210,#20211);
#17755=AXIS2_PLACEMENT_3D('',#25130,#20212,#20213);
#17756=AXIS2_PLACEMENT_3D('',#25132,#20214,#20215);
#17757=AXIS2_PLACEMENT_3D('',#25133,#20216,#20217);
#17758=AXIS2_PLACEMENT_3D('',#25135,#20218,#20219);
#17759=AXIS2_PLACEMENT_3D('',#25136,#20220,#20221);
#17760=AXIS2_PLACEMENT_3D('',#25138,#20222,#20223);
#17761=AXIS2_PLACEMENT_3D('',#25140,#20225,#20226);
#17762=AXIS2_PLACEMENT_3D('',#25142,#20227,#20228);
#17763=AXIS2_PLACEMENT_3D('',#25144,#20230,#20231);
#17764=AXIS2_PLACEMENT_3D('',#25146,#20232,#20233);
#17765=AXIS2_PLACEMENT_3D('',#25148,#20235,#20236);
#17766=AXIS2_PLACEMENT_3D('',#25150,#20237,#20238);
#17767=AXIS2_PLACEMENT_3D('',#25151,#20239,#20240);
#17768=AXIS2_PLACEMENT_3D('',#25153,#20241,#20242);
#17769=AXIS2_PLACEMENT_3D('',#25155,#20244,#20245);
#17770=AXIS2_PLACEMENT_3D('',#25157,#20247,#20248);
#17771=AXIS2_PLACEMENT_3D('',#25158,#20249,#20250);
#17772=AXIS2_PLACEMENT_3D('',#25167,#20255,#20256);
#17773=AXIS2_PLACEMENT_3D('',#25173,#20260,#20261);
#17774=AXIS2_PLACEMENT_3D('',#25179,#20265,#20266);
#17775=AXIS2_PLACEMENT_3D('',#25182,#20269,#20270);
#17776=AXIS2_PLACEMENT_3D('',#25183,#20271,#20272);
#17777=AXIS2_PLACEMENT_3D('',#25192,#20277,#20278);
#17778=AXIS2_PLACEMENT_3D('',#25198,#20282,#20283);
#17779=AXIS2_PLACEMENT_3D('',#25204,#20287,#20288);
#17780=AXIS2_PLACEMENT_3D('',#25207,#20291,#20292);
#17781=AXIS2_PLACEMENT_3D('',#25208,#20293,#20294);
#17782=AXIS2_PLACEMENT_3D('',#25217,#20299,#20300);
#17783=AXIS2_PLACEMENT_3D('',#25223,#20304,#20305);
#17784=AXIS2_PLACEMENT_3D('',#25229,#20309,#20310);
#17785=AXIS2_PLACEMENT_3D('',#25232,#20313,#20314);
#17786=AXIS2_PLACEMENT_3D('',#25233,#20315,#20316);
#17787=AXIS2_PLACEMENT_3D('',#25242,#20321,#20322);
#17788=AXIS2_PLACEMENT_3D('',#25248,#20326,#20327);
#17789=AXIS2_PLACEMENT_3D('',#25254,#20331,#20332);
#17790=AXIS2_PLACEMENT_3D('',#25257,#20335,#20336);
#17791=AXIS2_PLACEMENT_3D('',#25258,#20337,#20338);
#17792=AXIS2_PLACEMENT_3D('',#25267,#20343,#20344);
#17793=AXIS2_PLACEMENT_3D('',#25273,#20348,#20349);
#17794=AXIS2_PLACEMENT_3D('',#25279,#20353,#20354);
#17795=AXIS2_PLACEMENT_3D('',#25282,#20357,#20358);
#17796=AXIS2_PLACEMENT_3D('',#25283,#20359,#20360);
#17797=AXIS2_PLACEMENT_3D('',#25292,#20365,#20366);
#17798=AXIS2_PLACEMENT_3D('',#25298,#20370,#20371);
#17799=AXIS2_PLACEMENT_3D('',#25304,#20375,#20376);
#17800=AXIS2_PLACEMENT_3D('',#25307,#20379,#20380);
#17801=AXIS2_PLACEMENT_3D('',#25308,#20381,#20382);
#17802=AXIS2_PLACEMENT_3D('',#25317,#20387,#20388);
#17803=AXIS2_PLACEMENT_3D('',#25323,#20392,#20393);
#17804=AXIS2_PLACEMENT_3D('',#25329,#20397,#20398);
#17805=AXIS2_PLACEMENT_3D('',#25332,#20401,#20402);
#17806=AXIS2_PLACEMENT_3D('',#25333,#20403,#20404);
#17807=AXIS2_PLACEMENT_3D('',#25342,#20409,#20410);
#17808=AXIS2_PLACEMENT_3D('',#25348,#20414,#20415);
#17809=AXIS2_PLACEMENT_3D('',#25354,#20419,#20420);
#17810=AXIS2_PLACEMENT_3D('',#25357,#20423,#20424);
#17811=AXIS2_PLACEMENT_3D('',#25358,#20425,#20426);
#17812=AXIS2_PLACEMENT_3D('',#25367,#20431,#20432);
#17813=AXIS2_PLACEMENT_3D('',#25373,#20436,#20437);
#17814=AXIS2_PLACEMENT_3D('',#25379,#20441,#20442);
#17815=AXIS2_PLACEMENT_3D('',#25382,#20445,#20446);
#17816=AXIS2_PLACEMENT_3D('',#25383,#20447,#20448);
#17817=AXIS2_PLACEMENT_3D('',#25392,#20453,#20454);
#17818=AXIS2_PLACEMENT_3D('',#25398,#20458,#20459);
#17819=AXIS2_PLACEMENT_3D('',#25404,#20463,#20464);
#17820=AXIS2_PLACEMENT_3D('',#25407,#20467,#20468);
#17821=AXIS2_PLACEMENT_3D('',#25408,#20469,#20470);
#17822=AXIS2_PLACEMENT_3D('',#25417,#20475,#20476);
#17823=AXIS2_PLACEMENT_3D('',#25423,#20480,#20481);
#17824=AXIS2_PLACEMENT_3D('',#25429,#20485,#20486);
#17825=AXIS2_PLACEMENT_3D('',#25432,#20489,#20490);
#17826=AXIS2_PLACEMENT_3D('',#25433,#20491,#20492);
#17827=AXIS2_PLACEMENT_3D('',#25442,#20497,#20498);
#17828=AXIS2_PLACEMENT_3D('',#25448,#20502,#20503);
#17829=AXIS2_PLACEMENT_3D('',#25454,#20507,#20508);
#17830=AXIS2_PLACEMENT_3D('',#25457,#20511,#20512);
#17831=AXIS2_PLACEMENT_3D('',#25458,#20513,#20514);
#17832=AXIS2_PLACEMENT_3D('',#25467,#20519,#20520);
#17833=AXIS2_PLACEMENT_3D('',#25473,#20524,#20525);
#17834=AXIS2_PLACEMENT_3D('',#25479,#20529,#20530);
#17835=AXIS2_PLACEMENT_3D('',#25482,#20533,#20534);
#17836=AXIS2_PLACEMENT_3D('',#25483,#20535,#20536);
#17837=AXIS2_PLACEMENT_3D('',#25492,#20541,#20542);
#17838=AXIS2_PLACEMENT_3D('',#25498,#20546,#20547);
#17839=AXIS2_PLACEMENT_3D('',#25504,#20551,#20552);
#17840=AXIS2_PLACEMENT_3D('',#25507,#20555,#20556);
#17841=AXIS2_PLACEMENT_3D('',#25508,#20557,#20558);
#17842=AXIS2_PLACEMENT_3D('',#25517,#20563,#20564);
#17843=AXIS2_PLACEMENT_3D('',#25523,#20568,#20569);
#17844=AXIS2_PLACEMENT_3D('',#25529,#20573,#20574);
#17845=AXIS2_PLACEMENT_3D('',#25532,#20577,#20578);
#17846=AXIS2_PLACEMENT_3D('',#25533,#20579,#20580);
#17847=AXIS2_PLACEMENT_3D('',#25542,#20585,#20586);
#17848=AXIS2_PLACEMENT_3D('',#25548,#20590,#20591);
#17849=AXIS2_PLACEMENT_3D('',#25554,#20595,#20596);
#17850=AXIS2_PLACEMENT_3D('',#25557,#20599,#20600);
#17851=AXIS2_PLACEMENT_3D('',#25558,#20601,#20602);
#17852=AXIS2_PLACEMENT_3D('',#25567,#20607,#20608);
#17853=AXIS2_PLACEMENT_3D('',#25573,#20612,#20613);
#17854=AXIS2_PLACEMENT_3D('',#25579,#20617,#20618);
#17855=AXIS2_PLACEMENT_3D('',#25582,#20621,#20622);
#17856=AXIS2_PLACEMENT_3D('',#25583,#20623,#20624);
#17857=AXIS2_PLACEMENT_3D('',#25592,#20629,#20630);
#17858=AXIS2_PLACEMENT_3D('',#25598,#20634,#20635);
#17859=AXIS2_PLACEMENT_3D('',#25604,#20639,#20640);
#17860=AXIS2_PLACEMENT_3D('',#25607,#20643,#20644);
#17861=AXIS2_PLACEMENT_3D('',#25608,#20645,#20646);
#17862=AXIS2_PLACEMENT_3D('',#25617,#20651,#20652);
#17863=AXIS2_PLACEMENT_3D('',#25623,#20656,#20657);
#17864=AXIS2_PLACEMENT_3D('',#25629,#20661,#20662);
#17865=AXIS2_PLACEMENT_3D('',#25632,#20665,#20666);
#17866=AXIS2_PLACEMENT_3D('',#25633,#20667,#20668);
#17867=AXIS2_PLACEMENT_3D('',#25642,#20673,#20674);
#17868=AXIS2_PLACEMENT_3D('',#25648,#20678,#20679);
#17869=AXIS2_PLACEMENT_3D('',#25654,#20683,#20684);
#17870=AXIS2_PLACEMENT_3D('',#25657,#20687,#20688);
#17871=AXIS2_PLACEMENT_3D('',#25658,#20689,#20690);
#17872=AXIS2_PLACEMENT_3D('',#25667,#20695,#20696);
#17873=AXIS2_PLACEMENT_3D('',#25673,#20700,#20701);
#17874=AXIS2_PLACEMENT_3D('',#25679,#20705,#20706);
#17875=AXIS2_PLACEMENT_3D('',#25682,#20709,#20710);
#17876=AXIS2_PLACEMENT_3D('',#25683,#20711,#20712);
#17877=AXIS2_PLACEMENT_3D('',#25692,#20717,#20718);
#17878=AXIS2_PLACEMENT_3D('',#25698,#20722,#20723);
#17879=AXIS2_PLACEMENT_3D('',#25704,#20727,#20728);
#17880=AXIS2_PLACEMENT_3D('',#25707,#20731,#20732);
#17881=AXIS2_PLACEMENT_3D('',#25708,#20733,#20734);
#17882=AXIS2_PLACEMENT_3D('',#25717,#20739,#20740);
#17883=AXIS2_PLACEMENT_3D('',#25723,#20744,#20745);
#17884=AXIS2_PLACEMENT_3D('',#25729,#20749,#20750);
#17885=AXIS2_PLACEMENT_3D('',#25732,#20753,#20754);
#17886=AXIS2_PLACEMENT_3D('',#25733,#20755,#20756);
#17887=AXIS2_PLACEMENT_3D('',#25742,#20761,#20762);
#17888=AXIS2_PLACEMENT_3D('',#25748,#20766,#20767);
#17889=AXIS2_PLACEMENT_3D('',#25754,#20771,#20772);
#17890=AXIS2_PLACEMENT_3D('',#25757,#20775,#20776);
#17891=AXIS2_PLACEMENT_3D('',#25758,#20777,#20778);
#17892=AXIS2_PLACEMENT_3D('',#25760,#20779,#20780);
#17893=AXIS2_PLACEMENT_3D('',#25763,#20782,#20783);
#17894=AXIS2_PLACEMENT_3D('',#25764,#20784,#20785);
#17895=AXIS2_PLACEMENT_3D('',#25766,#20786,#20787);
#17896=AXIS2_PLACEMENT_3D('',#25769,#20789,#20790);
#17897=AXIS2_PLACEMENT_3D('',#25770,#20791,#20792);
#17898=AXIS2_PLACEMENT_3D('',#25772,#20793,#20794);
#17899=AXIS2_PLACEMENT_3D('',#25775,#20796,#20797);
#17900=AXIS2_PLACEMENT_3D('',#25776,#20798,#20799);
#17901=AXIS2_PLACEMENT_3D('',#25785,#20804,#20805);
#17902=AXIS2_PLACEMENT_3D('',#25794,#20810,#20811);
#17903=AXIS2_PLACEMENT_3D('',#25800,#20815,#20816);
#17904=AXIS2_PLACEMENT_3D('',#25806,#20820,#20821);
#17905=AXIS2_PLACEMENT_3D('',#25809,#20824,#20825);
#17906=AXIS2_PLACEMENT_3D('',#25815,#20829,#20830);
#17907=AXIS2_PLACEMENT_3D('',#25818,#20832,#20833);
#17908=AXIS2_PLACEMENT_3D('',#25819,#20834,#20835);
#17909=AXIS2_PLACEMENT_3D('',#25823,#20838,#20839);
#17910=AXIS2_PLACEMENT_3D('',#25824,#20840,#20841);
#17911=AXIS2_PLACEMENT_3D('',#25825,#20842,#20843);
#17912=AXIS2_PLACEMENT_3D('',#25826,#20844,#20845);
#17913=AXIS2_PLACEMENT_3D('',#25827,#20846,#20847);
#17914=AXIS2_PLACEMENT_3D('',#25829,#20848,#20849);
#17915=AXIS2_PLACEMENT_3D('',#25832,#20851,#20852);
#17916=AXIS2_PLACEMENT_3D('',#25833,#20853,#20854);
#17917=AXIS2_PLACEMENT_3D('',#25835,#20855,#20856);
#17918=AXIS2_PLACEMENT_3D('',#25838,#20858,#20859);
#17919=AXIS2_PLACEMENT_3D('',#25839,#20860,#20861);
#17920=AXIS2_PLACEMENT_3D('',#25840,#20862,#20863);
#17921=AXIS2_PLACEMENT_3D('',#25841,#20864,#20865);
#17922=AXIS2_PLACEMENT_3D('',#25842,#20866,#20867);
#17923=AXIS2_PLACEMENT_3D('',#25844,#20868,#20869);
#17924=AXIS2_PLACEMENT_3D('',#25847,#20871,#20872);
#17925=AXIS2_PLACEMENT_3D('',#25848,#20873,#20874);
#17926=AXIS2_PLACEMENT_3D('',#25850,#20875,#20876);
#17927=AXIS2_PLACEMENT_3D('',#25853,#20878,#20879);
#17928=AXIS2_PLACEMENT_3D('',#25854,#20880,#20881);
#17929=AXIS2_PLACEMENT_3D('',#25855,#20882,#20883);
#17930=AXIS2_PLACEMENT_3D('',#25856,#20884,#20885);
#17931=AXIS2_PLACEMENT_3D('',#25857,#20886,#20887);
#17932=AXIS2_PLACEMENT_3D('',#25866,#20892,#20893);
#17933=AXIS2_PLACEMENT_3D('',#25872,#20897,#20898);
#17934=AXIS2_PLACEMENT_3D('',#25878,#20902,#20903);
#17935=AXIS2_PLACEMENT_3D('',#25881,#20906,#20907);
#17936=AXIS2_PLACEMENT_3D('',#25882,#20908,#20909);
#17937=AXIS2_PLACEMENT_3D('',#25883,#20910,#20911);
#17938=AXIS2_PLACEMENT_3D('',#25884,#20912,#20913);
#17939=AXIS2_PLACEMENT_3D('',#25893,#20918,#20919);
#17940=AXIS2_PLACEMENT_3D('',#25899,#20923,#20924);
#17941=AXIS2_PLACEMENT_3D('',#25905,#20928,#20929);
#17942=AXIS2_PLACEMENT_3D('',#25908,#20932,#20933);
#17943=AXIS2_PLACEMENT_3D('',#25909,#20934,#20935);
#17944=AXIS2_PLACEMENT_3D('',#25910,#20936,#20937);
#17945=AXIS2_PLACEMENT_3D('',#25911,#20938,#20939);
#17946=AXIS2_PLACEMENT_3D('',#25920,#20944,#20945);
#17947=AXIS2_PLACEMENT_3D('',#25926,#20949,#20950);
#17948=AXIS2_PLACEMENT_3D('',#25932,#20954,#20955);
#17949=AXIS2_PLACEMENT_3D('',#25938,#20959,#20960);
#17950=AXIS2_PLACEMENT_3D('',#25944,#20964,#20965);
#17951=AXIS2_PLACEMENT_3D('',#25947,#20968,#20969);
#17952=AXIS2_PLACEMENT_3D('',#25948,#20970,#20971);
#17953=AXIS2_PLACEMENT_3D('',#25949,#20972,#20973);
#17954=AXIS2_PLACEMENT_3D('',#25951,#20974,#20975);
#17955=AXIS2_PLACEMENT_3D('',#25953,#20976,#20977);
#17956=AXIS2_PLACEMENT_3D('',#25954,#20978,#20979);
#17957=AXIS2_PLACEMENT_3D('',#25957,#20981,#20982);
#17958=AXIS2_PLACEMENT_3D('',#25958,#20983,#20984);
#17959=AXIS2_PLACEMENT_3D('',#25959,#20985,#20986);
#17960=AXIS2_PLACEMENT_3D('',#25961,#20987,#20988);
#17961=AXIS2_PLACEMENT_3D('',#25962,#20989,#20990);
#17962=AXIS2_PLACEMENT_3D('',#25964,#20991,#20992);
#17963=AXIS2_PLACEMENT_3D('',#25966,#20994,#20995);
#17964=AXIS2_PLACEMENT_3D('',#25968,#20996,#20997);
#17965=AXIS2_PLACEMENT_3D('',#25970,#20999,#21000);
#17966=AXIS2_PLACEMENT_3D('',#25972,#21001,#21002);
#17967=AXIS2_PLACEMENT_3D('',#25974,#21004,#21005);
#17968=AXIS2_PLACEMENT_3D('',#25976,#21006,#21007);
#17969=AXIS2_PLACEMENT_3D('',#25977,#21008,#21009);
#17970=AXIS2_PLACEMENT_3D('',#25979,#21010,#21011);
#17971=AXIS2_PLACEMENT_3D('',#25981,#21013,#21014);
#17972=AXIS2_PLACEMENT_3D('',#25983,#21016,#21017);
#17973=AXIS2_PLACEMENT_3D('',#25984,#21018,#21019);
#17974=AXIS2_PLACEMENT_3D('',#25985,#21020,#21021);
#17975=AXIS2_PLACEMENT_3D('',#25987,#21022,#21023);
#17976=AXIS2_PLACEMENT_3D('',#25990,#21025,#21026);
#17977=AXIS2_PLACEMENT_3D('',#25991,#21027,#21028);
#17978=AXIS2_PLACEMENT_3D('',#25992,#21029,#21030);
#17979=AXIS2_PLACEMENT_3D('',#26001,#21035,#21036);
#17980=AXIS2_PLACEMENT_3D('',#26003,#21037,#21038);
#17981=AXIS2_PLACEMENT_3D('',#26007,#21041,#21042);
#17982=AXIS2_PLACEMENT_3D('',#26013,#21046,#21047);
#17983=AXIS2_PLACEMENT_3D('',#26015,#21049,#21050);
#17984=AXIS2_PLACEMENT_3D('',#26016,#21051,#21052);
#17985=AXIS2_PLACEMENT_3D('',#26017,#21053,#21054);
#17986=AXIS2_PLACEMENT_3D('',#26026,#21059,#21060);
#17987=AXIS2_PLACEMENT_3D('',#26028,#21061,#21062);
#17988=AXIS2_PLACEMENT_3D('',#26032,#21065,#21066);
#17989=AXIS2_PLACEMENT_3D('',#26038,#21070,#21071);
#17990=AXIS2_PLACEMENT_3D('',#26040,#21073,#21074);
#17991=AXIS2_PLACEMENT_3D('',#26041,#21075,#21076);
#17992=AXIS2_PLACEMENT_3D('',#26042,#21077,#21078);
#17993=AXIS2_PLACEMENT_3D('',#26044,#21079,#21080);
#17994=AXIS2_PLACEMENT_3D('',#26046,#21081,#21082);
#17995=AXIS2_PLACEMENT_3D('',#26047,#21083,#21084);
#17996=AXIS2_PLACEMENT_3D('',#26049,#21085,#21086);
#17997=AXIS2_PLACEMENT_3D('',#26051,#21087,#21088);
#17998=AXIS2_PLACEMENT_3D('',#26052,#21089,#21090);
#17999=AXIS2_PLACEMENT_3D('',#26054,#21092,#21093);
#18000=AXIS2_PLACEMENT_3D('',#26057,#21095,#21096);
#18001=AXIS2_PLACEMENT_3D('',#26058,#21097,#21098);
#18002=AXIS2_PLACEMENT_3D('',#26060,#21099,#21100);
#18003=AXIS2_PLACEMENT_3D('',#26062,#21102,#21103);
#18004=AXIS2_PLACEMENT_3D('',#26063,#21104,#21105);
#18005=AXIS2_PLACEMENT_3D('',#26064,#21106,#21107);
#18006=AXIS2_PLACEMENT_3D('',#26065,#21108,#21109);
#18007=AXIS2_PLACEMENT_3D('',#26067,#21110,#21111);
#18008=AXIS2_PLACEMENT_3D('',#26070,#21113,#21114);
#18009=AXIS2_PLACEMENT_3D('',#26071,#21115,#21116);
#18010=AXIS2_PLACEMENT_3D('',#26073,#21117,#21118);
#18011=AXIS2_PLACEMENT_3D('',#26076,#21120,#21121);
#18012=AXIS2_PLACEMENT_3D('',#26077,#21122,#21123);
#18013=AXIS2_PLACEMENT_3D('',#26078,#21124,#21125);
#18014=AXIS2_PLACEMENT_3D('',#26079,#21126,#21127);
#18015=AXIS2_PLACEMENT_3D('',#26080,#21128,#21129);
#18016=AXIS2_PLACEMENT_3D('',#26082,#21130,#21131);
#18017=AXIS2_PLACEMENT_3D('',#26085,#21133,#21134);
#18018=AXIS2_PLACEMENT_3D('',#26086,#21135,#21136);
#18019=AXIS2_PLACEMENT_3D('',#26088,#21137,#21138);
#18020=AXIS2_PLACEMENT_3D('',#26091,#21140,#21141);
#18021=AXIS2_PLACEMENT_3D('',#26092,#21142,#21143);
#18022=AXIS2_PLACEMENT_3D('',#26093,#21144,#21145);
#18023=AXIS2_PLACEMENT_3D('',#26094,#21146,#21147);
#18024=AXIS2_PLACEMENT_3D('',#26095,#21148,#21149);
#18025=AXIS2_PLACEMENT_3D('',#26099,#21151,#21152);
#18026=AXIS2_PLACEMENT_3D('',#26100,#21153,#21154);
#18027=AXIS2_PLACEMENT_3D('',#26113,#21155,#21156);
#18028=AXIS2_PLACEMENT_3D('',#26154,#21158,#21159);
#18029=AXIS2_PLACEMENT_3D('',#26165,#21160,#21161);
#18030=AXIS2_PLACEMENT_3D('',#26167,#21163,#21164);
#18031=AXIS2_PLACEMENT_3D('',#26169,#21165,#21166);
#18032=AXIS2_PLACEMENT_3D('',#26172,#21168,#21169);
#18033=AXIS2_PLACEMENT_3D('',#26173,#21170,#21171);
#18034=AXIS2_PLACEMENT_3D('',#26175,#21172,#21173);
#18035=AXIS2_PLACEMENT_3D('',#26178,#21175,#21176);
#18036=AXIS2_PLACEMENT_3D('',#26179,#21177,#21178);
#18037=AXIS2_PLACEMENT_3D('',#26180,#21179,#21180);
#18038=AXIS2_PLACEMENT_3D('',#26181,#21181,#21182);
#18039=AXIS2_PLACEMENT_3D('',#26182,#21183,#21184);
#18040=AXIS2_PLACEMENT_3D('',#26184,#21185,#21186);
#18041=AXIS2_PLACEMENT_3D('',#26187,#21188,#21189);
#18042=AXIS2_PLACEMENT_3D('',#26188,#21190,#21191);
#18043=AXIS2_PLACEMENT_3D('',#26197,#21196,#21197);
#18044=AXIS2_PLACEMENT_3D('',#26203,#21201,#21202);
#18045=AXIS2_PLACEMENT_3D('',#26209,#21206,#21207);
#18046=AXIS2_PLACEMENT_3D('',#26211,#21208,#21209);
#18047=AXIS2_PLACEMENT_3D('',#26212,#21210,#21211);
#18048=AXIS2_PLACEMENT_3D('',#26213,#21212,#21213);
#18049=AXIS2_PLACEMENT_3D('',#26214,#21214,#21215);
#18050=AXIS2_PLACEMENT_3D('',#26215,#21216,#21217);
#18051=AXIS2_PLACEMENT_3D('',#26220,#21219,#21220);
#18052=AXIS2_PLACEMENT_3D('',#26223,#21222,#21223);
#18053=AXIS2_PLACEMENT_3D('',#26224,#21224,#21225);
#18054=AXIS2_PLACEMENT_3D('',#26228,#21227,#21228);
#18055=AXIS2_PLACEMENT_3D('',#26230,#21230,#21231);
#18056=AXIS2_PLACEMENT_3D('',#26234,#21234,#21235);
#18057=AXIS2_PLACEMENT_3D('',#26237,#21237,#21238);
#18058=AXIS2_PLACEMENT_3D('',#26238,#21239,#21240);
#18059=AXIS2_PLACEMENT_3D('',#26240,#21242,#21243);
#18060=AXIS2_PLACEMENT_3D('',#26243,#21245,#21246);
#18061=AXIS2_PLACEMENT_3D('',#26244,#21247,#21248);
#18062=AXIS2_PLACEMENT_3D('',#26245,#21249,#21250);
#18063=AXIS2_PLACEMENT_3D('',#26246,#21251,#21252);
#18064=AXIS2_PLACEMENT_3D('',#26248,#21253,#21254);
#18065=AXIS2_PLACEMENT_3D('',#26251,#21256,#21257);
#18066=AXIS2_PLACEMENT_3D('',#26252,#21258,#21259);
#18067=AXIS2_PLACEMENT_3D('',#26254,#21260,#21261);
#18068=AXIS2_PLACEMENT_3D('',#26257,#21263,#21264);
#18069=AXIS2_PLACEMENT_3D('',#26258,#21265,#21266);
#18070=AXIS2_PLACEMENT_3D('',#26259,#21267,#21268);
#18071=AXIS2_PLACEMENT_3D('',#26260,#21269,#21270);
#18072=AXIS2_PLACEMENT_3D('',#26261,#21271,#21272);
#18073=AXIS2_PLACEMENT_3D('',#26263,#21273,#21274);
#18074=AXIS2_PLACEMENT_3D('',#26266,#21276,#21277);
#18075=AXIS2_PLACEMENT_3D('',#26267,#21278,#21279);
#18076=AXIS2_PLACEMENT_3D('',#26269,#21280,#21281);
#18077=AXIS2_PLACEMENT_3D('',#26272,#21283,#21284);
#18078=AXIS2_PLACEMENT_3D('',#26273,#21285,#21286);
#18079=AXIS2_PLACEMENT_3D('',#26274,#21287,#21288);
#18080=AXIS2_PLACEMENT_3D('',#26275,#21289,#21290);
#18081=AXIS2_PLACEMENT_3D('',#26276,#21291,#21292);
#18082=AXIS2_PLACEMENT_3D('',#26278,#21293,#21294);
#18083=AXIS2_PLACEMENT_3D('',#26281,#21296,#21297);
#18084=AXIS2_PLACEMENT_3D('',#26282,#21298,#21299);
#18085=AXIS2_PLACEMENT_3D('',#26284,#21300,#21301);
#18086=AXIS2_PLACEMENT_3D('',#26287,#21303,#21304);
#18087=AXIS2_PLACEMENT_3D('',#26288,#21305,#21306);
#18088=AXIS2_PLACEMENT_3D('',#26289,#21307,#21308);
#18089=AXIS2_PLACEMENT_3D('',#26290,#21309,#21310);
#18090=AXIS2_PLACEMENT_3D('',#26291,#21311,#21312);
#18091=AXIS2_PLACEMENT_3D('',#26293,#21313,#21314);
#18092=AXIS2_PLACEMENT_3D('',#26296,#21316,#21317);
#18093=AXIS2_PLACEMENT_3D('',#26297,#21318,#21319);
#18094=AXIS2_PLACEMENT_3D('',#26299,#21320,#21321);
#18095=AXIS2_PLACEMENT_3D('',#26302,#21323,#21324);
#18096=AXIS2_PLACEMENT_3D('',#26303,#21325,#21326);
#18097=AXIS2_PLACEMENT_3D('',#26304,#21327,#21328);
#18098=AXIS2_PLACEMENT_3D('',#26305,#21329,#21330);
#18099=AXIS2_PLACEMENT_3D('',#26306,#21331,#21332);
#18100=AXIS2_PLACEMENT_3D('',#26308,#21333,#21334);
#18101=AXIS2_PLACEMENT_3D('',#26311,#21336,#21337);
#18102=AXIS2_PLACEMENT_3D('',#26312,#21338,#21339);
#18103=AXIS2_PLACEMENT_3D('',#26314,#21340,#21341);
#18104=AXIS2_PLACEMENT_3D('',#26317,#21343,#21344);
#18105=AXIS2_PLACEMENT_3D('',#26318,#21345,#21346);
#18106=AXIS2_PLACEMENT_3D('',#26319,#21347,#21348);
#18107=AXIS2_PLACEMENT_3D('',#26320,#21349,#21350);
#18108=AXIS2_PLACEMENT_3D('',#26321,#21351,#21352);
#18109=AXIS2_PLACEMENT_3D('',#26330,#21357,#21358);
#18110=AXIS2_PLACEMENT_3D('',#26336,#21362,#21363);
#18111=AXIS2_PLACEMENT_3D('',#26342,#21367,#21368);
#18112=AXIS2_PLACEMENT_3D('',#26348,#21372,#21373);
#18113=AXIS2_PLACEMENT_3D('',#26354,#21377,#21378);
#18114=AXIS2_PLACEMENT_3D('',#26357,#21381,#21382);
#18115=AXIS2_PLACEMENT_3D('',#26358,#21383,#21384);
#18116=AXIS2_PLACEMENT_3D('',#26359,#21385,#21386);
#18117=AXIS2_PLACEMENT_3D('',#26361,#21387,#21388);
#18118=AXIS2_PLACEMENT_3D('',#26363,#21389,#21390);
#18119=AXIS2_PLACEMENT_3D('',#26364,#21391,#21392);
#18120=AXIS2_PLACEMENT_3D('',#26367,#21394,#21395);
#18121=AXIS2_PLACEMENT_3D('',#26368,#21396,#21397);
#18122=AXIS2_PLACEMENT_3D('',#26369,#21398,#21399);
#18123=AXIS2_PLACEMENT_3D('',#26371,#21400,#21401);
#18124=AXIS2_PLACEMENT_3D('',#26372,#21402,#21403);
#18125=AXIS2_PLACEMENT_3D('',#26374,#21404,#21405);
#18126=AXIS2_PLACEMENT_3D('',#26376,#21407,#21408);
#18127=AXIS2_PLACEMENT_3D('',#26378,#21409,#21410);
#18128=AXIS2_PLACEMENT_3D('',#26380,#21412,#21413);
#18129=AXIS2_PLACEMENT_3D('',#26382,#21414,#21415);
#18130=AXIS2_PLACEMENT_3D('',#26384,#21417,#21418);
#18131=AXIS2_PLACEMENT_3D('',#26386,#21419,#21420);
#18132=AXIS2_PLACEMENT_3D('',#26387,#21421,#21422);
#18133=AXIS2_PLACEMENT_3D('',#26389,#21423,#21424);
#18134=AXIS2_PLACEMENT_3D('',#26391,#21426,#21427);
#18135=AXIS2_PLACEMENT_3D('',#26393,#21429,#21430);
#18136=AXIS2_PLACEMENT_3D('',#26394,#21431,#21432);
#18137=AXIS2_PLACEMENT_3D('',#26395,#21433,#21434);
#18138=AXIS2_PLACEMENT_3D('',#26397,#21435,#21436);
#18139=AXIS2_PLACEMENT_3D('',#26400,#21438,#21439);
#18140=AXIS2_PLACEMENT_3D('',#26401,#21440,#21441);
#18141=AXIS2_PLACEMENT_3D('',#26402,#21442,#21443);
#18142=AXIS2_PLACEMENT_3D('',#26411,#21448,#21449);
#18143=AXIS2_PLACEMENT_3D('',#26413,#21450,#21451);
#18144=AXIS2_PLACEMENT_3D('',#26417,#21454,#21455);
#18145=AXIS2_PLACEMENT_3D('',#26423,#21459,#21460);
#18146=AXIS2_PLACEMENT_3D('',#26425,#21462,#21463);
#18147=AXIS2_PLACEMENT_3D('',#26426,#21464,#21465);
#18148=AXIS2_PLACEMENT_3D('',#26427,#21466,#21467);
#18149=AXIS2_PLACEMENT_3D('',#26429,#21468,#21469);
#18150=AXIS2_PLACEMENT_3D('',#26431,#21470,#21471);
#18151=AXIS2_PLACEMENT_3D('',#26432,#21472,#21473);
#18152=AXIS2_PLACEMENT_3D('',#26434,#21474,#21475);
#18153=AXIS2_PLACEMENT_3D('',#26436,#21476,#21477);
#18154=AXIS2_PLACEMENT_3D('',#26437,#21478,#21479);
#18155=AXIS2_PLACEMENT_3D('',#26439,#21481,#21482);
#18156=AXIS2_PLACEMENT_3D('',#26442,#21484,#21485);
#18157=AXIS2_PLACEMENT_3D('',#26443,#21486,#21487);
#18158=AXIS2_PLACEMENT_3D('',#26445,#21488,#21489);
#18159=AXIS2_PLACEMENT_3D('',#26447,#21491,#21492);
#18160=AXIS2_PLACEMENT_3D('',#26448,#21493,#21494);
#18161=AXIS2_PLACEMENT_3D('',#26449,#21495,#21496);
#18162=AXIS2_PLACEMENT_3D('',#26450,#21497,#21498);
#18163=AXIS2_PLACEMENT_3D('',#26452,#21499,#21500);
#18164=AXIS2_PLACEMENT_3D('',#26455,#21502,#21503);
#18165=AXIS2_PLACEMENT_3D('',#26456,#21504,#21505);
#18166=AXIS2_PLACEMENT_3D('',#26458,#21506,#21507);
#18167=AXIS2_PLACEMENT_3D('',#26461,#21509,#21510);
#18168=AXIS2_PLACEMENT_3D('',#26462,#21511,#21512);
#18169=AXIS2_PLACEMENT_3D('',#26463,#21513,#21514);
#18170=AXIS2_PLACEMENT_3D('',#26464,#21515,#21516);
#18171=AXIS2_PLACEMENT_3D('',#26465,#21517,#21518);
#18172=AXIS2_PLACEMENT_3D('',#26467,#21519,#21520);
#18173=AXIS2_PLACEMENT_3D('',#26470,#21522,#21523);
#18174=AXIS2_PLACEMENT_3D('',#26471,#21524,#21525);
#18175=AXIS2_PLACEMENT_3D('',#26473,#21526,#21527);
#18176=AXIS2_PLACEMENT_3D('',#26476,#21529,#21530);
#18177=AXIS2_PLACEMENT_3D('',#26477,#21531,#21532);
#18178=AXIS2_PLACEMENT_3D('',#26478,#21533,#21534);
#18179=AXIS2_PLACEMENT_3D('',#26479,#21535,#21536);
#18180=AXIS2_PLACEMENT_3D('',#26480,#21537,#21538);
#18181=AXIS2_PLACEMENT_3D('',#26484,#21540,#21541);
#18182=AXIS2_PLACEMENT_3D('',#26485,#21542,#21543);
#18183=AXIS2_PLACEMENT_3D('',#26502,#21544,#21545);
#18184=AXIS2_PLACEMENT_3D('',#26543,#21547,#21548);
#18185=AXIS2_PLACEMENT_3D('',#26558,#21549,#21550);
#18186=AXIS2_PLACEMENT_3D('',#26560,#21552,#21553);
#18187=AXIS2_PLACEMENT_3D('',#26562,#21554,#21555);
#18188=AXIS2_PLACEMENT_3D('',#26565,#21557,#21558);
#18189=AXIS2_PLACEMENT_3D('',#26566,#21559,#21560);
#18190=AXIS2_PLACEMENT_3D('',#26568,#21561,#21562);
#18191=AXIS2_PLACEMENT_3D('',#26571,#21564,#21565);
#18192=AXIS2_PLACEMENT_3D('',#26572,#21566,#21567);
#18193=AXIS2_PLACEMENT_3D('',#26573,#21568,#21569);
#18194=AXIS2_PLACEMENT_3D('',#26574,#21570,#21571);
#18195=AXIS2_PLACEMENT_3D('',#26575,#21572,#21573);
#18196=AXIS2_PLACEMENT_3D('',#26577,#21574,#21575);
#18197=AXIS2_PLACEMENT_3D('',#26580,#21577,#21578);
#18198=AXIS2_PLACEMENT_3D('',#26581,#21579,#21580);
#18199=AXIS2_PLACEMENT_3D('',#26583,#21581,#21582);
#18200=AXIS2_PLACEMENT_3D('',#26586,#21584,#21585);
#18201=AXIS2_PLACEMENT_3D('',#26587,#21586,#21587);
#18202=AXIS2_PLACEMENT_3D('',#26588,#21588,#21589);
#18203=AXIS2_PLACEMENT_3D('',#26589,#21590,#21591);
#18204=AXIS2_PLACEMENT_3D('',#26590,#21592,#21593);
#18205=AXIS2_PLACEMENT_3D('',#26591,#21594,#21595);
#18206=AXIS2_PLACEMENT_3D('',#26593,#21596,#21597);
#18207=AXIS2_PLACEMENT_3D('',#26596,#21599,#21600);
#18208=AXIS2_PLACEMENT_3D('',#26597,#21601,#21602);
#18209=AXIS2_PLACEMENT_3D('',#26598,#21603,#21604);
#18210=AXIS2_PLACEMENT_3D('',#26607,#21609,#21610);
#18211=AXIS2_PLACEMENT_3D('',#26609,#21611,#21612);
#18212=AXIS2_PLACEMENT_3D('',#26613,#21615,#21616);
#18213=AXIS2_PLACEMENT_3D('',#26619,#21620,#21621);
#18214=AXIS2_PLACEMENT_3D('',#26621,#21623,#21624);
#18215=AXIS2_PLACEMENT_3D('',#26622,#21625,#21626);
#18216=AXIS2_PLACEMENT_3D('',#26623,#21627,#21628);
#18217=AXIS2_PLACEMENT_3D('',#26625,#21629,#21630);
#18218=AXIS2_PLACEMENT_3D('',#26627,#21631,#21632);
#18219=AXIS2_PLACEMENT_3D('',#26628,#21633,#21634);
#18220=AXIS2_PLACEMENT_3D('',#26630,#21635,#21636);
#18221=AXIS2_PLACEMENT_3D('',#26632,#21637,#21638);
#18222=AXIS2_PLACEMENT_3D('',#26633,#21639,#21640);
#18223=AXIS2_PLACEMENT_3D('',#26635,#21642,#21643);
#18224=AXIS2_PLACEMENT_3D('',#26638,#21645,#21646);
#18225=AXIS2_PLACEMENT_3D('',#26639,#21647,#21648);
#18226=AXIS2_PLACEMENT_3D('',#26641,#21649,#21650);
#18227=AXIS2_PLACEMENT_3D('',#26643,#21652,#21653);
#18228=AXIS2_PLACEMENT_3D('',#26644,#21654,#21655);
#18229=AXIS2_PLACEMENT_3D('',#26645,#21656,#21657);
#18230=AXIS2_PLACEMENT_3D('',#26646,#21658,#21659);
#18231=AXIS2_PLACEMENT_3D('',#26648,#21660,#21661);
#18232=AXIS2_PLACEMENT_3D('',#26651,#21663,#21664);
#18233=AXIS2_PLACEMENT_3D('',#26652,#21665,#21666);
#18234=AXIS2_PLACEMENT_3D('',#26654,#21667,#21668);
#18235=AXIS2_PLACEMENT_3D('',#26657,#21670,#21671);
#18236=AXIS2_PLACEMENT_3D('',#26658,#21672,#21673);
#18237=AXIS2_PLACEMENT_3D('',#26659,#21674,#21675);
#18238=AXIS2_PLACEMENT_3D('',#26660,#21676,#21677);
#18239=AXIS2_PLACEMENT_3D('',#26661,#21678,#21679);
#18240=AXIS2_PLACEMENT_3D('',#26663,#21680,#21681);
#18241=AXIS2_PLACEMENT_3D('',#26666,#21683,#21684);
#18242=AXIS2_PLACEMENT_3D('',#26667,#21685,#21686);
#18243=AXIS2_PLACEMENT_3D('',#26669,#21687,#21688);
#18244=AXIS2_PLACEMENT_3D('',#26672,#21690,#21691);
#18245=AXIS2_PLACEMENT_3D('',#26673,#21692,#21693);
#18246=AXIS2_PLACEMENT_3D('',#26674,#21694,#21695);
#18247=AXIS2_PLACEMENT_3D('',#26675,#21696,#21697);
#18248=AXIS2_PLACEMENT_3D('',#26676,#21698,#21699);
#18249=AXIS2_PLACEMENT_3D('',#26680,#21701,#21702);
#18250=AXIS2_PLACEMENT_3D('',#26681,#21703,#21704);
#18251=AXIS2_PLACEMENT_3D('',#26694,#21705,#21706);
#18252=AXIS2_PLACEMENT_3D('',#26735,#21708,#21709);
#18253=AXIS2_PLACEMENT_3D('',#26746,#21710,#21711);
#18254=AXIS2_PLACEMENT_3D('',#26748,#21713,#21714);
#18255=AXIS2_PLACEMENT_3D('',#26750,#21715,#21716);
#18256=AXIS2_PLACEMENT_3D('',#26753,#21718,#21719);
#18257=AXIS2_PLACEMENT_3D('',#26754,#21720,#21721);
#18258=AXIS2_PLACEMENT_3D('',#26756,#21722,#21723);
#18259=AXIS2_PLACEMENT_3D('',#26759,#21725,#21726);
#18260=AXIS2_PLACEMENT_3D('',#26760,#21727,#21728);
#18261=AXIS2_PLACEMENT_3D('',#26761,#21729,#21730);
#18262=AXIS2_PLACEMENT_3D('',#26762,#21731,#21732);
#18263=AXIS2_PLACEMENT_3D('',#26763,#21733,#21734);
#18264=AXIS2_PLACEMENT_3D('',#26765,#21735,#21736);
#18265=AXIS2_PLACEMENT_3D('',#26768,#21738,#21739);
#18266=AXIS2_PLACEMENT_3D('',#26769,#21740,#21741);
#18267=AXIS2_PLACEMENT_3D('',#26771,#21742,#21743);
#18268=AXIS2_PLACEMENT_3D('',#26774,#21745,#21746);
#18269=AXIS2_PLACEMENT_3D('',#26775,#21747,#21748);
#18270=AXIS2_PLACEMENT_3D('',#26776,#21749,#21750);
#18271=AXIS2_PLACEMENT_3D('',#26777,#21751,#21752);
#18272=AXIS2_PLACEMENT_3D('',#26778,#21753,#21754);
#18273=AXIS2_PLACEMENT_3D('',#26787,#21759,#21760);
#18274=AXIS2_PLACEMENT_3D('',#26793,#21764,#21765);
#18275=AXIS2_PLACEMENT_3D('',#26799,#21769,#21770);
#18276=AXIS2_PLACEMENT_3D('',#26802,#21771,#21772);
#18277=AXIS2_PLACEMENT_3D('',#26948,#21774,#21775);
#18278=AXIS2_PLACEMENT_3D('',#27094,#21777,#21778);
#18279=AXIS2_PLACEMENT_3D('',#27240,#21780,#21781);
#18280=AXIS2_PLACEMENT_3D('',#27386,#21783,#21784);
#18281=AXIS2_PLACEMENT_3D('',#27532,#21786,#21787);
#18282=AXIS2_PLACEMENT_3D('',#27678,#21789,#21790);
#18283=AXIS2_PLACEMENT_3D('',#27824,#21792,#21793);
#18284=AXIS2_PLACEMENT_3D('',#27970,#21795,#21796);
#18285=AXIS2_PLACEMENT_3D('',#28116,#21798,#21799);
#18286=AXIS2_PLACEMENT_3D('',#28262,#21801,#21802);
#18287=AXIS2_PLACEMENT_3D('',#28408,#21804,#21805);
#18288=AXIS2_PLACEMENT_3D('',#28554,#21807,#21808);
#18289=AXIS2_PLACEMENT_3D('',#28700,#21810,#21811);
#18290=AXIS2_PLACEMENT_3D('',#28846,#21813,#21814);
#18291=AXIS2_PLACEMENT_3D('',#28992,#21816,#21817);
#18292=AXIS2_PLACEMENT_3D('',#29138,#21819,#21820);
#18293=AXIS2_PLACEMENT_3D('',#29284,#21822,#21823);
#18294=AXIS2_PLACEMENT_3D('',#29430,#21825,#21826);
#18295=AXIS2_PLACEMENT_3D('',#29576,#21828,#21829);
#18296=AXIS2_PLACEMENT_3D('',#29720,#21831,#21832);
#18297=AXIS2_PLACEMENT_3D('',#29721,#21833,#21834);
#18298=AXIS2_PLACEMENT_3D('',#29722,#21835,#21836);
#18299=AXIS2_PLACEMENT_3D('',#29723,#21837,#21838);
#18300=AXIS2_PLACEMENT_3D('',#29725,#21839,#21840);
#18301=AXIS2_PLACEMENT_3D('',#29728,#21842,#21843);
#18302=AXIS2_PLACEMENT_3D('',#29729,#21844,#21845);
#18303=AXIS2_PLACEMENT_3D('',#29944,#21848,#21849);
#18304=AXIS2_PLACEMENT_3D('',#30160,#21853,#21854);
#18305=AXIS2_PLACEMENT_3D('',#30162,#21855,#21856);
#18306=AXIS2_PLACEMENT_3D('',#30376,#21859,#21860);
#18307=AXIS2_PLACEMENT_3D('',#30592,#21864,#21865);
#18308=AXIS2_PLACEMENT_3D('',#30594,#21866,#21867);
#18309=AXIS2_PLACEMENT_3D('',#30808,#21870,#21871);
#18310=AXIS2_PLACEMENT_3D('',#31024,#21875,#21876);
#18311=AXIS2_PLACEMENT_3D('',#31026,#21877,#21878);
#18312=AXIS2_PLACEMENT_3D('',#31240,#21881,#21882);
#18313=AXIS2_PLACEMENT_3D('',#31456,#21886,#21887);
#18314=AXIS2_PLACEMENT_3D('',#31458,#21888,#21889);
#18315=AXIS2_PLACEMENT_3D('',#31672,#21892,#21893);
#18316=AXIS2_PLACEMENT_3D('',#31888,#21897,#21898);
#18317=AXIS2_PLACEMENT_3D('',#31890,#21899,#21900);
#18318=AXIS2_PLACEMENT_3D('',#32104,#21903,#21904);
#18319=AXIS2_PLACEMENT_3D('',#32320,#21908,#21909);
#18320=AXIS2_PLACEMENT_3D('',#32322,#21910,#21911);
#18321=AXIS2_PLACEMENT_3D('',#32536,#21914,#21915);
#18322=AXIS2_PLACEMENT_3D('',#32752,#21919,#21920);
#18323=AXIS2_PLACEMENT_3D('',#32754,#21921,#21922);
#18324=AXIS2_PLACEMENT_3D('',#32968,#21925,#21926);
#18325=AXIS2_PLACEMENT_3D('',#33184,#21930,#21931);
#18326=AXIS2_PLACEMENT_3D('',#33186,#21932,#21933);
#18327=AXIS2_PLACEMENT_3D('',#33400,#21936,#21937);
#18328=AXIS2_PLACEMENT_3D('',#33616,#21941,#21942);
#18329=AXIS2_PLACEMENT_3D('',#33618,#21943,#21944);
#18330=AXIS2_PLACEMENT_3D('',#33832,#21947,#21948);
#18331=AXIS2_PLACEMENT_3D('',#34048,#21952,#21953);
#18332=AXIS2_PLACEMENT_3D('',#34050,#21954,#21955);
#18333=AXIS2_PLACEMENT_3D('',#34264,#21958,#21959);
#18334=AXIS2_PLACEMENT_3D('',#34480,#21963,#21964);
#18335=AXIS2_PLACEMENT_3D('',#34482,#21965,#21966);
#18336=AXIS2_PLACEMENT_3D('',#34696,#21969,#21970);
#18337=AXIS2_PLACEMENT_3D('',#34912,#21974,#21975);
#18338=AXIS2_PLACEMENT_3D('',#34914,#21976,#21977);
#18339=AXIS2_PLACEMENT_3D('',#35128,#21980,#21981);
#18340=AXIS2_PLACEMENT_3D('',#35344,#21985,#21986);
#18341=AXIS2_PLACEMENT_3D('',#35346,#21987,#21988);
#18342=AXIS2_PLACEMENT_3D('',#35560,#21991,#21992);
#18343=AXIS2_PLACEMENT_3D('',#35776,#21996,#21997);
#18344=AXIS2_PLACEMENT_3D('',#35778,#21998,#21999);
#18345=AXIS2_PLACEMENT_3D('',#35992,#22002,#22003);
#18346=AXIS2_PLACEMENT_3D('',#36208,#22007,#22008);
#18347=AXIS2_PLACEMENT_3D('',#36210,#22009,#22010);
#18348=AXIS2_PLACEMENT_3D('',#36424,#22013,#22014);
#18349=AXIS2_PLACEMENT_3D('',#36640,#22018,#22019);
#18350=AXIS2_PLACEMENT_3D('',#36642,#22020,#22021);
#18351=AXIS2_PLACEMENT_3D('',#36856,#22024,#22025);
#18352=AXIS2_PLACEMENT_3D('',#37072,#22029,#22030);
#18353=AXIS2_PLACEMENT_3D('',#37074,#22031,#22032);
#18354=AXIS2_PLACEMENT_3D('',#37288,#22035,#22036);
#18355=AXIS2_PLACEMENT_3D('',#37504,#22040,#22041);
#18356=AXIS2_PLACEMENT_3D('',#37506,#22042,#22043);
#18357=AXIS2_PLACEMENT_3D('',#37720,#22046,#22047);
#18358=AXIS2_PLACEMENT_3D('',#37936,#22051,#22052);
#18359=AXIS2_PLACEMENT_3D('',#37938,#22053,#22054);
#18360=AXIS2_PLACEMENT_3D('',#38152,#22057,#22058);
#18361=AXIS2_PLACEMENT_3D('',#38368,#22062,#22063);
#18362=AXIS2_PLACEMENT_3D('',#38369,#22064,#22065);
#18363=AXIS2_PLACEMENT_3D('',#38370,#22066,#22067);
#18364=AXIS2_PLACEMENT_3D('',#38371,#22068,#22069);
#18365=AXIS2_PLACEMENT_3D('',#38372,#22070,#22071);
#18366=AXIS2_PLACEMENT_3D('',#38389,#22080,#22081);
#18367=AXIS2_PLACEMENT_3D('',#38395,#22085,#22086);
#18368=AXIS2_PLACEMENT_3D('',#38399,#22089,#22090);
#18369=AXIS2_PLACEMENT_3D('',#38403,#22093,#22094);
#18370=AXIS2_PLACEMENT_3D('',#38407,#22097,#22098);
#18371=AXIS2_PLACEMENT_3D('',#38415,#22103,#22104);
#18372=AXIS2_PLACEMENT_3D('',#38417,#22106,#22107);
#18373=AXIS2_PLACEMENT_3D('',#38419,#22109,#22110);
#18374=AXIS2_PLACEMENT_3D('',#38421,#22112,#22113);
#18375=AXIS2_PLACEMENT_3D('',#38422,#22114,#22115);
#18376=AXIS2_PLACEMENT_3D('',#38423,#22116,#22117);
#18377=AXIS2_PLACEMENT_3D('',#38424,#22118,#22119);
#18378=AXIS2_PLACEMENT_3D('',#38426,#22120,#22121);
#18379=AXIS2_PLACEMENT_3D('',#38429,#22123,#22124);
#18380=AXIS2_PLACEMENT_3D('',#38430,#22125,#22126);
#18381=AXIS2_PLACEMENT_3D('',#38431,#22127,#22128);
#18382=AXIS2_PLACEMENT_3D('',#38440,#22133,#22134);
#18383=AXIS2_PLACEMENT_3D('',#38442,#22135,#22136);
#18384=AXIS2_PLACEMENT_3D('',#38446,#22139,#22140);
#18385=AXIS2_PLACEMENT_3D('',#38452,#22144,#22145);
#18386=AXIS2_PLACEMENT_3D('',#38454,#22147,#22148);
#18387=AXIS2_PLACEMENT_3D('',#38455,#22149,#22150);
#18388=AXIS2_PLACEMENT_3D('',#38456,#22151,#22152);
#18389=AXIS2_PLACEMENT_3D('',#38458,#22153,#22154);
#18390=AXIS2_PLACEMENT_3D('',#38460,#22155,#22156);
#18391=AXIS2_PLACEMENT_3D('',#38461,#22157,#22158);
#18392=AXIS2_PLACEMENT_3D('',#38463,#22159,#22160);
#18393=AXIS2_PLACEMENT_3D('',#38465,#22161,#22162);
#18394=AXIS2_PLACEMENT_3D('',#38466,#22163,#22164);
#18395=AXIS2_PLACEMENT_3D('',#38468,#22166,#22167);
#18396=AXIS2_PLACEMENT_3D('',#38471,#22169,#22170);
#18397=AXIS2_PLACEMENT_3D('',#38472,#22171,#22172);
#18398=AXIS2_PLACEMENT_3D('',#38474,#22173,#22174);
#18399=AXIS2_PLACEMENT_3D('',#38476,#22176,#22177);
#18400=AXIS2_PLACEMENT_3D('',#38477,#22178,#22179);
#18401=AXIS2_PLACEMENT_3D('',#38478,#22180,#22181);
#18402=AXIS2_PLACEMENT_3D('',#38479,#22182,#22183);
#18403=AXIS2_PLACEMENT_3D('',#38481,#22184,#22185);
#18404=AXIS2_PLACEMENT_3D('',#38484,#22187,#22188);
#18405=AXIS2_PLACEMENT_3D('',#38485,#22189,#22190);
#18406=AXIS2_PLACEMENT_3D('',#38487,#22191,#22192);
#18407=AXIS2_PLACEMENT_3D('',#38490,#22194,#22195);
#18408=AXIS2_PLACEMENT_3D('',#38491,#22196,#22197);
#18409=AXIS2_PLACEMENT_3D('',#38492,#22198,#22199);
#18410=AXIS2_PLACEMENT_3D('',#38493,#22200,#22201);
#18411=AXIS2_PLACEMENT_3D('',#38494,#22202,#22203);
#18412=AXIS2_PLACEMENT_3D('',#38496,#22204,#22205);
#18413=AXIS2_PLACEMENT_3D('',#38499,#22207,#22208);
#18414=AXIS2_PLACEMENT_3D('',#38500,#22209,#22210);
#18415=AXIS2_PLACEMENT_3D('',#38502,#22211,#22212);
#18416=AXIS2_PLACEMENT_3D('',#38505,#22214,#22215);
#18417=AXIS2_PLACEMENT_3D('',#38506,#22216,#22217);
#18418=AXIS2_PLACEMENT_3D('',#38507,#22218,#22219);
#18419=AXIS2_PLACEMENT_3D('',#38508,#22220,#22221);
#18420=AXIS2_PLACEMENT_3D('',#38509,#22222,#22223);
#18421=AXIS2_PLACEMENT_3D('',#38513,#22225,#22226);
#18422=AXIS2_PLACEMENT_3D('',#38514,#22227,#22228);
#18423=AXIS2_PLACEMENT_3D('',#38531,#22229,#22230);
#18424=AXIS2_PLACEMENT_3D('',#38572,#22232,#22233);
#18425=AXIS2_PLACEMENT_3D('',#38587,#22234,#22235);
#18426=AXIS2_PLACEMENT_3D('',#38589,#22237,#22238);
#18427=AXIS2_PLACEMENT_3D('',#38591,#22239,#22240);
#18428=AXIS2_PLACEMENT_3D('',#38594,#22242,#22243);
#18429=AXIS2_PLACEMENT_3D('',#38595,#22244,#22245);
#18430=AXIS2_PLACEMENT_3D('',#38597,#22246,#22247);
#18431=AXIS2_PLACEMENT_3D('',#38600,#22249,#22250);
#18432=AXIS2_PLACEMENT_3D('',#38601,#22251,#22252);
#18433=AXIS2_PLACEMENT_3D('',#38602,#22253,#22254);
#18434=AXIS2_PLACEMENT_3D('',#38603,#22255,#22256);
#18435=AXIS2_PLACEMENT_3D('',#38604,#22257,#22258);
#18436=AXIS2_PLACEMENT_3D('',#38606,#22259,#22260);
#18437=AXIS2_PLACEMENT_3D('',#38609,#22262,#22263);
#18438=AXIS2_PLACEMENT_3D('',#38610,#22264,#22265);
#18439=AXIS2_PLACEMENT_3D('',#38612,#22266,#22267);
#18440=AXIS2_PLACEMENT_3D('',#38615,#22269,#22270);
#18441=AXIS2_PLACEMENT_3D('',#38616,#22271,#22272);
#18442=AXIS2_PLACEMENT_3D('',#38617,#22273,#22274);
#18443=AXIS2_PLACEMENT_3D('',#38618,#22275,#22276);
#18444=AXIS2_PLACEMENT_3D('',#38619,#22277,#22278);
#18445=AXIS2_PLACEMENT_3D('',#38621,#22279,#22280);
#18446=AXIS2_PLACEMENT_3D('',#38624,#22282,#22283);
#18447=AXIS2_PLACEMENT_3D('',#38625,#22284,#22285);
#18448=AXIS2_PLACEMENT_3D('',#38627,#22286,#22287);
#18449=AXIS2_PLACEMENT_3D('',#38630,#22289,#22290);
#18450=AXIS2_PLACEMENT_3D('',#38631,#22291,#22292);
#18451=AXIS2_PLACEMENT_3D('',#38632,#22293,#22294);
#18452=AXIS2_PLACEMENT_3D('',#38633,#22295,#22296);
#18453=AXIS2_PLACEMENT_3D('',#38634,#22297,#22298);
#18454=AXIS2_PLACEMENT_3D('',#38638,#22300,#22301);
#18455=AXIS2_PLACEMENT_3D('',#38639,#22302,#22303);
#18456=AXIS2_PLACEMENT_3D('',#38652,#22304,#22305);
#18457=AXIS2_PLACEMENT_3D('',#38693,#22307,#22308);
#18458=AXIS2_PLACEMENT_3D('',#38704,#22309,#22310);
#18459=AXIS2_PLACEMENT_3D('',#38706,#22312,#22313);
#18460=AXIS2_PLACEMENT_3D('',#38715,#22318,#22319);
#18461=AXIS2_PLACEMENT_3D('',#38717,#22320,#22321);
#18462=AXIS2_PLACEMENT_3D('',#38719,#22323,#22324);
#18463=AXIS2_PLACEMENT_3D('',#38721,#22325,#22326);
#18464=AXIS2_PLACEMENT_3D('',#38723,#22328,#22329);
#18465=AXIS2_PLACEMENT_3D('',#38725,#22331,#22332);
#18466=AXIS2_PLACEMENT_3D('',#38727,#22333,#22334);
#18467=AXIS2_PLACEMENT_3D('',#38730,#22336,#22337);
#18468=AXIS2_PLACEMENT_3D('',#38731,#22338,#22339);
#18469=AXIS2_PLACEMENT_3D('',#38733,#22340,#22341);
#18470=AXIS2_PLACEMENT_3D('',#38736,#22343,#22344);
#18471=AXIS2_PLACEMENT_3D('',#38737,#22345,#22346);
#18472=AXIS2_PLACEMENT_3D('',#38738,#22347,#22348);
#18473=AXIS2_PLACEMENT_3D('',#38739,#22349,#22350);
#18474=AXIS2_PLACEMENT_3D('',#38740,#22351,#22352);
#18475=AXIS2_PLACEMENT_3D('',#38742,#22353,#22354);
#18476=AXIS2_PLACEMENT_3D('',#38745,#22356,#22357);
#18477=AXIS2_PLACEMENT_3D('',#38746,#22358,#22359);
#18478=AXIS2_PLACEMENT_3D('',#38748,#22360,#22361);
#18479=AXIS2_PLACEMENT_3D('',#38751,#22363,#22364);
#18480=AXIS2_PLACEMENT_3D('',#38752,#22365,#22366);
#18481=AXIS2_PLACEMENT_3D('',#38753,#22367,#22368);
#18482=AXIS2_PLACEMENT_3D('',#38754,#22369,#22370);
#18483=AXIS2_PLACEMENT_3D('',#38755,#22371,#22372);
#18484=AXIS2_PLACEMENT_3D('',#38764,#22377,#22378);
#18485=AXIS2_PLACEMENT_3D('',#38770,#22382,#22383);
#18486=AXIS2_PLACEMENT_3D('',#38776,#22387,#22388);
#18487=AXIS2_PLACEMENT_3D('',#38779,#22389,#22390);
#18488=AXIS2_PLACEMENT_3D('',#38925,#22392,#22393);
#18489=AXIS2_PLACEMENT_3D('',#39071,#22395,#22396);
#18490=AXIS2_PLACEMENT_3D('',#39217,#22398,#22399);
#18491=AXIS2_PLACEMENT_3D('',#39363,#22401,#22402);
#18492=AXIS2_PLACEMENT_3D('',#39509,#22404,#22405);
#18493=AXIS2_PLACEMENT_3D('',#39655,#22407,#22408);
#18494=AXIS2_PLACEMENT_3D('',#39801,#22410,#22411);
#18495=AXIS2_PLACEMENT_3D('',#39947,#22413,#22414);
#18496=AXIS2_PLACEMENT_3D('',#40093,#22416,#22417);
#18497=AXIS2_PLACEMENT_3D('',#40239,#22419,#22420);
#18498=AXIS2_PLACEMENT_3D('',#40385,#22422,#22423);
#18499=AXIS2_PLACEMENT_3D('',#40531,#22425,#22426);
#18500=AXIS2_PLACEMENT_3D('',#40677,#22428,#22429);
#18501=AXIS2_PLACEMENT_3D('',#40823,#22431,#22432);
#18502=AXIS2_PLACEMENT_3D('',#40969,#22434,#22435);
#18503=AXIS2_PLACEMENT_3D('',#41115,#22437,#22438);
#18504=AXIS2_PLACEMENT_3D('',#41261,#22440,#22441);
#18505=AXIS2_PLACEMENT_3D('',#41407,#22443,#22444);
#18506=AXIS2_PLACEMENT_3D('',#41553,#22446,#22447);
#18507=AXIS2_PLACEMENT_3D('',#41699,#22449,#22450);
#18508=AXIS2_PLACEMENT_3D('',#41845,#22452,#22453);
#18509=AXIS2_PLACEMENT_3D('',#41991,#22455,#22456);
#18510=AXIS2_PLACEMENT_3D('',#42137,#22458,#22459);
#18511=AXIS2_PLACEMENT_3D('',#42283,#22461,#22462);
#18512=AXIS2_PLACEMENT_3D('',#42429,#22464,#22465);
#18513=AXIS2_PLACEMENT_3D('',#42575,#22467,#22468);
#18514=AXIS2_PLACEMENT_3D('',#42721,#22470,#22471);
#18515=AXIS2_PLACEMENT_3D('',#42867,#22473,#22474);
#18516=AXIS2_PLACEMENT_3D('',#43013,#22476,#22477);
#18517=AXIS2_PLACEMENT_3D('',#43159,#22479,#22480);
#18518=AXIS2_PLACEMENT_3D('',#43305,#22482,#22483);
#18519=AXIS2_PLACEMENT_3D('',#43451,#22485,#22486);
#18520=AXIS2_PLACEMENT_3D('',#43597,#22488,#22489);
#18521=AXIS2_PLACEMENT_3D('',#43743,#22491,#22492);
#18522=AXIS2_PLACEMENT_3D('',#43889,#22494,#22495);
#18523=AXIS2_PLACEMENT_3D('',#44035,#22497,#22498);
#18524=AXIS2_PLACEMENT_3D('',#44181,#22500,#22501);
#18525=AXIS2_PLACEMENT_3D('',#44327,#22503,#22504);
#18526=AXIS2_PLACEMENT_3D('',#44473,#22506,#22507);
#18527=AXIS2_PLACEMENT_3D('',#44617,#22509,#22510);
#18528=AXIS2_PLACEMENT_3D('',#44618,#22511,#22512);
#18529=AXIS2_PLACEMENT_3D('',#44619,#22513,#22514);
#18530=AXIS2_PLACEMENT_3D('',#44620,#22515,#22516);
#18531=AXIS2_PLACEMENT_3D('',#44622,#22517,#22518);
#18532=AXIS2_PLACEMENT_3D('',#44625,#22520,#22521);
#18533=AXIS2_PLACEMENT_3D('',#44626,#22522,#22523);
#18534=AXIS2_PLACEMENT_3D('',#45065,#22526,#22527);
#18535=AXIS2_PLACEMENT_3D('',#45067,#22529,#22530);
#18536=AXIS2_PLACEMENT_3D('',#45069,#22531,#22532);
#18537=AXIS2_PLACEMENT_3D('',#45507,#22535,#22536);
#18538=AXIS2_PLACEMENT_3D('',#45509,#22538,#22539);
#18539=AXIS2_PLACEMENT_3D('',#45511,#22540,#22541);
#18540=AXIS2_PLACEMENT_3D('',#45949,#22544,#22545);
#18541=AXIS2_PLACEMENT_3D('',#45951,#22547,#22548);
#18542=AXIS2_PLACEMENT_3D('',#45953,#22549,#22550);
#18543=AXIS2_PLACEMENT_3D('',#46391,#22553,#22554);
#18544=AXIS2_PLACEMENT_3D('',#46393,#22556,#22557);
#18545=AXIS2_PLACEMENT_3D('',#46395,#22558,#22559);
#18546=AXIS2_PLACEMENT_3D('',#46833,#22562,#22563);
#18547=AXIS2_PLACEMENT_3D('',#46835,#22565,#22566);
#18548=AXIS2_PLACEMENT_3D('',#46837,#22567,#22568);
#18549=AXIS2_PLACEMENT_3D('',#47275,#22571,#22572);
#18550=AXIS2_PLACEMENT_3D('',#47277,#22574,#22575);
#18551=AXIS2_PLACEMENT_3D('',#47279,#22576,#22577);
#18552=AXIS2_PLACEMENT_3D('',#47717,#22580,#22581);
#18553=AXIS2_PLACEMENT_3D('',#47719,#22583,#22584);
#18554=AXIS2_PLACEMENT_3D('',#47721,#22585,#22586);
#18555=AXIS2_PLACEMENT_3D('',#48159,#22589,#22590);
#18556=AXIS2_PLACEMENT_3D('',#48161,#22592,#22593);
#18557=AXIS2_PLACEMENT_3D('',#48163,#22594,#22595);
#18558=AXIS2_PLACEMENT_3D('',#48601,#22598,#22599);
#18559=AXIS2_PLACEMENT_3D('',#48603,#22601,#22602);
#18560=AXIS2_PLACEMENT_3D('',#48605,#22603,#22604);
#18561=AXIS2_PLACEMENT_3D('',#49043,#22607,#22608);
#18562=AXIS2_PLACEMENT_3D('',#49045,#22610,#22611);
#18563=AXIS2_PLACEMENT_3D('',#49047,#22612,#22613);
#18564=AXIS2_PLACEMENT_3D('',#49485,#22616,#22617);
#18565=AXIS2_PLACEMENT_3D('',#49487,#22619,#22620);
#18566=AXIS2_PLACEMENT_3D('',#49489,#22621,#22622);
#18567=AXIS2_PLACEMENT_3D('',#49927,#22625,#22626);
#18568=AXIS2_PLACEMENT_3D('',#49929,#22628,#22629);
#18569=AXIS2_PLACEMENT_3D('',#49931,#22630,#22631);
#18570=AXIS2_PLACEMENT_3D('',#50369,#22634,#22635);
#18571=AXIS2_PLACEMENT_3D('',#50371,#22637,#22638);
#18572=AXIS2_PLACEMENT_3D('',#50373,#22639,#22640);
#18573=AXIS2_PLACEMENT_3D('',#50811,#22643,#22644);
#18574=AXIS2_PLACEMENT_3D('',#50813,#22646,#22647);
#18575=AXIS2_PLACEMENT_3D('',#50815,#22648,#22649);
#18576=AXIS2_PLACEMENT_3D('',#51253,#22652,#22653);
#18577=AXIS2_PLACEMENT_3D('',#51255,#22655,#22656);
#18578=AXIS2_PLACEMENT_3D('',#51257,#22657,#22658);
#18579=AXIS2_PLACEMENT_3D('',#51695,#22661,#22662);
#18580=AXIS2_PLACEMENT_3D('',#51697,#22664,#22665);
#18581=AXIS2_PLACEMENT_3D('',#51699,#22666,#22667);
#18582=AXIS2_PLACEMENT_3D('',#52137,#22670,#22671);
#18583=AXIS2_PLACEMENT_3D('',#52139,#22673,#22674);
#18584=AXIS2_PLACEMENT_3D('',#52141,#22675,#22676);
#18585=AXIS2_PLACEMENT_3D('',#52579,#22679,#22680);
#18586=AXIS2_PLACEMENT_3D('',#52581,#22682,#22683);
#18587=AXIS2_PLACEMENT_3D('',#52583,#22684,#22685);
#18588=AXIS2_PLACEMENT_3D('',#53021,#22688,#22689);
#18589=AXIS2_PLACEMENT_3D('',#53023,#22691,#22692);
#18590=AXIS2_PLACEMENT_3D('',#53025,#22693,#22694);
#18591=AXIS2_PLACEMENT_3D('',#53463,#22697,#22698);
#18592=AXIS2_PLACEMENT_3D('',#53465,#22700,#22701);
#18593=AXIS2_PLACEMENT_3D('',#53467,#22702,#22703);
#18594=AXIS2_PLACEMENT_3D('',#53905,#22706,#22707);
#18595=AXIS2_PLACEMENT_3D('',#53907,#22709,#22710);
#18596=AXIS2_PLACEMENT_3D('',#53909,#22711,#22712);
#18597=AXIS2_PLACEMENT_3D('',#54347,#22715,#22716);
#18598=AXIS2_PLACEMENT_3D('',#54349,#22718,#22719);
#18599=AXIS2_PLACEMENT_3D('',#54351,#22720,#22721);
#18600=AXIS2_PLACEMENT_3D('',#54789,#22724,#22725);
#18601=AXIS2_PLACEMENT_3D('',#54791,#22727,#22728);
#18602=AXIS2_PLACEMENT_3D('',#54793,#22729,#22730);
#18603=AXIS2_PLACEMENT_3D('',#55231,#22733,#22734);
#18604=AXIS2_PLACEMENT_3D('',#55233,#22736,#22737);
#18605=AXIS2_PLACEMENT_3D('',#55235,#22738,#22739);
#18606=AXIS2_PLACEMENT_3D('',#55673,#22742,#22743);
#18607=AXIS2_PLACEMENT_3D('',#55675,#22745,#22746);
#18608=AXIS2_PLACEMENT_3D('',#55677,#22747,#22748);
#18609=AXIS2_PLACEMENT_3D('',#56115,#22751,#22752);
#18610=AXIS2_PLACEMENT_3D('',#56117,#22754,#22755);
#18611=AXIS2_PLACEMENT_3D('',#56119,#22756,#22757);
#18612=AXIS2_PLACEMENT_3D('',#56557,#22760,#22761);
#18613=AXIS2_PLACEMENT_3D('',#56559,#22763,#22764);
#18614=AXIS2_PLACEMENT_3D('',#56561,#22765,#22766);
#18615=AXIS2_PLACEMENT_3D('',#56999,#22769,#22770);
#18616=AXIS2_PLACEMENT_3D('',#57001,#22772,#22773);
#18617=AXIS2_PLACEMENT_3D('',#57003,#22774,#22775);
#18618=AXIS2_PLACEMENT_3D('',#57441,#22778,#22779);
#18619=AXIS2_PLACEMENT_3D('',#57443,#22781,#22782);
#18620=AXIS2_PLACEMENT_3D('',#57445,#22783,#22784);
#18621=AXIS2_PLACEMENT_3D('',#57883,#22787,#22788);
#18622=AXIS2_PLACEMENT_3D('',#57885,#22790,#22791);
#18623=AXIS2_PLACEMENT_3D('',#57887,#22792,#22793);
#18624=AXIS2_PLACEMENT_3D('',#58325,#22796,#22797);
#18625=AXIS2_PLACEMENT_3D('',#58327,#22799,#22800);
#18626=AXIS2_PLACEMENT_3D('',#58329,#22801,#22802);
#18627=AXIS2_PLACEMENT_3D('',#58767,#22805,#22806);
#18628=AXIS2_PLACEMENT_3D('',#58769,#22808,#22809);
#18629=AXIS2_PLACEMENT_3D('',#58771,#22810,#22811);
#18630=AXIS2_PLACEMENT_3D('',#59209,#22814,#22815);
#18631=AXIS2_PLACEMENT_3D('',#59211,#22817,#22818);
#18632=AXIS2_PLACEMENT_3D('',#59213,#22819,#22820);
#18633=AXIS2_PLACEMENT_3D('',#59651,#22823,#22824);
#18634=AXIS2_PLACEMENT_3D('',#59653,#22826,#22827);
#18635=AXIS2_PLACEMENT_3D('',#59655,#22828,#22829);
#18636=AXIS2_PLACEMENT_3D('',#60093,#22832,#22833);
#18637=AXIS2_PLACEMENT_3D('',#60095,#22835,#22836);
#18638=AXIS2_PLACEMENT_3D('',#60097,#22837,#22838);
#18639=AXIS2_PLACEMENT_3D('',#60535,#22841,#22842);
#18640=AXIS2_PLACEMENT_3D('',#60537,#22844,#22845);
#18641=AXIS2_PLACEMENT_3D('',#60539,#22846,#22847);
#18642=AXIS2_PLACEMENT_3D('',#60977,#22850,#22851);
#18643=AXIS2_PLACEMENT_3D('',#60979,#22853,#22854);
#18644=AXIS2_PLACEMENT_3D('',#60981,#22855,#22856);
#18645=AXIS2_PLACEMENT_3D('',#61419,#22859,#22860);
#18646=AXIS2_PLACEMENT_3D('',#61421,#22862,#22863);
#18647=AXIS2_PLACEMENT_3D('',#61423,#22864,#22865);
#18648=AXIS2_PLACEMENT_3D('',#61642,#22867,#22868);
#18649=AXIS2_PLACEMENT_3D('',#61863,#22871,#22872);
#18650=AXIS2_PLACEMENT_3D('',#61865,#22873,#22874);
#18651=AXIS2_PLACEMENT_3D('',#62303,#22877,#22878);
#18652=AXIS2_PLACEMENT_3D('',#62305,#22880,#22881);
#18653=AXIS2_PLACEMENT_3D('',#62306,#22882,#22883);
#18654=AXIS2_PLACEMENT_3D('',#62307,#22884,#22885);
#18655=AXIS2_PLACEMENT_3D('',#62308,#22886,#22887);
#18656=AXIS2_PLACEMENT_3D('',#62309,#22888,#22889);
#18657=AXIS2_PLACEMENT_3D('',#62326,#22898,#22899);
#18658=AXIS2_PLACEMENT_3D('',#62332,#22903,#22904);
#18659=AXIS2_PLACEMENT_3D('',#62336,#22907,#22908);
#18660=AXIS2_PLACEMENT_3D('',#62340,#22911,#22912);
#18661=AXIS2_PLACEMENT_3D('',#62344,#22915,#22916);
#18662=AXIS2_PLACEMENT_3D('',#62352,#22921,#22922);
#18663=AXIS2_PLACEMENT_3D('',#62354,#22924,#22925);
#18664=AXIS2_PLACEMENT_3D('',#62356,#22927,#22928);
#18665=AXIS2_PLACEMENT_3D('',#62358,#22930,#22931);
#18666=AXIS2_PLACEMENT_3D('',#62359,#22932,#22933);
#18667=AXIS2_PLACEMENT_3D('',#62360,#22934,#22935);
#18668=AXIS2_PLACEMENT_3D('',#62369,#22940,#22941);
#18669=AXIS2_PLACEMENT_3D('',#62375,#22945,#22946);
#18670=AXIS2_PLACEMENT_3D('',#62381,#22950,#22951);
#18671=AXIS2_PLACEMENT_3D('',#62387,#22955,#22956);
#18672=AXIS2_PLACEMENT_3D('',#62393,#22960,#22961);
#18673=AXIS2_PLACEMENT_3D('',#62396,#22964,#22965);
#18674=AXIS2_PLACEMENT_3D('',#62397,#22966,#22967);
#18675=AXIS2_PLACEMENT_3D('',#62399,#22968,#22969);
#18676=AXIS2_PLACEMENT_3D('',#62400,#22970,#22971);
#18677=AXIS2_PLACEMENT_3D('',#62402,#22972,#22973);
#18678=AXIS2_PLACEMENT_3D('',#62404,#22975,#22976);
#18679=AXIS2_PLACEMENT_3D('',#62406,#22977,#22978);
#18680=AXIS2_PLACEMENT_3D('',#62408,#22980,#22981);
#18681=AXIS2_PLACEMENT_3D('',#62410,#22982,#22983);
#18682=AXIS2_PLACEMENT_3D('',#62412,#22985,#22986);
#18683=AXIS2_PLACEMENT_3D('',#62413,#22987,#22988);
#18684=AXIS2_PLACEMENT_3D('',#62414,#22989,#22990);
#18685=AXIS2_PLACEMENT_3D('',#62416,#22991,#22992);
#18686=AXIS2_PLACEMENT_3D('',#62417,#22993,#22994);
#18687=AXIS2_PLACEMENT_3D('',#62419,#22995,#22996);
#18688=AXIS2_PLACEMENT_3D('',#62421,#22998,#22999);
#18689=AXIS2_PLACEMENT_3D('',#62423,#23000,#23001);
#18690=AXIS2_PLACEMENT_3D('',#62425,#23003,#23004);
#18691=AXIS2_PLACEMENT_3D('',#62427,#23005,#23006);
#18692=AXIS2_PLACEMENT_3D('',#62429,#23008,#23009);
#18693=AXIS2_PLACEMENT_3D('',#62431,#23010,#23011);
#18694=AXIS2_PLACEMENT_3D('',#62432,#23012,#23013);
#18695=AXIS2_PLACEMENT_3D('',#62434,#23014,#23015);
#18696=AXIS2_PLACEMENT_3D('',#62436,#23017,#23018);
#18697=AXIS2_PLACEMENT_3D('',#62438,#23019,#23020);
#18698=AXIS2_PLACEMENT_3D('',#62440,#23022,#23023);
#18699=AXIS2_PLACEMENT_3D('',#62442,#23024,#23025);
#18700=AXIS2_PLACEMENT_3D('',#62444,#23027,#23028);
#18701=AXIS2_PLACEMENT_3D('',#62445,#23029,#23030);
#18702=AXIS2_PLACEMENT_3D('',#62454,#23035,#23036);
#18703=AXIS2_PLACEMENT_3D('',#62460,#23040,#23041);
#18704=AXIS2_PLACEMENT_3D('',#62466,#23045,#23046);
#18705=AXIS2_PLACEMENT_3D('',#62472,#23050,#23051);
#18706=AXIS2_PLACEMENT_3D('',#62478,#23055,#23056);
#18707=AXIS2_PLACEMENT_3D('',#62481,#23059,#23060);
#18708=AXIS2_PLACEMENT_3D('',#62482,#23061,#23062);
#18709=AXIS2_PLACEMENT_3D('',#62483,#23063,#23064);
#18710=AXIS2_PLACEMENT_3D('',#62484,#23065,#23066);
#18711=AXIS2_PLACEMENT_3D('',#62485,#23067,#23068);
#18712=AXIS2_PLACEMENT_3D('',#62486,#23069,#23070);
#18713=AXIS2_PLACEMENT_3D('',#62487,#23071,#23072);
#18714=AXIS2_PLACEMENT_3D('',#62488,#23073,#23074);
#18715=AXIS2_PLACEMENT_3D('',#62489,#23075,#23076);
#18716=AXIS2_PLACEMENT_3D('',#62490,#23077,#23078);
#18717=AXIS2_PLACEMENT_3D('',#62491,#23079,#23080);
#18718=AXIS2_PLACEMENT_3D('',#62492,#23081,#23082);
#18719=AXIS2_PLACEMENT_3D('',#62493,#23083,#23084);
#18720=AXIS2_PLACEMENT_3D('',#62494,#23085,#23086);
#18721=AXIS2_PLACEMENT_3D('',#62495,#23087,#23088);
#18722=AXIS2_PLACEMENT_3D('',#62496,#23089,#23090);
#18723=AXIS2_PLACEMENT_3D('',#62497,#23091,#23092);
#18724=AXIS2_PLACEMENT_3D('',#62498,#23093,#23094);
#18725=AXIS2_PLACEMENT_3D('',#62499,#23095,#23096);
#18726=AXIS2_PLACEMENT_3D('',#62500,#23097,#23098);
#18727=AXIS2_PLACEMENT_3D('',#62501,#23099,#23100);
#18728=AXIS2_PLACEMENT_3D('',#62502,#23101,#23102);
#18729=AXIS2_PLACEMENT_3D('',#62503,#23103,#23104);
#18730=AXIS2_PLACEMENT_3D('',#62504,#23105,#23106);
#18731=AXIS2_PLACEMENT_3D('',#62505,#23107,#23108);
#18732=AXIS2_PLACEMENT_3D('',#62506,#23109,#23110);
#18733=AXIS2_PLACEMENT_3D('',#62507,#23111,#23112);
#18734=AXIS2_PLACEMENT_3D('',#62508,#23113,#23114);
#18735=AXIS2_PLACEMENT_3D('',#62509,#23115,#23116);
#18736=AXIS2_PLACEMENT_3D('',#62510,#23117,#23118);
#18737=AXIS2_PLACEMENT_3D('',#62511,#23119,#23120);
#18738=AXIS2_PLACEMENT_3D('',#62512,#23121,#23122);
#18739=AXIS2_PLACEMENT_3D('',#62513,#23123,#23124);
#18740=AXIS2_PLACEMENT_3D('',#62514,#23125,#23126);
#18741=AXIS2_PLACEMENT_3D('',#62515,#23127,#23128);
#18742=AXIS2_PLACEMENT_3D('',#62516,#23129,#23130);
#18743=AXIS2_PLACEMENT_3D('',#62517,#23131,#23132);
#18744=AXIS2_PLACEMENT_3D('',#62518,#23133,#23134);
#18745=AXIS2_PLACEMENT_3D('',#62519,#23135,#23136);
#18746=AXIS2_PLACEMENT_3D('',#62520,#23137,#23138);
#18747=AXIS2_PLACEMENT_3D('',#62521,#23139,#23140);
#18748=AXIS2_PLACEMENT_3D('',#62522,#23141,#23142);
#18749=AXIS2_PLACEMENT_3D('',#62523,#23143,#23144);
#18750=AXIS2_PLACEMENT_3D('',#62524,#23145,#23146);
#18751=AXIS2_PLACEMENT_3D('',#62525,#23147,#23148);
#18752=AXIS2_PLACEMENT_3D('',#62526,#23149,#23150);
#18753=AXIS2_PLACEMENT_3D('',#62527,#23151,#23152);
#18754=AXIS2_PLACEMENT_3D('',#62528,#23153,#23154);
#18755=AXIS2_PLACEMENT_3D('',#62529,#23155,#23156);
#18756=AXIS2_PLACEMENT_3D('',#62530,#23157,#23158);
#18757=AXIS2_PLACEMENT_3D('',#62531,#23159,#23160);
#18758=AXIS2_PLACEMENT_3D('',#62532,#23161,#23162);
#18759=AXIS2_PLACEMENT_3D('',#62533,#23163,#23164);
#18760=AXIS2_PLACEMENT_3D('',#62534,#23165,#23166);
#18761=AXIS2_PLACEMENT_3D('',#62535,#23167,#23168);
#18762=AXIS2_PLACEMENT_3D('',#62536,#23169,#23170);
#18763=AXIS2_PLACEMENT_3D('',#62537,#23171,#23172);
#18764=AXIS2_PLACEMENT_3D('',#62538,#23173,#23174);
#18765=AXIS2_PLACEMENT_3D('',#62539,#23175,#23176);
#18766=AXIS2_PLACEMENT_3D('',#62540,#23177,#23178);
#18767=AXIS2_PLACEMENT_3D('',#62541,#23179,#23180);
#18768=AXIS2_PLACEMENT_3D('',#62542,#23181,#23182);
#18769=AXIS2_PLACEMENT_3D('',#62543,#23183,#23184);
#18770=AXIS2_PLACEMENT_3D('',#62544,#23185,#23186);
#18771=AXIS2_PLACEMENT_3D('',#62545,#23187,#23188);
#18772=AXIS2_PLACEMENT_3D('',#62546,#23189,#23190);
#18773=AXIS2_PLACEMENT_3D('',#62547,#23191,#23192);
#18774=AXIS2_PLACEMENT_3D('',#62548,#23193,#23194);
#18775=AXIS2_PLACEMENT_3D('',#62549,#23195,#23196);
#18776=AXIS2_PLACEMENT_3D('',#62550,#23197,#23198);
#18777=AXIS2_PLACEMENT_3D('',#62551,#23199,#23200);
#18778=AXIS2_PLACEMENT_3D('',#62552,#23201,#23202);
#18779=AXIS2_PLACEMENT_3D('',#62553,#23203,#23204);
#18780=AXIS2_PLACEMENT_3D('',#62554,#23205,#23206);
#18781=AXIS2_PLACEMENT_3D('',#62555,#23207,#23208);
#18782=AXIS2_PLACEMENT_3D('',#62556,#23209,#23210);
#18783=AXIS2_PLACEMENT_3D('',#62557,#23211,#23212);
#18784=AXIS2_PLACEMENT_3D('',#62558,#23213,#23214);
#18785=AXIS2_PLACEMENT_3D('',#62559,#23215,#23216);
#18786=AXIS2_PLACEMENT_3D('',#62560,#23217,#23218);
#18787=AXIS2_PLACEMENT_3D('',#62561,#23219,#23220);
#18788=AXIS2_PLACEMENT_3D('',#62562,#23221,#23222);
#18789=AXIS2_PLACEMENT_3D('',#62563,#23223,#23224);
#18790=AXIS2_PLACEMENT_3D('',#62564,#23225,#23226);
#18791=AXIS2_PLACEMENT_3D('',#62565,#23227,#23228);
#18792=AXIS2_PLACEMENT_3D('',#62566,#23229,#23230);
#18793=AXIS2_PLACEMENT_3D('',#62567,#23231,#23232);
#18794=AXIS2_PLACEMENT_3D('',#62568,#23233,#23234);
#18795=AXIS2_PLACEMENT_3D('',#62569,#23235,#23236);
#18796=AXIS2_PLACEMENT_3D('',#62570,#23237,#23238);
#18797=AXIS2_PLACEMENT_3D('',#62571,#23239,#23240);
#18798=AXIS2_PLACEMENT_3D('',#62572,#23241,#23242);
#18799=AXIS2_PLACEMENT_3D('',#62573,#23243,#23244);
#18800=AXIS2_PLACEMENT_3D('',#62574,#23245,#23246);
#18801=AXIS2_PLACEMENT_3D('',#62575,#23247,#23248);
#18802=AXIS2_PLACEMENT_3D('',#62576,#23249,#23250);
#18803=AXIS2_PLACEMENT_3D('',#62577,#23251,#23252);
#18804=AXIS2_PLACEMENT_3D('',#62578,#23253,#23254);
#18805=AXIS2_PLACEMENT_3D('',#62579,#23255,#23256);
#18806=AXIS2_PLACEMENT_3D('',#62580,#23257,#23258);
#18807=AXIS2_PLACEMENT_3D('',#62581,#23259,#23260);
#18808=AXIS2_PLACEMENT_3D('',#62582,#23261,#23262);
#18809=AXIS2_PLACEMENT_3D('',#62583,#23263,#23264);
#18810=AXIS2_PLACEMENT_3D('',#62584,#23265,#23266);
#18811=AXIS2_PLACEMENT_3D('',#62585,#23267,#23268);
#18812=AXIS2_PLACEMENT_3D('',#62586,#23269,#23270);
#18813=AXIS2_PLACEMENT_3D('',#62587,#23271,#23272);
#18814=AXIS2_PLACEMENT_3D('',#62588,#23273,#23274);
#18815=AXIS2_PLACEMENT_3D('',#62589,#23275,#23276);
#18816=AXIS2_PLACEMENT_3D('',#62590,#23277,#23278);
#18817=AXIS2_PLACEMENT_3D('',#62592,#23279,#23280);
#18818=AXIS2_PLACEMENT_3D('',#62595,#23282,#23283);
#18819=AXIS2_PLACEMENT_3D('',#62596,#23284,#23285);
#18820=AXIS2_PLACEMENT_3D('',#62598,#23286,#23287);
#18821=AXIS2_PLACEMENT_3D('',#62601,#23289,#23290);
#18822=AXIS2_PLACEMENT_3D('',#62602,#23291,#23292);
#18823=AXIS2_PLACEMENT_3D('',#62603,#23293,#23294);
#18824=AXIS2_PLACEMENT_3D('',#62604,#23295,#23296);
#18825=AXIS2_PLACEMENT_3D('',#62605,#23297,#23298);
#18826=AXIS2_PLACEMENT_3D('',#62606,#23299,#23300);
#18827=AXIS2_PLACEMENT_3D('',#62607,#23301,#23302);
#18828=AXIS2_PLACEMENT_3D('',#62608,#23303,#23304);
#18829=AXIS2_PLACEMENT_3D('',#62609,#23305,#23306);
#18830=AXIS2_PLACEMENT_3D('',#62610,#23307,#23308);
#18831=DIRECTION('axis',(0.,0.,1.));
#18832=DIRECTION('refdir',(1.,0.,0.));
#18833=DIRECTION('axis',(0.,0.,1.));
#18834=DIRECTION('refdir',(1.,0.,0.));
#18835=DIRECTION('axis',(0.,0.,1.));
#18836=DIRECTION('refdir',(1.,0.,0.));
#18837=DIRECTION('center_axis',(0.,0.,1.));
#18838=DIRECTION('ref_axis',(1.,0.,0.));
#18839=DIRECTION('center_axis',(0.,0.,1.));
#18840=DIRECTION('ref_axis',(1.,0.,0.));
#18841=DIRECTION('',(0.,0.,1.));
#18842=DIRECTION('center_axis',(0.,0.,-1.));
#18843=DIRECTION('ref_axis',(1.,0.,0.));
#18844=DIRECTION('center_axis',(0.,0.,1.));
#18845=DIRECTION('ref_axis',(1.,0.,0.));
#18846=DIRECTION('center_axis',(0.,0.,1.));
#18847=DIRECTION('ref_axis',(1.,0.,0.));
#18848=DIRECTION('',(0.,0.,1.));
#18849=DIRECTION('center_axis',(0.,0.,-1.));
#18850=DIRECTION('ref_axis',(1.,0.,0.));
#18851=DIRECTION('center_axis',(0.,0.,1.));
#18852=DIRECTION('ref_axis',(1.,0.,0.));
#18853=DIRECTION('center_axis',(0.,0.,1.));
#18854=DIRECTION('ref_axis',(1.,0.,0.));
#18855=DIRECTION('',(0.,0.,1.));
#18856=DIRECTION('center_axis',(0.,0.,-1.));
#18857=DIRECTION('ref_axis',(1.,0.,0.));
#18858=DIRECTION('center_axis',(0.,1.,0.));
#18859=DIRECTION('ref_axis',(-1.,0.,0.));
#18860=DIRECTION('',(-1.,0.,0.));
#18861=DIRECTION('',(0.,0.,1.));
#18862=DIRECTION('',(-1.,0.,0.));
#18863=DIRECTION('',(0.,0.,1.));
#18864=DIRECTION('center_axis',(1.,0.,0.));
#18865=DIRECTION('ref_axis',(0.,1.,0.));
#18866=DIRECTION('',(0.,1.,0.));
#18867=DIRECTION('',(0.,1.,0.));
#18868=DIRECTION('',(0.,0.,1.));
#18869=DIRECTION('center_axis',(0.,-1.,0.));
#18870=DIRECTION('ref_axis',(1.,0.,0.));
#18871=DIRECTION('',(1.,0.,0.));
#18872=DIRECTION('',(1.,0.,0.));
#18873=DIRECTION('',(0.,0.,1.));
#18874=DIRECTION('center_axis',(-1.,0.,0.));
#18875=DIRECTION('ref_axis',(0.,-1.,0.));
#18876=DIRECTION('',(0.,-1.,0.));
#18877=DIRECTION('',(0.,-1.,0.));
#18878=DIRECTION('center_axis',(0.,0.,1.));
#18879=DIRECTION('ref_axis',(1.,0.,0.));
#18880=DIRECTION('center_axis',(0.,0.,1.));
#18881=DIRECTION('ref_axis',(1.,0.,0.));
#18882=DIRECTION('axis',(0.,0.,1.));
#18883=DIRECTION('refdir',(1.,0.,0.));
#18884=DIRECTION('center_axis',(0.,1.,0.));
#18885=DIRECTION('ref_axis',(1.,0.,0.));
#18886=DIRECTION('center_axis',(0.,1.,0.));
#18887=DIRECTION('ref_axis',(1.,0.,0.));
#18888=DIRECTION('',(0.,1.,0.));
#18889=DIRECTION('center_axis',(0.,-1.,0.));
#18890=DIRECTION('ref_axis',(1.,0.,0.));
#18891=DIRECTION('center_axis',(0.,1.,0.));
#18892=DIRECTION('ref_axis',(1.,0.,0.));
#18893=DIRECTION('center_axis',(0.,1.,0.));
#18894=DIRECTION('ref_axis',(1.,0.,0.));
#18895=DIRECTION('',(0.,1.,0.));
#18896=DIRECTION('center_axis',(0.,-1.,0.));
#18897=DIRECTION('ref_axis',(1.,0.,0.));
#18898=DIRECTION('center_axis',(0.,1.,0.));
#18899=DIRECTION('ref_axis',(1.,0.,0.));
#18900=DIRECTION('center_axis',(0.,1.,0.));
#18901=DIRECTION('ref_axis',(1.,0.,0.));
#18902=DIRECTION('',(0.,1.,0.));
#18903=DIRECTION('center_axis',(0.,-1.,0.));
#18904=DIRECTION('ref_axis',(1.,0.,0.));
#18905=DIRECTION('center_axis',(0.,1.,0.));
#18906=DIRECTION('ref_axis',(1.,0.,0.));
#18907=DIRECTION('center_axis',(0.,1.,0.));
#18908=DIRECTION('ref_axis',(1.,0.,0.));
#18909=DIRECTION('',(0.,1.,0.));
#18910=DIRECTION('center_axis',(0.,-1.,0.));
#18911=DIRECTION('ref_axis',(1.,0.,0.));
#18912=DIRECTION('center_axis',(0.,1.,0.));
#18913=DIRECTION('ref_axis',(1.,0.,0.));
#18914=DIRECTION('center_axis',(0.,1.,0.));
#18915=DIRECTION('ref_axis',(1.,0.,0.));
#18916=DIRECTION('',(0.,1.,0.));
#18917=DIRECTION('center_axis',(0.,-1.,0.));
#18918=DIRECTION('ref_axis',(1.,0.,0.));
#18919=DIRECTION('center_axis',(0.,1.,0.));
#18920=DIRECTION('ref_axis',(1.,0.,0.));
#18921=DIRECTION('center_axis',(0.,1.,0.));
#18922=DIRECTION('ref_axis',(1.,0.,0.));
#18923=DIRECTION('',(0.,1.,0.));
#18924=DIRECTION('center_axis',(0.,-1.,0.));
#18925=DIRECTION('ref_axis',(1.,0.,0.));
#18926=DIRECTION('center_axis',(0.,1.,0.));
#18927=DIRECTION('ref_axis',(1.,0.,0.));
#18928=DIRECTION('center_axis',(0.,1.,0.));
#18929=DIRECTION('ref_axis',(1.,0.,0.));
#18930=DIRECTION('',(0.,1.,0.));
#18931=DIRECTION('center_axis',(0.,-1.,0.));
#18932=DIRECTION('ref_axis',(1.,0.,0.));
#18933=DIRECTION('center_axis',(0.,1.,0.));
#18934=DIRECTION('ref_axis',(1.,0.,0.));
#18935=DIRECTION('center_axis',(0.,1.,0.));
#18936=DIRECTION('ref_axis',(1.,0.,0.));
#18937=DIRECTION('',(0.,1.,0.));
#18938=DIRECTION('center_axis',(0.,-1.,0.));
#18939=DIRECTION('ref_axis',(1.,0.,0.));
#18940=DIRECTION('center_axis',(0.,1.,0.));
#18941=DIRECTION('ref_axis',(1.,0.,0.));
#18942=DIRECTION('center_axis',(0.,1.,0.));
#18943=DIRECTION('ref_axis',(1.,0.,0.));
#18944=DIRECTION('',(0.,1.,0.));
#18945=DIRECTION('center_axis',(0.,-1.,0.));
#18946=DIRECTION('ref_axis',(1.,0.,0.));
#18947=DIRECTION('center_axis',(0.,1.,0.));
#18948=DIRECTION('ref_axis',(1.,0.,0.));
#18949=DIRECTION('center_axis',(0.,1.,0.));
#18950=DIRECTION('ref_axis',(1.,0.,0.));
#18951=DIRECTION('',(0.,1.,0.));
#18952=DIRECTION('center_axis',(0.,-1.,0.));
#18953=DIRECTION('ref_axis',(1.,0.,0.));
#18954=DIRECTION('center_axis',(0.,1.,0.));
#18955=DIRECTION('ref_axis',(1.,0.,0.));
#18956=DIRECTION('center_axis',(0.,1.,0.));
#18957=DIRECTION('ref_axis',(1.,0.,0.));
#18958=DIRECTION('',(0.,1.,0.));
#18959=DIRECTION('center_axis',(0.,-1.,0.));
#18960=DIRECTION('ref_axis',(1.,0.,0.));
#18961=DIRECTION('center_axis',(0.,1.,0.));
#18962=DIRECTION('ref_axis',(1.,0.,0.));
#18963=DIRECTION('center_axis',(0.,1.,0.));
#18964=DIRECTION('ref_axis',(1.,0.,0.));
#18965=DIRECTION('',(0.,1.,0.));
#18966=DIRECTION('center_axis',(0.,-1.,0.));
#18967=DIRECTION('ref_axis',(1.,0.,0.));
#18968=DIRECTION('center_axis',(0.,1.,0.));
#18969=DIRECTION('ref_axis',(1.,0.,0.));
#18970=DIRECTION('center_axis',(0.,1.,0.));
#18971=DIRECTION('ref_axis',(1.,0.,0.));
#18972=DIRECTION('',(0.,1.,0.));
#18973=DIRECTION('center_axis',(0.,-1.,0.));
#18974=DIRECTION('ref_axis',(1.,0.,0.));
#18975=DIRECTION('center_axis',(0.,1.,0.));
#18976=DIRECTION('ref_axis',(1.,0.,0.));
#18977=DIRECTION('center_axis',(0.,1.,0.));
#18978=DIRECTION('ref_axis',(1.,0.,0.));
#18979=DIRECTION('',(0.,1.,0.));
#18980=DIRECTION('center_axis',(0.,-1.,0.));
#18981=DIRECTION('ref_axis',(1.,0.,0.));
#18982=DIRECTION('center_axis',(0.,1.,0.));
#18983=DIRECTION('ref_axis',(1.,0.,0.));
#18984=DIRECTION('center_axis',(0.,1.,0.));
#18985=DIRECTION('ref_axis',(1.,0.,0.));
#18986=DIRECTION('',(0.,1.,0.));
#18987=DIRECTION('center_axis',(0.,-1.,0.));
#18988=DIRECTION('ref_axis',(1.,0.,0.));
#18989=DIRECTION('center_axis',(0.,1.,0.));
#18990=DIRECTION('ref_axis',(1.,0.,0.));
#18991=DIRECTION('center_axis',(0.,1.,0.));
#18992=DIRECTION('ref_axis',(1.,0.,0.));
#18993=DIRECTION('',(0.,1.,0.));
#18994=DIRECTION('center_axis',(0.,-1.,0.));
#18995=DIRECTION('ref_axis',(1.,0.,0.));
#18996=DIRECTION('center_axis',(0.,1.,0.));
#18997=DIRECTION('ref_axis',(1.,0.,0.));
#18998=DIRECTION('center_axis',(0.,1.,0.));
#18999=DIRECTION('ref_axis',(1.,0.,0.));
#19000=DIRECTION('',(0.,1.,0.));
#19001=DIRECTION('center_axis',(0.,-1.,0.));
#19002=DIRECTION('ref_axis',(1.,0.,0.));
#19003=DIRECTION('center_axis',(0.,1.,0.));
#19004=DIRECTION('ref_axis',(1.,0.,0.));
#19005=DIRECTION('center_axis',(0.,1.,0.));
#19006=DIRECTION('ref_axis',(1.,0.,0.));
#19007=DIRECTION('',(0.,1.,0.));
#19008=DIRECTION('center_axis',(0.,-1.,0.));
#19009=DIRECTION('ref_axis',(1.,0.,0.));
#19010=DIRECTION('center_axis',(0.,1.,0.));
#19011=DIRECTION('ref_axis',(1.,0.,0.));
#19012=DIRECTION('center_axis',(0.,1.,0.));
#19013=DIRECTION('ref_axis',(1.,0.,0.));
#19014=DIRECTION('',(0.,1.,0.));
#19015=DIRECTION('center_axis',(0.,-1.,0.));
#19016=DIRECTION('ref_axis',(1.,0.,0.));
#19017=DIRECTION('center_axis',(0.,1.,0.));
#19018=DIRECTION('ref_axis',(1.,0.,0.));
#19019=DIRECTION('center_axis',(0.,1.,0.));
#19020=DIRECTION('ref_axis',(1.,0.,0.));
#19021=DIRECTION('',(0.,1.,0.));
#19022=DIRECTION('center_axis',(0.,-1.,0.));
#19023=DIRECTION('ref_axis',(1.,0.,0.));
#19024=DIRECTION('center_axis',(0.,1.,0.));
#19025=DIRECTION('ref_axis',(1.,0.,0.));
#19026=DIRECTION('center_axis',(0.,1.,0.));
#19027=DIRECTION('ref_axis',(1.,0.,0.));
#19028=DIRECTION('',(0.,1.,0.));
#19029=DIRECTION('center_axis',(0.,-1.,0.));
#19030=DIRECTION('ref_axis',(1.,0.,0.));
#19031=DIRECTION('center_axis',(0.,1.,0.));
#19032=DIRECTION('ref_axis',(1.,0.,0.));
#19033=DIRECTION('center_axis',(0.,1.,0.));
#19034=DIRECTION('ref_axis',(1.,0.,0.));
#19035=DIRECTION('',(0.,1.,0.));
#19036=DIRECTION('center_axis',(0.,-1.,0.));
#19037=DIRECTION('ref_axis',(1.,0.,0.));
#19038=DIRECTION('center_axis',(0.,0.,1.));
#19039=DIRECTION('ref_axis',(1.,0.,0.));
#19040=DIRECTION('center_axis',(0.,0.,1.));
#19041=DIRECTION('ref_axis',(1.,0.,0.));
#19042=DIRECTION('',(0.,0.,1.));
#19043=DIRECTION('center_axis',(0.,0.,-1.));
#19044=DIRECTION('ref_axis',(1.,0.,0.));
#19045=DIRECTION('center_axis',(0.,0.,1.));
#19046=DIRECTION('ref_axis',(1.,0.,0.));
#19047=DIRECTION('center_axis',(0.,0.,1.));
#19048=DIRECTION('ref_axis',(1.,0.,0.));
#19049=DIRECTION('',(0.,0.,1.));
#19050=DIRECTION('center_axis',(0.,0.,-1.));
#19051=DIRECTION('ref_axis',(1.,0.,0.));
#19052=DIRECTION('center_axis',(0.,0.,1.));
#19053=DIRECTION('ref_axis',(1.,0.,0.));
#19054=DIRECTION('center_axis',(0.,0.,1.));
#19055=DIRECTION('ref_axis',(1.,0.,0.));
#19056=DIRECTION('',(0.,0.,1.));
#19057=DIRECTION('center_axis',(0.,0.,-1.));
#19058=DIRECTION('ref_axis',(1.,0.,0.));
#19059=DIRECTION('center_axis',(0.,0.,1.));
#19060=DIRECTION('ref_axis',(1.,0.,0.));
#19061=DIRECTION('',(-1.,0.,0.));
#19062=DIRECTION('',(0.,1.,0.));
#19063=DIRECTION('',(1.,0.,0.));
#19064=DIRECTION('',(0.,1.,0.));
#19065=DIRECTION('center_axis',(0.,1.,0.));
#19066=DIRECTION('ref_axis',(1.,0.,0.));
#19067=DIRECTION('',(0.,0.,-1.));
#19068=DIRECTION('',(1.,0.,0.));
#19069=DIRECTION('',(0.,0.,1.));
#19070=DIRECTION('center_axis',(0.,1.,0.));
#19071=DIRECTION('ref_axis',(-1.,0.,0.));
#19072=DIRECTION('',(-1.,0.,0.));
#19073=DIRECTION('',(0.,0.,1.));
#19074=DIRECTION('',(-1.,0.,0.));
#19075=DIRECTION('',(0.,0.,1.));
#19076=DIRECTION('center_axis',(1.,0.,0.));
#19077=DIRECTION('ref_axis',(0.,1.,0.));
#19078=DIRECTION('',(0.,1.,0.));
#19079=DIRECTION('',(0.,1.,0.));
#19080=DIRECTION('',(0.,0.,1.));
#19081=DIRECTION('center_axis',(0.,-1.,0.));
#19082=DIRECTION('ref_axis',(1.,0.,0.));
#19083=DIRECTION('',(1.,0.,0.));
#19084=DIRECTION('',(0.,0.,1.));
#19085=DIRECTION('center_axis',(-1.,0.,0.));
#19086=DIRECTION('ref_axis',(0.,-1.,0.));
#19087=DIRECTION('',(0.,-1.,0.));
#19088=DIRECTION('',(0.,-1.,0.));
#19089=DIRECTION('center_axis',(0.,0.,1.));
#19090=DIRECTION('ref_axis',(1.,0.,0.));
#19091=DIRECTION('center_axis',(0.,0.,1.));
#19092=DIRECTION('ref_axis',(1.,0.,0.));
#19093=DIRECTION('axis',(0.,0.,1.));
#19094=DIRECTION('refdir',(1.,0.,0.));
#19095=DIRECTION('center_axis',(0.,1.,0.));
#19096=DIRECTION('ref_axis',(1.,0.,0.));
#19097=DIRECTION('center_axis',(0.,1.,0.));
#19098=DIRECTION('ref_axis',(1.,0.,0.));
#19099=DIRECTION('',(0.,1.,0.));
#19100=DIRECTION('center_axis',(0.,-1.,0.));
#19101=DIRECTION('ref_axis',(1.,0.,0.));
#19102=DIRECTION('center_axis',(0.,1.,0.));
#19103=DIRECTION('ref_axis',(1.,0.,0.));
#19104=DIRECTION('center_axis',(0.,1.,0.));
#19105=DIRECTION('ref_axis',(1.,0.,0.));
#19106=DIRECTION('',(0.,1.,0.));
#19107=DIRECTION('center_axis',(0.,-1.,0.));
#19108=DIRECTION('ref_axis',(1.,0.,0.));
#19109=DIRECTION('center_axis',(0.,1.,0.));
#19110=DIRECTION('ref_axis',(1.,0.,0.));
#19111=DIRECTION('center_axis',(0.,1.,0.));
#19112=DIRECTION('ref_axis',(1.,0.,0.));
#19113=DIRECTION('',(0.,1.,0.));
#19114=DIRECTION('center_axis',(0.,-1.,0.));
#19115=DIRECTION('ref_axis',(1.,0.,0.));
#19116=DIRECTION('center_axis',(0.,1.,0.));
#19117=DIRECTION('ref_axis',(1.,0.,0.));
#19118=DIRECTION('center_axis',(0.,1.,0.));
#19119=DIRECTION('ref_axis',(1.,0.,0.));
#19120=DIRECTION('',(0.,1.,0.));
#19121=DIRECTION('center_axis',(0.,-1.,0.));
#19122=DIRECTION('ref_axis',(1.,0.,0.));
#19123=DIRECTION('center_axis',(0.,1.,0.));
#19124=DIRECTION('ref_axis',(1.,0.,0.));
#19125=DIRECTION('center_axis',(0.,1.,0.));
#19126=DIRECTION('ref_axis',(1.,0.,0.));
#19127=DIRECTION('',(0.,-1.,0.));
#19128=DIRECTION('center_axis',(0.,-1.,0.));
#19129=DIRECTION('ref_axis',(1.,0.,0.));
#19130=DIRECTION('center_axis',(0.,1.,0.));
#19131=DIRECTION('ref_axis',(1.,0.,0.));
#19132=DIRECTION('center_axis',(0.,-1.,0.));
#19133=DIRECTION('ref_axis',(1.,0.,0.));
#19134=DIRECTION('center_axis',(0.,1.,0.));
#19135=DIRECTION('ref_axis',(1.,0.,0.));
#19136=DIRECTION('',(0.,-1.,0.));
#19137=DIRECTION('center_axis',(0.,-1.,0.));
#19138=DIRECTION('ref_axis',(1.,0.,0.));
#19139=DIRECTION('center_axis',(0.,1.,0.));
#19140=DIRECTION('ref_axis',(1.,0.,0.));
#19141=DIRECTION('center_axis',(0.,1.,0.));
#19142=DIRECTION('ref_axis',(1.,0.,0.));
#19143=DIRECTION('',(0.,-1.,0.));
#19144=DIRECTION('center_axis',(0.,1.,0.));
#19145=DIRECTION('ref_axis',(1.,0.,0.));
#19146=DIRECTION('center_axis',(0.,1.,0.));
#19147=DIRECTION('ref_axis',(1.,0.,0.));
#19148=DIRECTION('center_axis',(0.,1.,0.));
#19149=DIRECTION('ref_axis',(1.,0.,0.));
#19150=DIRECTION('axis',(0.,0.,1.));
#19151=DIRECTION('refdir',(1.,0.,0.));
#19152=DIRECTION('center_axis',(0.,1.,0.));
#19153=DIRECTION('ref_axis',(1.,0.,0.));
#19154=DIRECTION('center_axis',(0.,1.,0.));
#19155=DIRECTION('ref_axis',(1.,0.,0.));
#19156=DIRECTION('',(0.,1.,0.));
#19157=DIRECTION('center_axis',(0.,-1.,0.));
#19158=DIRECTION('ref_axis',(1.,0.,0.));
#19159=DIRECTION('center_axis',(0.,1.,0.));
#19160=DIRECTION('ref_axis',(1.,0.,0.));
#19161=DIRECTION('center_axis',(0.,1.,0.));
#19162=DIRECTION('ref_axis',(1.,0.,0.));
#19163=DIRECTION('',(0.,1.,0.));
#19164=DIRECTION('center_axis',(0.,-1.,0.));
#19165=DIRECTION('ref_axis',(1.,0.,0.));
#19166=DIRECTION('center_axis',(0.,1.,0.));
#19167=DIRECTION('ref_axis',(1.,0.,0.));
#19168=DIRECTION('center_axis',(0.,1.,0.));
#19169=DIRECTION('ref_axis',(1.,0.,0.));
#19170=DIRECTION('',(0.,1.,0.));
#19171=DIRECTION('center_axis',(0.,-1.,0.));
#19172=DIRECTION('ref_axis',(1.,0.,0.));
#19173=DIRECTION('center_axis',(0.,1.,0.));
#19174=DIRECTION('ref_axis',(1.,0.,0.));
#19175=DIRECTION('center_axis',(0.,1.,0.));
#19176=DIRECTION('ref_axis',(1.,0.,0.));
#19177=DIRECTION('',(0.,1.,0.));
#19178=DIRECTION('center_axis',(0.,-1.,0.));
#19179=DIRECTION('ref_axis',(1.,0.,0.));
#19180=DIRECTION('center_axis',(0.,1.,0.));
#19181=DIRECTION('ref_axis',(1.,0.,0.));
#19182=DIRECTION('center_axis',(0.,1.,0.));
#19183=DIRECTION('ref_axis',(1.,0.,0.));
#19184=DIRECTION('',(0.,-1.,0.));
#19185=DIRECTION('center_axis',(0.,1.,0.));
#19186=DIRECTION('ref_axis',(1.,0.,0.));
#19187=DIRECTION('center_axis',(0.,1.,0.));
#19188=DIRECTION('ref_axis',(1.,0.,0.));
#19189=DIRECTION('center_axis',(0.,-1.,0.));
#19190=DIRECTION('ref_axis',(1.,0.,0.));
#19191=DIRECTION('center_axis',(0.,1.,0.));
#19192=DIRECTION('ref_axis',(1.,0.,0.));
#19193=DIRECTION('center_axis',(0.,-1.,0.));
#19194=DIRECTION('ref_axis',(1.,0.,0.));
#19195=DIRECTION('',(0.,-1.,0.));
#19196=DIRECTION('center_axis',(0.,1.,0.));
#19197=DIRECTION('ref_axis',(1.,0.,0.));
#19198=DIRECTION('center_axis',(0.,1.,0.));
#19199=DIRECTION('ref_axis',(1.,0.,0.));
#19200=DIRECTION('',(0.,-1.,0.));
#19201=DIRECTION('center_axis',(0.,1.,0.));
#19202=DIRECTION('ref_axis',(1.,0.,0.));
#19203=DIRECTION('center_axis',(0.,1.,0.));
#19204=DIRECTION('ref_axis',(1.,0.,0.));
#19205=DIRECTION('center_axis',(0.,1.,0.));
#19206=DIRECTION('ref_axis',(1.,0.,0.));
#19207=DIRECTION('axis',(0.,0.,1.));
#19208=DIRECTION('refdir',(1.,0.,0.));
#19209=DIRECTION('center_axis',(0.,1.,0.));
#19210=DIRECTION('ref_axis',(1.,0.,0.));
#19211=DIRECTION('center_axis',(0.,1.,0.));
#19212=DIRECTION('ref_axis',(1.,0.,0.));
#19213=DIRECTION('',(0.,1.,0.));
#19214=DIRECTION('center_axis',(0.,-1.,0.));
#19215=DIRECTION('ref_axis',(1.,0.,0.));
#19216=DIRECTION('center_axis',(0.,1.,0.));
#19217=DIRECTION('ref_axis',(1.,0.,0.));
#19218=DIRECTION('center_axis',(0.,1.,0.));
#19219=DIRECTION('ref_axis',(1.,0.,0.));
#19220=DIRECTION('',(0.,1.,0.));
#19221=DIRECTION('center_axis',(0.,-1.,0.));
#19222=DIRECTION('ref_axis',(1.,0.,0.));
#19223=DIRECTION('center_axis',(0.,1.,0.));
#19224=DIRECTION('ref_axis',(1.,0.,0.));
#19225=DIRECTION('center_axis',(0.,1.,0.));
#19226=DIRECTION('ref_axis',(1.,0.,0.));
#19227=DIRECTION('',(0.,1.,0.));
#19228=DIRECTION('center_axis',(0.,-1.,0.));
#19229=DIRECTION('ref_axis',(1.,0.,0.));
#19230=DIRECTION('center_axis',(0.,1.,0.));
#19231=DIRECTION('ref_axis',(1.,0.,0.));
#19232=DIRECTION('center_axis',(0.,1.,0.));
#19233=DIRECTION('ref_axis',(1.,0.,0.));
#19234=DIRECTION('',(0.,1.,0.));
#19235=DIRECTION('center_axis',(0.,-1.,0.));
#19236=DIRECTION('ref_axis',(1.,0.,0.));
#19237=DIRECTION('center_axis',(0.,1.,0.));
#19238=DIRECTION('ref_axis',(1.,0.,0.));
#19239=DIRECTION('center_axis',(0.,1.,0.));
#19240=DIRECTION('ref_axis',(1.,0.,0.));
#19241=DIRECTION('',(0.,-1.,0.));
#19242=DIRECTION('center_axis',(0.,-1.,0.));
#19243=DIRECTION('ref_axis',(1.,0.,0.));
#19244=DIRECTION('center_axis',(0.,1.,0.));
#19245=DIRECTION('ref_axis',(1.,0.,0.));
#19246=DIRECTION('center_axis',(0.,-1.,0.));
#19247=DIRECTION('ref_axis',(1.,0.,0.));
#19248=DIRECTION('center_axis',(0.,1.,0.));
#19249=DIRECTION('ref_axis',(1.,0.,0.));
#19250=DIRECTION('',(0.,-1.,0.));
#19251=DIRECTION('center_axis',(0.,-1.,0.));
#19252=DIRECTION('ref_axis',(1.,0.,0.));
#19253=DIRECTION('center_axis',(0.,1.,0.));
#19254=DIRECTION('ref_axis',(1.,0.,0.));
#19255=DIRECTION('center_axis',(0.,1.,0.));
#19256=DIRECTION('ref_axis',(1.,0.,0.));
#19257=DIRECTION('',(0.,-1.,0.));
#19258=DIRECTION('center_axis',(0.,1.,0.));
#19259=DIRECTION('ref_axis',(1.,0.,0.));
#19260=DIRECTION('center_axis',(0.,1.,0.));
#19261=DIRECTION('ref_axis',(1.,0.,0.));
#19262=DIRECTION('center_axis',(0.,1.,0.));
#19263=DIRECTION('ref_axis',(1.,0.,0.));
#19264=DIRECTION('axis',(0.,0.,1.));
#19265=DIRECTION('refdir',(1.,0.,0.));
#19266=DIRECTION('center_axis',(0.,1.,0.));
#19267=DIRECTION('ref_axis',(1.,0.,0.));
#19268=DIRECTION('center_axis',(0.,1.,0.));
#19269=DIRECTION('ref_axis',(1.,0.,0.));
#19270=DIRECTION('',(0.,1.,0.));
#19271=DIRECTION('center_axis',(0.,-1.,0.));
#19272=DIRECTION('ref_axis',(1.,0.,0.));
#19273=DIRECTION('center_axis',(0.,1.,0.));
#19274=DIRECTION('ref_axis',(1.,0.,0.));
#19275=DIRECTION('center_axis',(0.,1.,0.));
#19276=DIRECTION('ref_axis',(1.,0.,0.));
#19277=DIRECTION('',(0.,1.,0.));
#19278=DIRECTION('center_axis',(0.,-1.,0.));
#19279=DIRECTION('ref_axis',(1.,0.,0.));
#19280=DIRECTION('center_axis',(0.,1.,0.));
#19281=DIRECTION('ref_axis',(1.,0.,0.));
#19282=DIRECTION('center_axis',(0.,1.,0.));
#19283=DIRECTION('ref_axis',(1.,0.,0.));
#19284=DIRECTION('',(0.,1.,0.));
#19285=DIRECTION('center_axis',(0.,-1.,0.));
#19286=DIRECTION('ref_axis',(1.,0.,0.));
#19287=DIRECTION('center_axis',(0.,1.,0.));
#19288=DIRECTION('ref_axis',(1.,0.,0.));
#19289=DIRECTION('center_axis',(0.,1.,0.));
#19290=DIRECTION('ref_axis',(1.,0.,0.));
#19291=DIRECTION('',(0.,1.,0.));
#19292=DIRECTION('center_axis',(0.,-1.,0.));
#19293=DIRECTION('ref_axis',(1.,0.,0.));
#19294=DIRECTION('center_axis',(0.,1.,0.));
#19295=DIRECTION('ref_axis',(1.,0.,0.));
#19296=DIRECTION('center_axis',(0.,1.,0.));
#19297=DIRECTION('ref_axis',(1.,0.,0.));
#19298=DIRECTION('',(0.,-1.,0.));
#19299=DIRECTION('center_axis',(0.,1.,0.));
#19300=DIRECTION('ref_axis',(1.,0.,0.));
#19301=DIRECTION('center_axis',(0.,1.,0.));
#19302=DIRECTION('ref_axis',(1.,0.,0.));
#19303=DIRECTION('center_axis',(0.,-1.,0.));
#19304=DIRECTION('ref_axis',(1.,0.,0.));
#19305=DIRECTION('center_axis',(0.,1.,0.));
#19306=DIRECTION('ref_axis',(1.,0.,0.));
#19307=DIRECTION('center_axis',(0.,-1.,0.));
#19308=DIRECTION('ref_axis',(1.,0.,0.));
#19309=DIRECTION('',(0.,-1.,0.));
#19310=DIRECTION('center_axis',(0.,1.,0.));
#19311=DIRECTION('ref_axis',(1.,0.,0.));
#19312=DIRECTION('center_axis',(0.,1.,0.));
#19313=DIRECTION('ref_axis',(1.,0.,0.));
#19314=DIRECTION('',(0.,-1.,0.));
#19315=DIRECTION('center_axis',(0.,1.,0.));
#19316=DIRECTION('ref_axis',(1.,0.,0.));
#19317=DIRECTION('center_axis',(0.,1.,0.));
#19318=DIRECTION('ref_axis',(1.,0.,0.));
#19319=DIRECTION('center_axis',(0.,1.,0.));
#19320=DIRECTION('ref_axis',(1.,0.,0.));
#19321=DIRECTION('axis',(0.,0.,1.));
#19322=DIRECTION('refdir',(1.,0.,0.));
#19323=DIRECTION('center_axis',(0.866025403784439,0.,-0.5));
#19324=DIRECTION('ref_axis',(0.5,0.,0.866025403784439));
#19325=DIRECTION('',(-0.5,0.,-0.866025403784439));
#19326=DIRECTION('',(0.,-1.,0.));
#19327=DIRECTION('',(0.5,0.,0.866025403784439));
#19328=DIRECTION('',(0.,-1.,0.));
#19329=DIRECTION('center_axis',(1.92296268638356E-16,0.,-1.));
#19330=DIRECTION('ref_axis',(1.,0.,1.92296268638356E-16));
#19331=DIRECTION('',(-1.,0.,-1.92296268638356E-16));
#19332=DIRECTION('',(0.,-1.,0.));
#19333=DIRECTION('',(1.,0.,1.92296268638356E-16));
#19334=DIRECTION('center_axis',(-0.866025403784439,0.,-0.5));
#19335=DIRECTION('ref_axis',(0.5,0.,-0.866025403784439));
#19336=DIRECTION('',(-0.5,0.,0.866025403784438));
#19337=DIRECTION('',(0.,-1.,0.));
#19338=DIRECTION('',(0.5,0.,-0.866025403784438));
#19339=DIRECTION('center_axis',(-0.866025403784439,0.,0.5));
#19340=DIRECTION('ref_axis',(-0.5,0.,-0.866025403784439));
#19341=DIRECTION('',(0.5,0.,0.866025403784439));
#19342=DIRECTION('',(0.,-1.,0.));
#19343=DIRECTION('',(-0.5,0.,-0.866025403784439));
#19344=DIRECTION('center_axis',(-1.92296268638356E-16,0.,1.));
#19345=DIRECTION('ref_axis',(-1.,0.,-1.92296268638356E-16));
#19346=DIRECTION('',(1.,0.,1.92296268638356E-16));
#19347=DIRECTION('',(0.,-1.,0.));
#19348=DIRECTION('',(-1.,0.,-1.92296268638356E-16));
#19349=DIRECTION('center_axis',(0.866025403784439,0.,0.5));
#19350=DIRECTION('ref_axis',(-0.5,0.,0.866025403784439));
#19351=DIRECTION('',(0.5,0.,-0.866025403784439));
#19352=DIRECTION('',(-0.5,0.,0.866025403784439));
#19353=DIRECTION('center_axis',(0.,1.,0.));
#19354=DIRECTION('ref_axis',(1.,0.,0.));
#19355=DIRECTION('center_axis',(0.,-1.,0.));
#19356=DIRECTION('ref_axis',(0.,0.,-1.));
#19357=DIRECTION('center_axis',(0.,1.,0.));
#19358=DIRECTION('ref_axis',(1.,0.,0.));
#19359=DIRECTION('center_axis',(0.,1.,0.));
#19360=DIRECTION('ref_axis',(1.,0.,0.));
#19361=DIRECTION('center_axis',(0.,1.,0.));
#19362=DIRECTION('ref_axis',(0.,0.,1.));
#19363=DIRECTION('center_axis',(0.,-1.,0.));
#19364=DIRECTION('ref_axis',(1.,0.,0.));
#19365=DIRECTION('center_axis',(0.,-1.,0.));
#19366=DIRECTION('ref_axis',(1.,0.,0.));
#19367=DIRECTION('center_axis',(0.,-1.,0.));
#19368=DIRECTION('ref_axis',(1.,0.,0.));
#19369=DIRECTION('',(0.707106781186548,0.707106781186547,8.65956056235494E-17));
#19370=DIRECTION('center_axis',(0.,-1.,0.));
#19371=DIRECTION('ref_axis',(1.,0.,0.));
#19372=DIRECTION('center_axis',(0.,-1.,0.));
#19373=DIRECTION('ref_axis',(1.,0.,0.));
#19374=DIRECTION('',(0.,1.,0.));
#19375=DIRECTION('center_axis',(0.,1.,0.));
#19376=DIRECTION('ref_axis',(1.,0.,0.));
#19377=DIRECTION('center_axis',(0.,-1.,0.));
#19378=DIRECTION('ref_axis',(1.,0.,0.));
#19379=DIRECTION('',(-0.707106781186547,0.707106781186548,-8.65956056235493E-17));
#19380=DIRECTION('center_axis',(0.,-1.,0.));
#19381=DIRECTION('ref_axis',(0.,0.,-1.));
#19382=DIRECTION('center_axis',(0.,-1.,0.));
#19383=DIRECTION('ref_axis',(1.,0.,0.));
#19384=DIRECTION('center_axis',(0.,1.,0.));
#19385=DIRECTION('ref_axis',(1.,0.,0.));
#19386=DIRECTION('center_axis',(0.,1.,0.));
#19387=DIRECTION('ref_axis',(1.,0.,0.));
#19388=DIRECTION('',(-0.447213595499958,0.894427190999916,-5.47678698264203E-17));
#19389=DIRECTION('center_axis',(0.,-1.,0.));
#19390=DIRECTION('ref_axis',(1.,0.,0.));
#19391=DIRECTION('',(0.,1.,0.));
#19392=DIRECTION('axis',(0.,0.,1.));
#19393=DIRECTION('refdir',(1.,0.,0.));
#19394=DIRECTION('center_axis',(0.,1.,0.));
#19395=DIRECTION('ref_axis',(1.,0.,0.));
#19396=DIRECTION('center_axis',(0.,1.,0.));
#19397=DIRECTION('ref_axis',(1.,0.,0.));
#19398=DIRECTION('',(0.,1.,0.));
#19399=DIRECTION('center_axis',(0.,-1.,0.));
#19400=DIRECTION('ref_axis',(1.,0.,0.));
#19401=DIRECTION('center_axis',(0.,1.,0.));
#19402=DIRECTION('ref_axis',(1.,0.,0.));
#19403=DIRECTION('center_axis',(0.,1.,0.));
#19404=DIRECTION('ref_axis',(1.,0.,0.));
#19405=DIRECTION('',(0.,1.,0.));
#19406=DIRECTION('center_axis',(0.,-1.,0.));
#19407=DIRECTION('ref_axis',(1.,0.,0.));
#19408=DIRECTION('center_axis',(0.,1.,0.));
#19409=DIRECTION('ref_axis',(1.,0.,0.));
#19410=DIRECTION('center_axis',(0.,1.,0.));
#19411=DIRECTION('ref_axis',(1.,0.,0.));
#19412=DIRECTION('',(0.,1.,0.));
#19413=DIRECTION('center_axis',(0.,-1.,0.));
#19414=DIRECTION('ref_axis',(1.,0.,0.));
#19415=DIRECTION('center_axis',(0.,1.,0.));
#19416=DIRECTION('ref_axis',(1.,0.,0.));
#19417=DIRECTION('center_axis',(0.,1.,0.));
#19418=DIRECTION('ref_axis',(1.,0.,0.));
#19419=DIRECTION('',(0.,1.,0.));
#19420=DIRECTION('center_axis',(0.,-1.,0.));
#19421=DIRECTION('ref_axis',(1.,0.,0.));
#19422=DIRECTION('center_axis',(0.,1.,0.));
#19423=DIRECTION('ref_axis',(1.,0.,0.));
#19424=DIRECTION('center_axis',(0.,1.,0.));
#19425=DIRECTION('ref_axis',(1.,0.,0.));
#19426=DIRECTION('',(0.,-1.,0.));
#19427=DIRECTION('center_axis',(0.,-1.,0.));
#19428=DIRECTION('ref_axis',(1.,0.,0.));
#19429=DIRECTION('center_axis',(0.,1.,0.));
#19430=DIRECTION('ref_axis',(1.,0.,0.));
#19431=DIRECTION('center_axis',(0.,-1.,0.));
#19432=DIRECTION('ref_axis',(1.,0.,0.));
#19433=DIRECTION('center_axis',(0.,1.,0.));
#19434=DIRECTION('ref_axis',(1.,0.,0.));
#19435=DIRECTION('',(0.,-1.,0.));
#19436=DIRECTION('center_axis',(0.,-1.,0.));
#19437=DIRECTION('ref_axis',(1.,0.,0.));
#19438=DIRECTION('center_axis',(0.,1.,0.));
#19439=DIRECTION('ref_axis',(1.,0.,0.));
#19440=DIRECTION('center_axis',(0.,1.,0.));
#19441=DIRECTION('ref_axis',(1.,0.,0.));
#19442=DIRECTION('',(0.,-1.,0.));
#19443=DIRECTION('center_axis',(0.,1.,0.));
#19444=DIRECTION('ref_axis',(1.,0.,0.));
#19445=DIRECTION('center_axis',(0.,1.,0.));
#19446=DIRECTION('ref_axis',(1.,0.,0.));
#19447=DIRECTION('center_axis',(0.,1.,0.));
#19448=DIRECTION('ref_axis',(1.,0.,0.));
#19449=DIRECTION('axis',(0.,0.,1.));
#19450=DIRECTION('refdir',(1.,0.,0.));
#19451=DIRECTION('center_axis',(0.,1.,0.));
#19452=DIRECTION('ref_axis',(1.,0.,0.));
#19453=DIRECTION('center_axis',(0.,1.,0.));
#19454=DIRECTION('ref_axis',(1.,0.,0.));
#19455=DIRECTION('',(0.,1.,0.));
#19456=DIRECTION('center_axis',(0.,-1.,0.));
#19457=DIRECTION('ref_axis',(1.,0.,0.));
#19458=DIRECTION('center_axis',(0.,1.,0.));
#19459=DIRECTION('ref_axis',(1.,0.,0.));
#19460=DIRECTION('center_axis',(0.,1.,0.));
#19461=DIRECTION('ref_axis',(1.,0.,0.));
#19462=DIRECTION('',(0.,1.,0.));
#19463=DIRECTION('center_axis',(0.,-1.,0.));
#19464=DIRECTION('ref_axis',(1.,0.,0.));
#19465=DIRECTION('center_axis',(0.,1.,0.));
#19466=DIRECTION('ref_axis',(1.,0.,0.));
#19467=DIRECTION('center_axis',(0.,1.,0.));
#19468=DIRECTION('ref_axis',(1.,0.,0.));
#19469=DIRECTION('',(0.,1.,0.));
#19470=DIRECTION('center_axis',(0.,-1.,0.));
#19471=DIRECTION('ref_axis',(1.,0.,0.));
#19472=DIRECTION('center_axis',(0.,1.,0.));
#19473=DIRECTION('ref_axis',(1.,0.,0.));
#19474=DIRECTION('center_axis',(0.,1.,0.));
#19475=DIRECTION('ref_axis',(1.,0.,0.));
#19476=DIRECTION('',(0.,1.,0.));
#19477=DIRECTION('center_axis',(0.,-1.,0.));
#19478=DIRECTION('ref_axis',(1.,0.,0.));
#19479=DIRECTION('center_axis',(0.,1.,0.));
#19480=DIRECTION('ref_axis',(1.,0.,0.));
#19481=DIRECTION('center_axis',(0.,1.,0.));
#19482=DIRECTION('ref_axis',(1.,0.,0.));
#19483=DIRECTION('',(0.,-1.,0.));
#19484=DIRECTION('center_axis',(0.,1.,0.));
#19485=DIRECTION('ref_axis',(1.,0.,0.));
#19486=DIRECTION('center_axis',(0.,1.,0.));
#19487=DIRECTION('ref_axis',(1.,0.,0.));
#19488=DIRECTION('center_axis',(0.,-1.,0.));
#19489=DIRECTION('ref_axis',(1.,0.,0.));
#19490=DIRECTION('center_axis',(0.,1.,0.));
#19491=DIRECTION('ref_axis',(1.,0.,0.));
#19492=DIRECTION('center_axis',(0.,-1.,0.));
#19493=DIRECTION('ref_axis',(1.,0.,0.));
#19494=DIRECTION('',(0.,-1.,0.));
#19495=DIRECTION('center_axis',(0.,1.,0.));
#19496=DIRECTION('ref_axis',(1.,0.,0.));
#19497=DIRECTION('center_axis',(0.,1.,0.));
#19498=DIRECTION('ref_axis',(1.,0.,0.));
#19499=DIRECTION('',(0.,-1.,0.));
#19500=DIRECTION('center_axis',(0.,1.,0.));
#19501=DIRECTION('ref_axis',(1.,0.,0.));
#19502=DIRECTION('center_axis',(0.,1.,0.));
#19503=DIRECTION('ref_axis',(1.,0.,0.));
#19504=DIRECTION('center_axis',(0.,1.,0.));
#19505=DIRECTION('ref_axis',(1.,0.,0.));
#19506=DIRECTION('axis',(0.,0.,1.));
#19507=DIRECTION('refdir',(1.,0.,0.));
#19508=DIRECTION('center_axis',(0.,1.,0.));
#19509=DIRECTION('ref_axis',(1.,0.,0.));
#19510=DIRECTION('center_axis',(0.,1.,0.));
#19511=DIRECTION('ref_axis',(1.,0.,0.));
#19512=DIRECTION('',(0.,1.,0.));
#19513=DIRECTION('center_axis',(0.,-1.,0.));
#19514=DIRECTION('ref_axis',(1.,0.,0.));
#19515=DIRECTION('center_axis',(0.,1.,0.));
#19516=DIRECTION('ref_axis',(1.,0.,0.));
#19517=DIRECTION('center_axis',(0.,1.,0.));
#19518=DIRECTION('ref_axis',(1.,0.,0.));
#19519=DIRECTION('',(0.,1.,0.));
#19520=DIRECTION('center_axis',(0.,-1.,0.));
#19521=DIRECTION('ref_axis',(1.,0.,0.));
#19522=DIRECTION('center_axis',(0.,1.,0.));
#19523=DIRECTION('ref_axis',(1.,0.,0.));
#19524=DIRECTION('center_axis',(0.,1.,0.));
#19525=DIRECTION('ref_axis',(1.,0.,0.));
#19526=DIRECTION('',(0.,1.,0.));
#19527=DIRECTION('center_axis',(0.,-1.,0.));
#19528=DIRECTION('ref_axis',(1.,0.,0.));
#19529=DIRECTION('center_axis',(0.,1.,0.));
#19530=DIRECTION('ref_axis',(1.,0.,0.));
#19531=DIRECTION('center_axis',(0.,1.,0.));
#19532=DIRECTION('ref_axis',(1.,0.,0.));
#19533=DIRECTION('',(0.,1.,0.));
#19534=DIRECTION('center_axis',(0.,-1.,0.));
#19535=DIRECTION('ref_axis',(1.,0.,0.));
#19536=DIRECTION('center_axis',(0.,1.,0.));
#19537=DIRECTION('ref_axis',(1.,0.,0.));
#19538=DIRECTION('center_axis',(0.,1.,0.));
#19539=DIRECTION('ref_axis',(1.,0.,0.));
#19540=DIRECTION('',(0.,-1.,0.));
#19541=DIRECTION('center_axis',(0.,-1.,0.));
#19542=DIRECTION('ref_axis',(1.,0.,0.));
#19543=DIRECTION('center_axis',(0.,1.,0.));
#19544=DIRECTION('ref_axis',(1.,0.,0.));
#19545=DIRECTION('center_axis',(0.,-1.,0.));
#19546=DIRECTION('ref_axis',(1.,0.,0.));
#19547=DIRECTION('center_axis',(0.,1.,0.));
#19548=DIRECTION('ref_axis',(1.,0.,0.));
#19549=DIRECTION('',(0.,-1.,0.));
#19550=DIRECTION('center_axis',(0.,-1.,0.));
#19551=DIRECTION('ref_axis',(1.,0.,0.));
#19552=DIRECTION('center_axis',(0.,1.,0.));
#19553=DIRECTION('ref_axis',(1.,0.,0.));
#19554=DIRECTION('center_axis',(0.,1.,0.));
#19555=DIRECTION('ref_axis',(1.,0.,0.));
#19556=DIRECTION('',(0.,-1.,0.));
#19557=DIRECTION('center_axis',(0.,1.,0.));
#19558=DIRECTION('ref_axis',(1.,0.,0.));
#19559=DIRECTION('center_axis',(0.,1.,0.));
#19560=DIRECTION('ref_axis',(1.,0.,0.));
#19561=DIRECTION('center_axis',(0.,1.,0.));
#19562=DIRECTION('ref_axis',(1.,0.,0.));
#19563=DIRECTION('axis',(0.,0.,1.));
#19564=DIRECTION('refdir',(1.,0.,0.));
#19565=DIRECTION('center_axis',(0.,1.,0.));
#19566=DIRECTION('ref_axis',(1.,0.,0.));
#19567=DIRECTION('center_axis',(0.,1.,0.));
#19568=DIRECTION('ref_axis',(1.,0.,0.));
#19569=DIRECTION('',(0.,1.,0.));
#19570=DIRECTION('center_axis',(0.,-1.,0.));
#19571=DIRECTION('ref_axis',(1.,0.,0.));
#19572=DIRECTION('center_axis',(0.,1.,0.));
#19573=DIRECTION('ref_axis',(1.,0.,0.));
#19574=DIRECTION('center_axis',(0.,1.,0.));
#19575=DIRECTION('ref_axis',(1.,0.,0.));
#19576=DIRECTION('',(0.,1.,0.));
#19577=DIRECTION('center_axis',(0.,-1.,0.));
#19578=DIRECTION('ref_axis',(1.,0.,0.));
#19579=DIRECTION('center_axis',(0.,1.,0.));
#19580=DIRECTION('ref_axis',(1.,0.,0.));
#19581=DIRECTION('center_axis',(0.,1.,0.));
#19582=DIRECTION('ref_axis',(1.,0.,0.));
#19583=DIRECTION('',(0.,1.,0.));
#19584=DIRECTION('center_axis',(0.,-1.,0.));
#19585=DIRECTION('ref_axis',(1.,0.,0.));
#19586=DIRECTION('center_axis',(0.,1.,0.));
#19587=DIRECTION('ref_axis',(1.,0.,0.));
#19588=DIRECTION('center_axis',(0.,1.,0.));
#19589=DIRECTION('ref_axis',(1.,0.,0.));
#19590=DIRECTION('',(0.,1.,0.));
#19591=DIRECTION('center_axis',(0.,-1.,0.));
#19592=DIRECTION('ref_axis',(1.,0.,0.));
#19593=DIRECTION('center_axis',(0.,1.,0.));
#19594=DIRECTION('ref_axis',(1.,0.,0.));
#19595=DIRECTION('center_axis',(0.,1.,0.));
#19596=DIRECTION('ref_axis',(1.,0.,0.));
#19597=DIRECTION('',(0.,-1.,0.));
#19598=DIRECTION('center_axis',(0.,1.,0.));
#19599=DIRECTION('ref_axis',(1.,0.,0.));
#19600=DIRECTION('center_axis',(0.,1.,0.));
#19601=DIRECTION('ref_axis',(1.,0.,0.));
#19602=DIRECTION('center_axis',(0.,-1.,0.));
#19603=DIRECTION('ref_axis',(1.,0.,0.));
#19604=DIRECTION('center_axis',(0.,1.,0.));
#19605=DIRECTION('ref_axis',(1.,0.,0.));
#19606=DIRECTION('center_axis',(0.,-1.,0.));
#19607=DIRECTION('ref_axis',(1.,0.,0.));
#19608=DIRECTION('',(0.,-1.,0.));
#19609=DIRECTION('center_axis',(0.,1.,0.));
#19610=DIRECTION('ref_axis',(1.,0.,0.));
#19611=DIRECTION('center_axis',(0.,1.,0.));
#19612=DIRECTION('ref_axis',(1.,0.,0.));
#19613=DIRECTION('',(0.,-1.,0.));
#19614=DIRECTION('center_axis',(0.,1.,0.));
#19615=DIRECTION('ref_axis',(1.,0.,0.));
#19616=DIRECTION('center_axis',(0.,1.,0.));
#19617=DIRECTION('ref_axis',(1.,0.,0.));
#19618=DIRECTION('center_axis',(0.,1.,0.));
#19619=DIRECTION('ref_axis',(1.,0.,0.));
#19620=DIRECTION('axis',(0.,0.,1.));
#19621=DIRECTION('refdir',(1.,0.,0.));
#19622=DIRECTION('axis',(0.,0.,1.));
#19623=DIRECTION('refdir',(1.,0.,0.));
#19624=DIRECTION('center_axis',(0.,-1.,0.));
#19625=DIRECTION('ref_axis',(0.,0.,-1.));
#19626=DIRECTION('center_axis',(0.,-1.,0.));
#19627=DIRECTION('ref_axis',(1.,0.,0.));
#19628=DIRECTION('center_axis',(0.,-1.,0.));
#19629=DIRECTION('ref_axis',(1.,0.,0.));
#19630=DIRECTION('center_axis',(1.,0.,1.22464679914735E-16));
#19631=DIRECTION('ref_axis',(-1.22464679914735E-16,0.,1.));
#19632=DIRECTION('center_axis',(0.,1.,0.));
#19633=DIRECTION('ref_axis',(1.,0.,0.));
#19634=DIRECTION('center_axis',(0.,1.,0.));
#19635=DIRECTION('ref_axis',(1.,0.,0.));
#19636=DIRECTION('center_axis',(0.,-1.,0.));
#19637=DIRECTION('ref_axis',(1.,0.,0.));
#19638=DIRECTION('',(0.,1.,0.));
#19639=DIRECTION('center_axis',(0.,-1.,0.));
#19640=DIRECTION('ref_axis',(1.,0.,0.));
#19641=DIRECTION('center_axis',(0.,-1.,0.));
#19642=DIRECTION('ref_axis',(1.,0.,0.));
#19643=DIRECTION('center_axis',(0.,-1.,0.));
#19644=DIRECTION('ref_axis',(1.,0.,0.));
#19645=DIRECTION('',(0.,1.,0.));
#19646=DIRECTION('center_axis',(0.,-1.,0.));
#19647=DIRECTION('ref_axis',(1.,0.,0.));
#19648=DIRECTION('center_axis',(0.,1.,0.));
#19649=DIRECTION('ref_axis',(1.,0.,0.));
#19650=DIRECTION('',(-0.707106781186548,0.707106781186547,-8.65956056235493E-17));
#19651=DIRECTION('center_axis',(0.,-1.,0.));
#19652=DIRECTION('ref_axis',(1.,0.,0.));
#19653=DIRECTION('center_axis',(0.,1.,0.));
#19654=DIRECTION('ref_axis',(0.,0.,1.));
#19655=DIRECTION('center_axis',(0.,-1.,0.));
#19656=DIRECTION('ref_axis',(1.,0.,0.));
#19657=DIRECTION('center_axis',(0.,-1.,0.));
#19658=DIRECTION('ref_axis',(1.,0.,0.));
#19659=DIRECTION('',(0.,1.,0.));
#19660=DIRECTION('center_axis',(0.,-1.,0.));
#19661=DIRECTION('ref_axis',(0.,0.,-1.));
#19662=DIRECTION('center_axis',(0.,-1.,0.));
#19663=DIRECTION('ref_axis',(1.,0.,0.));
#19664=DIRECTION('center_axis',(0.,-1.,0.));
#19665=DIRECTION('ref_axis',(1.,0.,0.));
#19666=DIRECTION('',(0.707106781186548,0.707106781186547,8.65956056235493E-17));
#19667=DIRECTION('axis',(0.,0.,1.));
#19668=DIRECTION('refdir',(1.,0.,0.));
#19669=DIRECTION('center_axis',(0.,-1.,0.));
#19670=DIRECTION('ref_axis',(0.,0.,-1.));
#19671=DIRECTION('center_axis',(0.,-1.,0.));
#19672=DIRECTION('ref_axis',(1.,0.,0.));
#19673=DIRECTION('center_axis',(0.,-1.,0.));
#19674=DIRECTION('ref_axis',(1.,0.,0.));
#19675=DIRECTION('center_axis',(1.,0.,1.22464679914735E-16));
#19676=DIRECTION('ref_axis',(-1.22464679914735E-16,0.,1.));
#19677=DIRECTION('center_axis',(0.,1.,0.));
#19678=DIRECTION('ref_axis',(1.,0.,0.));
#19679=DIRECTION('center_axis',(0.,1.,0.));
#19680=DIRECTION('ref_axis',(1.,0.,0.));
#19681=DIRECTION('center_axis',(0.,-1.,0.));
#19682=DIRECTION('ref_axis',(1.,0.,0.));
#19683=DIRECTION('center_axis',(0.,-1.,0.));
#19684=DIRECTION('ref_axis',(1.,0.,0.));
#19685=DIRECTION('',(0.,1.,0.));
#19686=DIRECTION('center_axis',(0.,1.,0.));
#19687=DIRECTION('ref_axis',(0.,0.,1.));
#19688=DIRECTION('center_axis',(0.,-1.,0.));
#19689=DIRECTION('ref_axis',(1.,0.,0.));
#19690=DIRECTION('center_axis',(0.,-1.,0.));
#19691=DIRECTION('ref_axis',(1.,0.,0.));
#19692=DIRECTION('center_axis',(0.,-1.,0.));
#19693=DIRECTION('ref_axis',(1.,0.,0.));
#19694=DIRECTION('center_axis',(0.,-1.,0.));
#19695=DIRECTION('ref_axis',(1.,0.,0.));
#19696=DIRECTION('',(0.707106781186548,0.707106781186547,8.65956056235494E-17));
#19697=DIRECTION('center_axis',(0.,-1.,0.));
#19698=DIRECTION('ref_axis',(1.,0.,0.));
#19699=DIRECTION('center_axis',(0.,-1.,0.));
#19700=DIRECTION('ref_axis',(1.,0.,0.));
#19701=DIRECTION('',(0.,1.,0.));
#19702=DIRECTION('center_axis',(0.,1.,0.));
#19703=DIRECTION('ref_axis',(1.,0.,0.));
#19704=DIRECTION('center_axis',(0.,-1.,0.));
#19705=DIRECTION('ref_axis',(1.,0.,0.));
#19706=DIRECTION('',(-0.707106781186548,0.707106781186547,-8.65956056235494E-17));
#19707=DIRECTION('center_axis',(0.,-1.,0.));
#19708=DIRECTION('ref_axis',(0.,0.,-1.));
#19709=DIRECTION('center_axis',(0.,-1.,0.));
#19710=DIRECTION('ref_axis',(1.,0.,0.));
#19711=DIRECTION('',(0.,1.,0.));
#19712=DIRECTION('axis',(0.,0.,1.));
#19713=DIRECTION('refdir',(1.,0.,0.));
#19714=DIRECTION('center_axis',(0.,0.,1.));
#19715=DIRECTION('ref_axis',(1.,0.,0.));
#19716=DIRECTION('center_axis',(1.22464679914735E-16,-1.,0.));
#19717=DIRECTION('ref_axis',(-1.,-1.22464679914735E-16,0.));
#19718=DIRECTION('center_axis',(0.78183148246803,0.,0.623489801858733));
#19719=DIRECTION('ref_axis',(0.623489801858734,0.,-0.78183148246803));
#19720=DIRECTION('center_axis',(7.63554790147315E-17,-1.,-9.57467422477103E-17));
#19721=DIRECTION('ref_axis',(-0.623489801858734,-1.22464679914735E-16,0.78183148246803));
#19722=DIRECTION('center_axis',(0.974927912181824,0.,-0.222520933956314));
#19723=DIRECTION('ref_axis',(-0.222520933956314,0.,-0.974927912181824));
#19724=DIRECTION('center_axis',(-2.7250954951288E-17,-1.,-1.19394234705288E-16));
#19725=DIRECTION('ref_axis',(0.222520933956314,-1.22464679914735E-16,0.974927912181824));
#19726=DIRECTION('center_axis',(0.433883739117558,0.,-0.900968867902419));
#19727=DIRECTION('ref_axis',(-0.900968867902419,0.,-0.433883739117558));
#19728=DIRECTION('center_axis',(-1.10336864020811E-16,-1.,-5.31354332312403E-17));
#19729=DIRECTION('ref_axis',(0.900968867902419,-1.22464679914735E-16,0.433883739117558));
#19730=DIRECTION('center_axis',(-0.433883739117558,0.,-0.900968867902419));
#19731=DIRECTION('ref_axis',(-0.900968867902419,0.,0.433883739117558));
#19732=DIRECTION('center_axis',(-1.10336864020811E-16,-1.,5.31354332312403E-17));
#19733=DIRECTION('ref_axis',(0.900968867902419,-1.22464679914735E-16,-0.433883739117558));
#19734=DIRECTION('center_axis',(-0.974927912181824,0.,-0.222520933956314));
#19735=DIRECTION('ref_axis',(-0.222520933956315,0.,0.974927912181824));
#19736=DIRECTION('center_axis',(-2.7250954951288E-17,-1.,1.19394234705288E-16));
#19737=DIRECTION('ref_axis',(0.222520933956315,-1.22464679914735E-16,-0.974927912181824));
#19738=DIRECTION('center_axis',(-0.78183148246803,0.,0.623489801858734));
#19739=DIRECTION('ref_axis',(0.623489801858733,0.,0.78183148246803));
#19740=DIRECTION('center_axis',(7.63554790147315E-17,-1.,9.57467422477103E-17));
#19741=DIRECTION('ref_axis',(-0.623489801858733,-1.22464679914735E-16,-0.78183148246803));
#19742=DIRECTION('axis',(0.,0.,1.));
#19743=DIRECTION('refdir',(1.,0.,0.));
#19744=DIRECTION('center_axis',(0.,0.,1.));
#19745=DIRECTION('ref_axis',(1.,0.,0.));
#19746=DIRECTION('center_axis',(0.,-1.,0.));
#19747=DIRECTION('ref_axis',(0.,0.,-1.));
#19748=DIRECTION('center_axis',(0.,-1.,0.));
#19749=DIRECTION('ref_axis',(0.,0.,-1.));
#19750=DIRECTION('center_axis',(0.,1.,0.));
#19751=DIRECTION('ref_axis',(1.,0.,0.));
#19752=DIRECTION('center_axis',(0.,1.,0.));
#19753=DIRECTION('ref_axis',(1.,0.,0.));
#19754=DIRECTION('center_axis',(0.,1.,0.));
#19755=DIRECTION('ref_axis',(1.,0.,0.));
#19756=DIRECTION('center_axis',(0.,1.,0.));
#19757=DIRECTION('ref_axis',(1.,0.,0.));
#19758=DIRECTION('',(0.,-1.,0.));
#19759=DIRECTION('center_axis',(0.,-1.,0.));
#19760=DIRECTION('ref_axis',(1.,0.,0.));
#19761=DIRECTION('center_axis',(0.,1.,0.));
#19762=DIRECTION('ref_axis',(1.,0.,0.));
#19763=DIRECTION('center_axis',(0.,1.,0.));
#19764=DIRECTION('ref_axis',(1.,0.,0.));
#19765=DIRECTION('center_axis',(0.,1.,0.));
#19766=DIRECTION('ref_axis',(1.,0.,0.));
#19767=DIRECTION('center_axis',(0.,1.,0.));
#19768=DIRECTION('ref_axis',(1.,0.,0.));
#19769=DIRECTION('center_axis',(0.,1.,0.));
#19770=DIRECTION('ref_axis',(1.,0.,0.));
#19771=DIRECTION('center_axis',(0.,1.,0.));
#19772=DIRECTION('ref_axis',(1.,0.,0.));
#19773=DIRECTION('center_axis',(0.,-1.,0.));
#19774=DIRECTION('ref_axis',(1.,0.,0.));
#19775=DIRECTION('center_axis',(0.,-1.,0.));
#19776=DIRECTION('ref_axis',(0.,0.,-1.));
#19777=DIRECTION('center_axis',(8.96625347776458E-17,0.,1.));
#19778=DIRECTION('ref_axis',(1.,0.,0.));
#19779=DIRECTION('center_axis',(0.,-1.,0.));
#19780=DIRECTION('ref_axis',(0.,0.,-1.));
#19781=DIRECTION('center_axis',(0.,1.,0.));
#19782=DIRECTION('ref_axis',(1.,0.,0.));
#19783=DIRECTION('center_axis',(0.,-1.,0.));
#19784=DIRECTION('ref_axis',(1.,0.,0.));
#19785=DIRECTION('center_axis',(0.,-1.,0.));
#19786=DIRECTION('ref_axis',(0.,0.,-1.));
#19787=DIRECTION('center_axis',(0.,0.,1.));
#19788=DIRECTION('ref_axis',(1.,0.,0.));
#19789=DIRECTION('center_axis',(0.,-1.,0.));
#19790=DIRECTION('ref_axis',(0.,0.,-1.));
#19791=DIRECTION('center_axis',(0.,1.,0.));
#19792=DIRECTION('ref_axis',(1.,0.,0.));
#19793=DIRECTION('center_axis',(0.,-1.,0.));
#19794=DIRECTION('ref_axis',(1.,0.,0.));
#19795=DIRECTION('center_axis',(0.,-1.,0.));
#19796=DIRECTION('ref_axis',(1.,0.,0.));
#19797=DIRECTION('center_axis',(0.,-1.,0.));
#19798=DIRECTION('ref_axis',(0.,0.,-1.));
#19799=DIRECTION('center_axis',(0.,0.,1.));
#19800=DIRECTION('ref_axis',(1.,0.,0.));
#19801=DIRECTION('center_axis',(0.,-1.,0.));
#19802=DIRECTION('ref_axis',(0.,0.,-1.));
#19803=DIRECTION('center_axis',(0.,1.,0.));
#19804=DIRECTION('ref_axis',(1.,0.,0.));
#19805=DIRECTION('center_axis',(0.,-1.,0.));
#19806=DIRECTION('ref_axis',(1.,0.,0.));
#19807=DIRECTION('center_axis',(0.,-1.,0.));
#19808=DIRECTION('ref_axis',(0.,0.,-1.));
#19809=DIRECTION('center_axis',(8.96625347776458E-17,0.,1.));
#19810=DIRECTION('ref_axis',(1.,0.,0.));
#19811=DIRECTION('center_axis',(0.,-1.,0.));
#19812=DIRECTION('ref_axis',(0.,0.,-1.));
#19813=DIRECTION('center_axis',(0.,1.,0.));
#19814=DIRECTION('ref_axis',(1.,0.,0.));
#19815=DIRECTION('center_axis',(0.,-1.,0.));
#19816=DIRECTION('ref_axis',(1.,0.,0.));
#19817=DIRECTION('center_axis',(0.,-1.,0.));
#19818=DIRECTION('ref_axis',(0.,0.,-1.));
#19819=DIRECTION('center_axis',(0.,0.,1.));
#19820=DIRECTION('ref_axis',(1.,0.,0.));
#19821=DIRECTION('center_axis',(0.,-1.,0.));
#19822=DIRECTION('ref_axis',(0.,0.,-1.));
#19823=DIRECTION('center_axis',(0.,1.,0.));
#19824=DIRECTION('ref_axis',(1.,0.,0.));
#19825=DIRECTION('center_axis',(0.,1.,0.));
#19826=DIRECTION('ref_axis',(1.,0.,0.));
#19827=DIRECTION('',(0.,1.,0.));
#19828=DIRECTION('center_axis',(0.,-1.,0.));
#19829=DIRECTION('ref_axis',(1.,0.,0.));
#19830=DIRECTION('center_axis',(0.,-1.,0.));
#19831=DIRECTION('ref_axis',(1.,0.,0.));
#19832=DIRECTION('center_axis',(0.,1.,0.));
#19833=DIRECTION('ref_axis',(1.,0.,0.));
#19834=DIRECTION('center_axis',(0.,-1.,0.));
#19835=DIRECTION('ref_axis',(0.,0.,-1.));
#19836=DIRECTION('center_axis',(0.,0.,1.));
#19837=DIRECTION('ref_axis',(1.,0.,0.));
#19838=DIRECTION('center_axis',(0.,-1.,0.));
#19839=DIRECTION('ref_axis',(0.,0.,-1.));
#19840=DIRECTION('center_axis',(0.,-1.,0.));
#19841=DIRECTION('ref_axis',(-1.,0.,0.));
#19842=DIRECTION('center_axis',(0.,1.,0.));
#19843=DIRECTION('ref_axis',(1.,0.,0.));
#19844=DIRECTION('axis',(0.,0.,1.));
#19845=DIRECTION('refdir',(1.,0.,0.));
#19846=DIRECTION('center_axis',(0.,1.,0.));
#19847=DIRECTION('ref_axis',(0.,0.,1.));
#19848=DIRECTION('center_axis',(0.,-1.,0.));
#19849=DIRECTION('ref_axis',(1.,0.,0.));
#19850=DIRECTION('center_axis',(0.,-1.,0.));
#19851=DIRECTION('ref_axis',(1.,0.,0.));
#19852=DIRECTION('center_axis',(0.,-1.,0.));
#19853=DIRECTION('ref_axis',(1.,0.,0.));
#19854=DIRECTION('center_axis',(0.,-1.,0.));
#19855=DIRECTION('ref_axis',(1.,0.,0.));
#19856=DIRECTION('',(0.,1.,0.));
#19857=DIRECTION('center_axis',(0.,-1.,0.));
#19858=DIRECTION('ref_axis',(0.,0.,-1.));
#19859=DIRECTION('center_axis',(0.,-1.,0.));
#19860=DIRECTION('ref_axis',(1.,0.,0.));
#19861=DIRECTION('center_axis',(0.,-1.,0.));
#19862=DIRECTION('ref_axis',(1.,0.,0.));
#19863=DIRECTION('',(0.,1.,0.));
#19864=DIRECTION('center_axis',(0.,1.,0.));
#19865=DIRECTION('ref_axis',(0.,0.,1.));
#19866=DIRECTION('center_axis',(0.,-1.,0.));
#19867=DIRECTION('ref_axis',(1.,0.,0.));
#19868=DIRECTION('center_axis',(0.,-1.,0.));
#19869=DIRECTION('ref_axis',(1.,0.,0.));
#19870=DIRECTION('center_axis',(0.,-1.,0.));
#19871=DIRECTION('ref_axis',(1.,0.,0.));
#19872=DIRECTION('center_axis',(0.,-1.,0.));
#19873=DIRECTION('ref_axis',(1.,0.,0.));
#19874=DIRECTION('',(0.,1.,0.));
#19875=DIRECTION('center_axis',(0.,-1.,0.));
#19876=DIRECTION('ref_axis',(0.,0.,-1.));
#19877=DIRECTION('center_axis',(0.,-1.,0.));
#19878=DIRECTION('ref_axis',(1.,0.,0.));
#19879=DIRECTION('center_axis',(0.,-1.,0.));
#19880=DIRECTION('ref_axis',(1.,0.,0.));
#19881=DIRECTION('',(0.,1.,0.));
#19882=DIRECTION('',(0.,0.,1.));
#19883=DIRECTION('',(1.,0.,0.));
#19884=DIRECTION('',(0.,0.,1.));
#19885=DIRECTION('',(1.,0.,0.));
#19886=DIRECTION('',(0.,0.,1.));
#19887=DIRECTION('',(1.,0.,0.));
#19888=DIRECTION('',(0.,0.,1.));
#19889=DIRECTION('',(1.,0.,0.));
#19890=DIRECTION('',(0.,0.,1.));
#19891=DIRECTION('',(1.,0.,0.));
#19892=DIRECTION('axis',(0.,0.,1.));
#19893=DIRECTION('refdir',(1.,0.,0.));
#19894=DIRECTION('axis',(0.,0.,1.));
#19895=DIRECTION('refdir',(1.,0.,0.));
#19896=DIRECTION('center_axis',(0.,-1.,0.));
#19897=DIRECTION('ref_axis',(0.,0.,-1.));
#19898=DIRECTION('center_axis',(0.,-1.,0.));
#19899=DIRECTION('ref_axis',(1.,0.,0.));
#19900=DIRECTION('center_axis',(0.,-1.,0.));
#19901=DIRECTION('ref_axis',(1.,0.,0.));
#19902=DIRECTION('center_axis',(1.,0.,1.22464679914735E-16));
#19903=DIRECTION('ref_axis',(-1.22464679914735E-16,0.,1.));
#19904=DIRECTION('center_axis',(0.,1.,0.));
#19905=DIRECTION('ref_axis',(1.,0.,0.));
#19906=DIRECTION('center_axis',(0.,1.,0.));
#19907=DIRECTION('ref_axis',(1.,0.,0.));
#19908=DIRECTION('center_axis',(0.,-1.,0.));
#19909=DIRECTION('ref_axis',(1.,0.,0.));
#19910=DIRECTION('',(0.,1.,0.));
#19911=DIRECTION('center_axis',(0.,-1.,0.));
#19912=DIRECTION('ref_axis',(1.,0.,0.));
#19913=DIRECTION('center_axis',(0.,-1.,0.));
#19914=DIRECTION('ref_axis',(1.,0.,0.));
#19915=DIRECTION('center_axis',(0.,-1.,0.));
#19916=DIRECTION('ref_axis',(1.,0.,0.));
#19917=DIRECTION('',(0.,1.,0.));
#19918=DIRECTION('center_axis',(0.,-1.,0.));
#19919=DIRECTION('ref_axis',(1.,0.,0.));
#19920=DIRECTION('center_axis',(0.,1.,0.));
#19921=DIRECTION('ref_axis',(1.,0.,0.));
#19922=DIRECTION('',(-0.707106781186548,0.707106781186547,-8.65956056235494E-17));
#19923=DIRECTION('center_axis',(0.,-1.,0.));
#19924=DIRECTION('ref_axis',(1.,0.,0.));
#19925=DIRECTION('center_axis',(0.,1.,0.));
#19926=DIRECTION('ref_axis',(0.,0.,1.));
#19927=DIRECTION('center_axis',(0.,-1.,0.));
#19928=DIRECTION('ref_axis',(1.,0.,0.));
#19929=DIRECTION('center_axis',(0.,-1.,0.));
#19930=DIRECTION('ref_axis',(1.,0.,0.));
#19931=DIRECTION('',(0.,1.,0.));
#19932=DIRECTION('center_axis',(0.,-1.,0.));
#19933=DIRECTION('ref_axis',(0.,0.,-1.));
#19934=DIRECTION('center_axis',(0.,-1.,0.));
#19935=DIRECTION('ref_axis',(1.,0.,0.));
#19936=DIRECTION('center_axis',(0.,-1.,0.));
#19937=DIRECTION('ref_axis',(1.,0.,0.));
#19938=DIRECTION('',(0.707106781186548,0.707106781186547,8.65956056235494E-17));
#19939=DIRECTION('axis',(0.,0.,1.));
#19940=DIRECTION('refdir',(1.,0.,0.));
#19941=DIRECTION('center_axis',(0.,-1.,0.));
#19942=DIRECTION('ref_axis',(0.,0.,-1.));
#19943=DIRECTION('center_axis',(0.,-1.,0.));
#19944=DIRECTION('ref_axis',(1.,0.,0.));
#19945=DIRECTION('center_axis',(0.,-1.,0.));
#19946=DIRECTION('ref_axis',(1.,0.,0.));
#19947=DIRECTION('center_axis',(1.,0.,1.22464679914735E-16));
#19948=DIRECTION('ref_axis',(-1.22464679914735E-16,0.,1.));
#19949=DIRECTION('center_axis',(0.,1.,0.));
#19950=DIRECTION('ref_axis',(1.,0.,0.));
#19951=DIRECTION('center_axis',(0.,1.,0.));
#19952=DIRECTION('ref_axis',(1.,0.,0.));
#19953=DIRECTION('center_axis',(0.,-1.,0.));
#19954=DIRECTION('ref_axis',(1.,0.,0.));
#19955=DIRECTION('center_axis',(0.,-1.,0.));
#19956=DIRECTION('ref_axis',(1.,0.,0.));
#19957=DIRECTION('',(0.,1.,0.));
#19958=DIRECTION('center_axis',(0.,1.,0.));
#19959=DIRECTION('ref_axis',(0.,0.,1.));
#19960=DIRECTION('center_axis',(0.,-1.,0.));
#19961=DIRECTION('ref_axis',(1.,0.,0.));
#19962=DIRECTION('center_axis',(0.,-1.,0.));
#19963=DIRECTION('ref_axis',(1.,0.,0.));
#19964=DIRECTION('center_axis',(0.,-1.,0.));
#19965=DIRECTION('ref_axis',(1.,0.,0.));
#19966=DIRECTION('center_axis',(0.,-1.,0.));
#19967=DIRECTION('ref_axis',(1.,0.,0.));
#19968=DIRECTION('',(0.707106781186548,0.707106781186547,8.65956056235494E-17));
#19969=DIRECTION('center_axis',(0.,-1.,0.));
#19970=DIRECTION('ref_axis',(1.,0.,0.));
#19971=DIRECTION('center_axis',(0.,-1.,0.));
#19972=DIRECTION('ref_axis',(1.,0.,0.));
#19973=DIRECTION('',(0.,1.,0.));
#19974=DIRECTION('center_axis',(0.,1.,0.));
#19975=DIRECTION('ref_axis',(1.,0.,0.));
#19976=DIRECTION('center_axis',(0.,-1.,0.));
#19977=DIRECTION('ref_axis',(1.,0.,0.));
#19978=DIRECTION('',(-0.707106781186548,0.707106781186547,-8.65956056235494E-17));
#19979=DIRECTION('center_axis',(0.,-1.,0.));
#19980=DIRECTION('ref_axis',(0.,0.,-1.));
#19981=DIRECTION('center_axis',(0.,-1.,0.));
#19982=DIRECTION('ref_axis',(1.,0.,0.));
#19983=DIRECTION('',(0.,1.,0.));
#19984=DIRECTION('axis',(0.,0.,1.));
#19985=DIRECTION('refdir',(1.,0.,0.));
#19986=DIRECTION('center_axis',(0.,0.,1.));
#19987=DIRECTION('ref_axis',(1.,0.,0.));
#19988=DIRECTION('center_axis',(1.22464679914735E-16,-1.,0.));
#19989=DIRECTION('ref_axis',(-1.,-1.22464679914735E-16,0.));
#19990=DIRECTION('center_axis',(0.707106781186548,0.,0.707106781186548));
#19991=DIRECTION('ref_axis',(0.707106781186548,0.,-0.707106781186548));
#19992=DIRECTION('center_axis',(8.65956056235493E-17,-1.,-8.65956056235493E-17));
#19993=DIRECTION('ref_axis',(-0.707106781186548,-1.22464679914735E-16,0.707106781186548));
#19994=DIRECTION('center_axis',(1.,0.,0.));
#19995=DIRECTION('ref_axis',(6.12323399573677E-17,0.,-1.));
#19996=DIRECTION('center_axis',(7.49879891330929E-33,-1.,-1.22464679914735E-16));
#19997=DIRECTION('ref_axis',(-6.12323399573677E-17,-1.22464679914735E-16,
1.));
#19998=DIRECTION('center_axis',(0.707106781186548,0.,-0.707106781186548));
#19999=DIRECTION('ref_axis',(-0.707106781186548,0.,-0.707106781186548));
#20000=DIRECTION('center_axis',(-8.65956056235493E-17,-1.,-8.65956056235493E-17));
#20001=DIRECTION('ref_axis',(0.707106781186548,-1.22464679914735E-16,0.707106781186548));
#20002=DIRECTION('center_axis',(0.,0.,-1.));
#20003=DIRECTION('ref_axis',(-1.,0.,-1.22464679914735E-16));
#20004=DIRECTION('center_axis',(-1.22464679914735E-16,-1.,-1.49975978266186E-32));
#20005=DIRECTION('ref_axis',(1.,-1.22464679914735E-16,1.22464679914735E-16));
#20006=DIRECTION('center_axis',(-0.707106781186548,0.,-0.707106781186548));
#20007=DIRECTION('ref_axis',(-0.707106781186548,0.,0.707106781186548));
#20008=DIRECTION('center_axis',(-8.65956056235493E-17,-1.,8.65956056235493E-17));
#20009=DIRECTION('ref_axis',(0.707106781186548,-1.22464679914735E-16,-0.707106781186548));
#20010=DIRECTION('center_axis',(-1.,0.,0.));
#20011=DIRECTION('ref_axis',(-1.83697019872103E-16,0.,1.));
#20012=DIRECTION('center_axis',(-2.24963967399279E-32,-1.,1.22464679914735E-16));
#20013=DIRECTION('ref_axis',(1.83697019872103E-16,-1.22464679914735E-16,
-1.));
#20014=DIRECTION('center_axis',(-0.707106781186548,0.,0.707106781186548));
#20015=DIRECTION('ref_axis',(0.707106781186548,0.,0.707106781186548));
#20016=DIRECTION('center_axis',(8.65956056235493E-17,-1.,8.65956056235494E-17));
#20017=DIRECTION('ref_axis',(-0.707106781186548,-1.22464679914735E-16,-0.707106781186548));
#20018=DIRECTION('axis',(0.,0.,1.));
#20019=DIRECTION('refdir',(1.,0.,0.));
#20020=DIRECTION('center_axis',(0.,0.,1.));
#20021=DIRECTION('ref_axis',(1.,0.,0.));
#20022=DIRECTION('center_axis',(0.,-1.,0.));
#20023=DIRECTION('ref_axis',(0.,0.,-1.));
#20024=DIRECTION('center_axis',(0.,-1.,0.));
#20025=DIRECTION('ref_axis',(0.,0.,-1.));
#20026=DIRECTION('center_axis',(0.,1.,0.));
#20027=DIRECTION('ref_axis',(1.,0.,0.));
#20028=DIRECTION('center_axis',(0.,1.,0.));
#20029=DIRECTION('ref_axis',(1.,0.,0.));
#20030=DIRECTION('center_axis',(0.,1.,0.));
#20031=DIRECTION('ref_axis',(1.,0.,0.));
#20032=DIRECTION('center_axis',(0.,1.,0.));
#20033=DIRECTION('ref_axis',(1.,0.,0.));
#20034=DIRECTION('',(0.,-1.,0.));
#20035=DIRECTION('center_axis',(0.,-1.,0.));
#20036=DIRECTION('ref_axis',(1.,0.,0.));
#20037=DIRECTION('center_axis',(0.,1.,0.));
#20038=DIRECTION('ref_axis',(1.,0.,0.));
#20039=DIRECTION('center_axis',(0.,1.,0.));
#20040=DIRECTION('ref_axis',(1.,0.,0.));
#20041=DIRECTION('center_axis',(0.,1.,0.));
#20042=DIRECTION('ref_axis',(1.,0.,0.));
#20043=DIRECTION('center_axis',(0.,1.,0.));
#20044=DIRECTION('ref_axis',(1.,0.,0.));
#20045=DIRECTION('center_axis',(0.,1.,0.));
#20046=DIRECTION('ref_axis',(1.,0.,0.));
#20047=DIRECTION('center_axis',(0.,1.,0.));
#20048=DIRECTION('ref_axis',(1.,0.,0.));
#20049=DIRECTION('center_axis',(0.,-1.,0.));
#20050=DIRECTION('ref_axis',(1.,0.,0.));
#20051=DIRECTION('center_axis',(0.,-1.,0.));
#20052=DIRECTION('ref_axis',(0.,0.,-1.));
#20053=DIRECTION('center_axis',(6.12323399573677E-17,0.,1.));
#20054=DIRECTION('ref_axis',(1.,0.,0.));
#20055=DIRECTION('center_axis',(0.,-1.,0.));
#20056=DIRECTION('ref_axis',(0.,0.,-1.));
#20057=DIRECTION('center_axis',(0.,1.,0.));
#20058=DIRECTION('ref_axis',(1.,0.,0.));
#20059=DIRECTION('center_axis',(0.,-1.,0.));
#20060=DIRECTION('ref_axis',(1.,0.,0.));
#20061=DIRECTION('center_axis',(0.,-1.,0.));
#20062=DIRECTION('ref_axis',(0.,0.,-1.));
#20063=DIRECTION('center_axis',(0.,0.,1.));
#20064=DIRECTION('ref_axis',(1.,0.,0.));
#20065=DIRECTION('center_axis',(0.,-1.,0.));
#20066=DIRECTION('ref_axis',(0.,0.,-1.));
#20067=DIRECTION('center_axis',(0.,1.,0.));
#20068=DIRECTION('ref_axis',(1.,0.,0.));
#20069=DIRECTION('center_axis',(0.,-1.,0.));
#20070=DIRECTION('ref_axis',(1.,0.,0.));
#20071=DIRECTION('center_axis',(0.,-1.,0.));
#20072=DIRECTION('ref_axis',(0.,0.,-1.));
#20073=DIRECTION('center_axis',(0.,0.,1.));
#20074=DIRECTION('ref_axis',(1.,0.,0.));
#20075=DIRECTION('center_axis',(0.,-1.,0.));
#20076=DIRECTION('ref_axis',(0.,0.,-1.));
#20077=DIRECTION('center_axis',(0.,1.,0.));
#20078=DIRECTION('ref_axis',(1.,0.,0.));
#20079=DIRECTION('center_axis',(0.,-1.,0.));
#20080=DIRECTION('ref_axis',(1.,0.,0.));
#20081=DIRECTION('center_axis',(0.,-1.,0.));
#20082=DIRECTION('ref_axis',(0.,0.,-1.));
#20083=DIRECTION('center_axis',(0.,0.,1.));
#20084=DIRECTION('ref_axis',(1.,0.,0.));
#20085=DIRECTION('center_axis',(0.,-1.,0.));
#20086=DIRECTION('ref_axis',(0.,0.,-1.));
#20087=DIRECTION('center_axis',(0.,1.,0.));
#20088=DIRECTION('ref_axis',(1.,0.,0.));
#20089=DIRECTION('center_axis',(0.,-1.,0.));
#20090=DIRECTION('ref_axis',(1.,0.,0.));
#20091=DIRECTION('center_axis',(0.,-1.,0.));
#20092=DIRECTION('ref_axis',(0.,0.,-1.));
#20093=DIRECTION('center_axis',(6.12323399573676E-17,0.,1.));
#20094=DIRECTION('ref_axis',(1.,0.,0.));
#20095=DIRECTION('center_axis',(0.,-1.,0.));
#20096=DIRECTION('ref_axis',(0.,0.,-1.));
#20097=DIRECTION('center_axis',(0.,1.,0.));
#20098=DIRECTION('ref_axis',(1.,0.,0.));
#20099=DIRECTION('center_axis',(0.,-1.,0.));
#20100=DIRECTION('ref_axis',(1.,0.,0.));
#20101=DIRECTION('center_axis',(0.,-1.,0.));
#20102=DIRECTION('ref_axis',(0.,0.,-1.));
#20103=DIRECTION('center_axis',(0.,0.,1.));
#20104=DIRECTION('ref_axis',(1.,0.,0.));
#20105=DIRECTION('center_axis',(0.,-1.,0.));
#20106=DIRECTION('ref_axis',(0.,0.,-1.));
#20107=DIRECTION('center_axis',(0.,1.,0.));
#20108=DIRECTION('ref_axis',(1.,0.,0.));
#20109=DIRECTION('center_axis',(0.,1.,0.));
#20110=DIRECTION('ref_axis',(1.,0.,0.));
#20111=DIRECTION('',(0.,1.,0.));
#20112=DIRECTION('center_axis',(0.,-1.,0.));
#20113=DIRECTION('ref_axis',(1.,0.,0.));
#20114=DIRECTION('center_axis',(0.,-1.,0.));
#20115=DIRECTION('ref_axis',(1.,0.,0.));
#20116=DIRECTION('center_axis',(0.,1.,0.));
#20117=DIRECTION('ref_axis',(1.,0.,0.));
#20118=DIRECTION('center_axis',(0.,-1.,0.));
#20119=DIRECTION('ref_axis',(0.,0.,-1.));
#20120=DIRECTION('center_axis',(0.,0.,1.));
#20121=DIRECTION('ref_axis',(1.,0.,0.));
#20122=DIRECTION('center_axis',(0.,-1.,0.));
#20123=DIRECTION('ref_axis',(0.,0.,-1.));
#20124=DIRECTION('center_axis',(0.,-1.,0.));
#20125=DIRECTION('ref_axis',(-1.,0.,0.));
#20126=DIRECTION('center_axis',(0.,1.,0.));
#20127=DIRECTION('ref_axis',(1.,0.,0.));
#20128=DIRECTION('axis',(0.,0.,1.));
#20129=DIRECTION('refdir',(1.,0.,0.));
#20130=DIRECTION('center_axis',(0.,1.,0.));
#20131=DIRECTION('ref_axis',(0.,0.,1.));
#20132=DIRECTION('center_axis',(0.,-1.,0.));
#20133=DIRECTION('ref_axis',(1.,0.,0.));
#20134=DIRECTION('center_axis',(0.,-1.,0.));
#20135=DIRECTION('ref_axis',(1.,0.,0.));
#20136=DIRECTION('center_axis',(0.,-1.,0.));
#20137=DIRECTION('ref_axis',(1.,0.,0.));
#20138=DIRECTION('center_axis',(0.,-1.,0.));
#20139=DIRECTION('ref_axis',(1.,0.,0.));
#20140=DIRECTION('',(0.,1.,0.));
#20141=DIRECTION('center_axis',(0.,-1.,0.));
#20142=DIRECTION('ref_axis',(0.,0.,-1.));
#20143=DIRECTION('center_axis',(0.,-1.,0.));
#20144=DIRECTION('ref_axis',(1.,0.,0.));
#20145=DIRECTION('center_axis',(0.,-1.,0.));
#20146=DIRECTION('ref_axis',(1.,0.,0.));
#20147=DIRECTION('',(0.,1.,0.));
#20148=DIRECTION('center_axis',(0.,1.,0.));
#20149=DIRECTION('ref_axis',(0.,0.,1.));
#20150=DIRECTION('center_axis',(0.,-1.,0.));
#20151=DIRECTION('ref_axis',(1.,0.,0.));
#20152=DIRECTION('center_axis',(0.,-1.,0.));
#20153=DIRECTION('ref_axis',(1.,0.,0.));
#20154=DIRECTION('center_axis',(0.,-1.,0.));
#20155=DIRECTION('ref_axis',(1.,0.,0.));
#20156=DIRECTION('center_axis',(0.,-1.,0.));
#20157=DIRECTION('ref_axis',(1.,0.,0.));
#20158=DIRECTION('',(0.,1.,0.));
#20159=DIRECTION('center_axis',(0.,-1.,0.));
#20160=DIRECTION('ref_axis',(0.,0.,-1.));
#20161=DIRECTION('center_axis',(0.,-1.,0.));
#20162=DIRECTION('ref_axis',(1.,0.,0.));
#20163=DIRECTION('center_axis',(0.,-1.,0.));
#20164=DIRECTION('ref_axis',(1.,0.,0.));
#20165=DIRECTION('',(0.,1.,0.));
#20166=DIRECTION('',(0.,0.,1.));
#20167=DIRECTION('',(1.,0.,0.));
#20168=DIRECTION('',(0.,0.,1.));
#20169=DIRECTION('',(1.,0.,0.));
#20170=DIRECTION('',(0.,0.,1.));
#20171=DIRECTION('',(1.,0.,0.));
#20172=DIRECTION('',(0.,0.,1.));
#20173=DIRECTION('',(1.,0.,0.));
#20174=DIRECTION('',(0.,0.,1.));
#20175=DIRECTION('',(1.,0.,0.));
#20176=DIRECTION('axis',(0.,0.,1.));
#20177=DIRECTION('refdir',(1.,0.,0.));
#20178=DIRECTION('center_axis',(0.866025403784439,0.,-0.5));
#20179=DIRECTION('ref_axis',(0.5,0.,0.866025403784439));
#20180=DIRECTION('',(-0.5,0.,-0.866025403784439));
#20181=DIRECTION('',(0.,-1.,0.));
#20182=DIRECTION('',(0.5,0.,0.866025403784439));
#20183=DIRECTION('',(0.,-1.,0.));
#20184=DIRECTION('center_axis',(1.60246890531964E-16,0.,-1.));
#20185=DIRECTION('ref_axis',(1.,0.,1.60246890531964E-16));
#20186=DIRECTION('',(-1.,0.,-1.60246890531964E-16));
#20187=DIRECTION('',(0.,-1.,0.));
#20188=DIRECTION('',(1.,0.,1.60246890531964E-16));
#20189=DIRECTION('center_axis',(-0.866025403784439,0.,-0.5));
#20190=DIRECTION('ref_axis',(0.5,0.,-0.866025403784439));
#20191=DIRECTION('',(-0.5,0.,0.866025403784439));
#20192=DIRECTION('',(0.,-1.,0.));
#20193=DIRECTION('',(0.5,0.,-0.866025403784439));
#20194=DIRECTION('center_axis',(-0.866025403784439,0.,0.5));
#20195=DIRECTION('ref_axis',(-0.5,0.,-0.866025403784439));
#20196=DIRECTION('',(0.5,0.,0.866025403784439));
#20197=DIRECTION('',(0.,-1.,0.));
#20198=DIRECTION('',(-0.5,0.,-0.866025403784439));
#20199=DIRECTION('center_axis',(-1.60246890531964E-16,0.,1.));
#20200=DIRECTION('ref_axis',(-1.,0.,-1.60246890531964E-16));
#20201=DIRECTION('',(1.,0.,1.60246890531964E-16));
#20202=DIRECTION('',(0.,-1.,0.));
#20203=DIRECTION('',(-1.,0.,-1.60246890531964E-16));
#20204=DIRECTION('center_axis',(0.866025403784439,0.,0.5));
#20205=DIRECTION('ref_axis',(-0.5,0.,0.866025403784439));
#20206=DIRECTION('',(0.5,0.,-0.866025403784439));
#20207=DIRECTION('',(-0.5,0.,0.866025403784439));
#20208=DIRECTION('center_axis',(0.,1.,0.));
#20209=DIRECTION('ref_axis',(1.,0.,0.));
#20210=DIRECTION('center_axis',(0.,-1.,0.));
#20211=DIRECTION('ref_axis',(0.,0.,-1.));
#20212=DIRECTION('center_axis',(0.,1.,0.));
#20213=DIRECTION('ref_axis',(1.,0.,0.));
#20214=DIRECTION('center_axis',(0.,1.,0.));
#20215=DIRECTION('ref_axis',(1.,0.,0.));
#20216=DIRECTION('center_axis',(0.,1.,0.));
#20217=DIRECTION('ref_axis',(0.,0.,1.));
#20218=DIRECTION('center_axis',(0.,-1.,0.));
#20219=DIRECTION('ref_axis',(1.,0.,0.));
#20220=DIRECTION('center_axis',(0.,-1.,0.));
#20221=DIRECTION('ref_axis',(1.,0.,0.));
#20222=DIRECTION('center_axis',(0.,-1.,0.));
#20223=DIRECTION('ref_axis',(1.,0.,0.));
#20224=DIRECTION('',(0.707106781186547,0.707106781186548,8.65956056235493E-17));
#20225=DIRECTION('center_axis',(0.,-1.,0.));
#20226=DIRECTION('ref_axis',(1.,0.,0.));
#20227=DIRECTION('center_axis',(0.,-1.,0.));
#20228=DIRECTION('ref_axis',(1.,0.,0.));
#20229=DIRECTION('',(0.,1.,0.));
#20230=DIRECTION('center_axis',(0.,1.,0.));
#20231=DIRECTION('ref_axis',(1.,0.,0.));
#20232=DIRECTION('center_axis',(0.,-1.,0.));
#20233=DIRECTION('ref_axis',(1.,0.,0.));
#20234=DIRECTION('',(-0.707106781186547,0.707106781186548,-8.65956056235493E-17));
#20235=DIRECTION('center_axis',(0.,-1.,0.));
#20236=DIRECTION('ref_axis',(0.,0.,-1.));
#20237=DIRECTION('center_axis',(0.,-1.,0.));
#20238=DIRECTION('ref_axis',(1.,0.,0.));
#20239=DIRECTION('center_axis',(0.,1.,0.));
#20240=DIRECTION('ref_axis',(1.,0.,0.));
#20241=DIRECTION('center_axis',(0.,1.,0.));
#20242=DIRECTION('ref_axis',(1.,0.,0.));
#20243=DIRECTION('',(-0.447213595499958,0.894427190999916,-5.47678698264203E-17));
#20244=DIRECTION('center_axis',(0.,-1.,0.));
#20245=DIRECTION('ref_axis',(1.,0.,0.));
#20246=DIRECTION('',(0.,1.,0.));
#20247=DIRECTION('axis',(0.,0.,1.));
#20248=DIRECTION('refdir',(1.,0.,0.));
#20249=DIRECTION('center_axis',(0.96592582628908,0.,-0.258819045102476));
#20250=DIRECTION('ref_axis',(-0.258819045102476,0.,-0.96592582628908));
#20251=DIRECTION('',(0.258819045102476,0.,0.96592582628908));
#20252=DIRECTION('',(0.,1.,0.));
#20253=DIRECTION('',(0.258819045102476,0.,0.96592582628908));
#20254=DIRECTION('',(0.,1.,0.));
#20255=DIRECTION('center_axis',(0.25108343875234,0.,0.967965447102478));
#20256=DIRECTION('ref_axis',(0.967965447102478,0.,-0.25108343875234));
#20257=DIRECTION('',(-0.967965447102478,0.,0.25108343875234));
#20258=DIRECTION('',(-0.967965447102478,0.,0.25108343875234));
#20259=DIRECTION('',(0.,1.,0.));
#20260=DIRECTION('center_axis',(-0.965925826289075,0.,0.258819045102495));
#20261=DIRECTION('ref_axis',(0.258819045102495,0.,0.965925826289075));
#20262=DIRECTION('',(-0.258819045102495,0.,-0.965925826289075));
#20263=DIRECTION('',(-0.258819045102495,0.,-0.965925826289075));
#20264=DIRECTION('',(0.,1.,0.));
#20265=DIRECTION('center_axis',(-0.266538087122156,0.,-0.963824386552479));
#20266=DIRECTION('ref_axis',(-0.963824386552479,0.,0.266538087122156));
#20267=DIRECTION('',(0.963824386552479,0.,-0.266538087122156));
#20268=DIRECTION('',(0.963824386552479,0.,-0.266538087122156));
#20269=DIRECTION('center_axis',(0.,1.,0.));
#20270=DIRECTION('ref_axis',(1.,0.,0.));
#20271=DIRECTION('center_axis',(0.866025403784429,0.,-0.500000000000017));
#20272=DIRECTION('ref_axis',(-0.500000000000017,0.,-0.866025403784429));
#20273=DIRECTION('',(0.500000000000017,0.,0.866025403784429));
#20274=DIRECTION('',(0.,1.,0.));
#20275=DIRECTION('',(0.500000000000017,0.,0.866025403784429));
#20276=DIRECTION('',(0.,1.,0.));
#20277=DIRECTION('center_axis',(0.493055870755657,0.,0.869997648452788));
#20278=DIRECTION('ref_axis',(0.869997648452788,0.,-0.493055870755657));
#20279=DIRECTION('',(-0.869997648452788,0.,0.493055870755657));
#20280=DIRECTION('',(-0.869997648452788,0.,0.493055870755657));
#20281=DIRECTION('',(0.,1.,0.));
#20282=DIRECTION('center_axis',(-0.866025403784438,0.,0.500000000000001));
#20283=DIRECTION('ref_axis',(0.500000000000001,0.,0.866025403784438));
#20284=DIRECTION('',(-0.500000000000001,0.,-0.866025403784438));
#20285=DIRECTION('',(-0.500000000000001,0.,-0.866025403784438));
#20286=DIRECTION('',(0.,1.,0.));
#20287=DIRECTION('center_axis',(-0.506912129415013,0.,-0.861997733785848));
#20288=DIRECTION('ref_axis',(-0.861997733785848,0.,0.506912129415013));
#20289=DIRECTION('',(0.861997733785848,0.,-0.506912129415013));
#20290=DIRECTION('',(0.861997733785848,0.,-0.506912129415013));
#20291=DIRECTION('center_axis',(0.,1.,0.));
#20292=DIRECTION('ref_axis',(1.,0.,0.));
#20293=DIRECTION('center_axis',(0.70710678118654,0.,-0.707106781186555));
#20294=DIRECTION('ref_axis',(-0.707106781186555,0.,-0.70710678118654));
#20295=DIRECTION('',(0.707106781186555,0.,0.70710678118654));
#20296=DIRECTION('',(0.,1.,0.));
#20297=DIRECTION('',(0.707106781186555,0.,0.70710678118654));
#20298=DIRECTION('',(0.,1.,0.));
#20299=DIRECTION('center_axis',(0.70142735998032,0.,0.712740947800137));
#20300=DIRECTION('ref_axis',(0.712740947800137,0.,-0.70142735998032));
#20301=DIRECTION('',(-0.712740947800137,0.,0.70142735998032));
#20302=DIRECTION('',(-0.712740947800137,0.,0.70142735998032));
#20303=DIRECTION('',(0.,1.,0.));
#20304=DIRECTION('center_axis',(-0.707106781186564,0.,0.707106781186531));
#20305=DIRECTION('ref_axis',(0.707106781186531,0.,0.707106781186564));
#20306=DIRECTION('',(-0.707106781186531,0.,-0.707106781186564));
#20307=DIRECTION('',(-0.707106781186531,0.,-0.707106781186564));
#20308=DIRECTION('',(0.,1.,0.));
#20309=DIRECTION('center_axis',(-0.712740947800136,0.,-0.701427359980322));
#20310=DIRECTION('ref_axis',(-0.701427359980322,0.,0.712740947800136));
#20311=DIRECTION('',(0.701427359980322,0.,-0.712740947800136));
#20312=DIRECTION('',(0.701427359980322,0.,-0.712740947800136));
#20313=DIRECTION('center_axis',(0.,1.,0.));
#20314=DIRECTION('ref_axis',(1.,0.,0.));
#20315=DIRECTION('center_axis',(0.500000000000008,0.,-0.866025403784434));
#20316=DIRECTION('ref_axis',(-0.866025403784434,0.,-0.500000000000008));
#20317=DIRECTION('',(0.866025403784434,0.,0.500000000000008));
#20318=DIRECTION('',(0.,1.,0.));
#20319=DIRECTION('',(0.866025403784434,0.,0.500000000000008));
#20320=DIRECTION('',(0.,1.,0.));
#20321=DIRECTION('center_axis',(0.861997733785848,0.,0.506912129415013));
#20322=DIRECTION('ref_axis',(0.506912129415013,0.,-0.861997733785848));
#20323=DIRECTION('',(-0.506912129415013,0.,0.861997733785848));
#20324=DIRECTION('',(-0.506912129415013,0.,0.861997733785848));
#20325=DIRECTION('',(0.,1.,0.));
#20326=DIRECTION('center_axis',(-0.500000000000017,0.,0.866025403784429));
#20327=DIRECTION('ref_axis',(0.866025403784429,0.,0.500000000000017));
#20328=DIRECTION('',(-0.866025403784429,0.,-0.500000000000017));
#20329=DIRECTION('',(-0.866025403784429,0.,-0.500000000000017));
#20330=DIRECTION('',(0.,1.,0.));
#20331=DIRECTION('center_axis',(-0.869997648452789,0.,-0.493055870755654));
#20332=DIRECTION('ref_axis',(-0.493055870755654,0.,0.869997648452789));
#20333=DIRECTION('',(0.493055870755654,0.,-0.869997648452789));
#20334=DIRECTION('',(0.493055870755654,0.,-0.869997648452789));
#20335=DIRECTION('center_axis',(0.,1.,0.));
#20336=DIRECTION('ref_axis',(1.,0.,0.));
#20337=DIRECTION('center_axis',(0.258819045102528,0.,-0.965925826289066));
#20338=DIRECTION('ref_axis',(-0.965925826289066,0.,-0.258819045102528));
#20339=DIRECTION('',(0.965925826289066,0.,0.258819045102528));
#20340=DIRECTION('',(0.,1.,0.));
#20341=DIRECTION('',(0.965925826289066,0.,0.258819045102528));
#20342=DIRECTION('',(0.,1.,0.));
#20343=DIRECTION('center_axis',(0.96382438655248,0.,0.26653808712215));
#20344=DIRECTION('ref_axis',(0.26653808712215,0.,-0.96382438655248));
#20345=DIRECTION('',(-0.26653808712215,0.,0.96382438655248));
#20346=DIRECTION('',(-0.26653808712215,0.,0.96382438655248));
#20347=DIRECTION('',(0.,1.,0.));
#20348=DIRECTION('center_axis',(-0.258819045102533,0.,0.965925826289065));
#20349=DIRECTION('ref_axis',(0.965925826289065,0.,0.258819045102533));
#20350=DIRECTION('',(-0.965925826289065,0.,-0.258819045102533));
#20351=DIRECTION('',(-0.965925826289065,0.,-0.258819045102533));
#20352=DIRECTION('',(0.,1.,0.));
#20353=DIRECTION('center_axis',(-0.967965447102477,0.,-0.251083438752344));
#20354=DIRECTION('ref_axis',(-0.251083438752344,0.,0.967965447102477));
#20355=DIRECTION('',(0.251083438752344,0.,-0.967965447102477));
#20356=DIRECTION('',(0.251083438752344,0.,-0.967965447102477));
#20357=DIRECTION('center_axis',(0.,1.,0.));
#20358=DIRECTION('ref_axis',(1.,0.,0.));
#20359=DIRECTION('center_axis',(0.,0.,-1.));
#20360=DIRECTION('ref_axis',(-1.,0.,0.));
#20361=DIRECTION('',(1.,0.,0.));
#20362=DIRECTION('',(0.,1.,0.));
#20363=DIRECTION('',(1.,0.,0.));
#20364=DIRECTION('',(0.,1.,0.));
#20365=DIRECTION('center_axis',(0.999968000170666,0.,0.00799991466693405));
#20366=DIRECTION('ref_axis',(0.00799991466693405,0.,-0.999968000170666));
#20367=DIRECTION('',(-0.00799991466693405,0.,0.999968000170666));
#20368=DIRECTION('',(-0.00799991466693405,0.,0.999968000170666));
#20369=DIRECTION('',(0.,1.,0.));
#20370=DIRECTION('center_axis',(0.,0.,1.));
#20371=DIRECTION('ref_axis',(1.,0.,0.));
#20372=DIRECTION('',(-1.,0.,0.));
#20373=DIRECTION('',(-1.,0.,0.));
#20374=DIRECTION('',(0.,1.,0.));
#20375=DIRECTION('center_axis',(-0.999968000170666,0.,0.00799991466694293));
#20376=DIRECTION('ref_axis',(0.00799991466694293,0.,0.999968000170666));
#20377=DIRECTION('',(-0.00799991466694293,0.,-0.999968000170666));
#20378=DIRECTION('',(-0.00799991466694293,0.,-0.999968000170666));
#20379=DIRECTION('center_axis',(0.,1.,0.));
#20380=DIRECTION('ref_axis',(1.,0.,0.));
#20381=DIRECTION('center_axis',(-0.258819045102499,0.,-0.965925826289074));
#20382=DIRECTION('ref_axis',(-0.965925826289074,0.,0.258819045102499));
#20383=DIRECTION('',(0.965925826289074,0.,-0.258819045102499));
#20384=DIRECTION('',(0.,1.,0.));
#20385=DIRECTION('',(0.965925826289074,0.,-0.258819045102499));
#20386=DIRECTION('',(0.,1.,0.));
#20387=DIRECTION('center_axis',(0.967965447102479,0.,-0.251083438752336));
#20388=DIRECTION('ref_axis',(-0.251083438752336,0.,-0.967965447102479));
#20389=DIRECTION('',(0.251083438752336,0.,0.967965447102479));
#20390=DIRECTION('',(0.251083438752336,0.,0.967965447102479));
#20391=DIRECTION('',(0.,1.,0.));
#20392=DIRECTION('center_axis',(0.258819045102534,0.,0.965925826289065));
#20393=DIRECTION('ref_axis',(0.965925826289065,0.,-0.258819045102534));
#20394=DIRECTION('',(-0.965925826289065,0.,0.258819045102534));
#20395=DIRECTION('',(-0.965925826289065,0.,0.258819045102534));
#20396=DIRECTION('',(0.,1.,0.));
#20397=DIRECTION('center_axis',(-0.963824386552478,0.,0.266538087122158));
#20398=DIRECTION('ref_axis',(0.266538087122158,0.,0.963824386552478));
#20399=DIRECTION('',(-0.266538087122158,0.,-0.963824386552478));
#20400=DIRECTION('',(-0.266538087122158,0.,-0.963824386552478));
#20401=DIRECTION('center_axis',(0.,1.,0.));
#20402=DIRECTION('ref_axis',(1.,0.,0.));
#20403=DIRECTION('center_axis',(-0.499999999999982,0.,-0.866025403784449));
#20404=DIRECTION('ref_axis',(-0.866025403784449,0.,0.499999999999982));
#20405=DIRECTION('',(0.866025403784449,0.,-0.499999999999982));
#20406=DIRECTION('',(0.,1.,0.));
#20407=DIRECTION('',(0.866025403784449,0.,-0.499999999999982));
#20408=DIRECTION('',(0.,1.,0.));
#20409=DIRECTION('center_axis',(0.869997648452789,0.,-0.493055870755654));
#20410=DIRECTION('ref_axis',(-0.493055870755654,0.,-0.869997648452789));
#20411=DIRECTION('',(0.493055870755654,0.,0.869997648452789));
#20412=DIRECTION('',(0.493055870755654,0.,0.869997648452789));
#20413=DIRECTION('',(0.,1.,0.));
#20414=DIRECTION('center_axis',(0.500000000000001,0.,0.866025403784438));
#20415=DIRECTION('ref_axis',(0.866025403784438,0.,-0.500000000000001));
#20416=DIRECTION('',(-0.866025403784438,0.,0.500000000000001));
#20417=DIRECTION('',(-0.866025403784438,0.,0.500000000000001));
#20418=DIRECTION('',(0.,1.,0.));
#20419=DIRECTION('center_axis',(-0.861997733785848,0.,0.506912129415012));
#20420=DIRECTION('ref_axis',(0.506912129415012,0.,0.861997733785848));
#20421=DIRECTION('',(-0.506912129415012,0.,-0.861997733785848));
#20422=DIRECTION('',(-0.506912129415012,0.,-0.861997733785848));
#20423=DIRECTION('center_axis',(0.,1.,0.));
#20424=DIRECTION('ref_axis',(1.,0.,0.));
#20425=DIRECTION('center_axis',(-0.707106781186555,0.,-0.70710678118654));
#20426=DIRECTION('ref_axis',(-0.70710678118654,0.,0.707106781186555));
#20427=DIRECTION('',(0.70710678118654,0.,-0.707106781186555));
#20428=DIRECTION('',(0.,1.,0.));
#20429=DIRECTION('',(0.70710678118654,0.,-0.707106781186555));
#20430=DIRECTION('',(0.,1.,0.));
#20431=DIRECTION('center_axis',(0.712740947800135,0.,-0.701427359980323));
#20432=DIRECTION('ref_axis',(-0.701427359980323,0.,-0.712740947800135));
#20433=DIRECTION('',(0.701427359980323,0.,0.712740947800135));
#20434=DIRECTION('',(0.701427359980323,0.,0.712740947800135));
#20435=DIRECTION('',(0.,1.,0.));
#20436=DIRECTION('center_axis',(0.707106781186539,0.,0.707106781186556));
#20437=DIRECTION('ref_axis',(0.707106781186556,0.,-0.707106781186539));
#20438=DIRECTION('',(-0.707106781186556,0.,0.707106781186539));
#20439=DIRECTION('',(-0.707106781186556,0.,0.707106781186539));
#20440=DIRECTION('',(0.,1.,0.));
#20441=DIRECTION('center_axis',(-0.701427359980323,0.,0.712740947800135));
#20442=DIRECTION('ref_axis',(0.712740947800135,0.,0.701427359980323));
#20443=DIRECTION('',(-0.712740947800135,0.,-0.701427359980323));
#20444=DIRECTION('',(-0.712740947800135,0.,-0.701427359980323));
#20445=DIRECTION('center_axis',(0.,1.,0.));
#20446=DIRECTION('ref_axis',(1.,0.,0.));
#20447=DIRECTION('center_axis',(-0.866025403784425,0.,-0.500000000000023));
#20448=DIRECTION('ref_axis',(-0.500000000000023,0.,0.866025403784425));
#20449=DIRECTION('',(0.500000000000023,0.,-0.866025403784425));
#20450=DIRECTION('',(0.,1.,0.));
#20451=DIRECTION('',(0.500000000000023,0.,-0.866025403784425));
#20452=DIRECTION('',(0.,1.,0.));
#20453=DIRECTION('center_axis',(0.50691212941501,0.,-0.86199773378585));
#20454=DIRECTION('ref_axis',(-0.86199773378585,0.,-0.50691212941501));
#20455=DIRECTION('',(0.86199773378585,0.,0.50691212941501));
#20456=DIRECTION('',(0.86199773378585,0.,0.50691212941501));
#20457=DIRECTION('',(0.,1.,0.));
#20458=DIRECTION('center_axis',(0.866025403784448,0.,0.499999999999983));
#20459=DIRECTION('ref_axis',(0.499999999999983,0.,-0.866025403784448));
#20460=DIRECTION('',(-0.499999999999983,0.,0.866025403784448));
#20461=DIRECTION('',(-0.499999999999983,0.,0.866025403784448));
#20462=DIRECTION('',(0.,1.,0.));
#20463=DIRECTION('center_axis',(-0.493055870755651,0.,0.869997648452791));
#20464=DIRECTION('ref_axis',(0.869997648452791,0.,0.493055870755651));
#20465=DIRECTION('',(-0.869997648452791,0.,-0.493055870755651));
#20466=DIRECTION('',(-0.869997648452791,0.,-0.493055870755651));
#20467=DIRECTION('center_axis',(0.,1.,0.));
#20468=DIRECTION('ref_axis',(1.,0.,0.));
#20469=DIRECTION('center_axis',(-0.965925826289073,0.,-0.258819045102503));
#20470=DIRECTION('ref_axis',(-0.258819045102503,0.,0.965925826289073));
#20471=DIRECTION('',(0.258819045102503,0.,-0.965925826289073));
#20472=DIRECTION('',(0.,1.,0.));
#20473=DIRECTION('',(0.258819045102503,0.,-0.965925826289073));
#20474=DIRECTION('',(0.,1.,0.));
#20475=DIRECTION('center_axis',(0.266538087122153,0.,-0.96382438655248));
#20476=DIRECTION('ref_axis',(-0.96382438655248,0.,-0.266538087122153));
#20477=DIRECTION('',(0.96382438655248,0.,0.266538087122153));
#20478=DIRECTION('',(0.96382438655248,0.,0.266538087122153));
#20479=DIRECTION('',(0.,1.,0.));
#20480=DIRECTION('center_axis',(0.965925826289077,0.,0.258819045102487));
#20481=DIRECTION('ref_axis',(0.258819045102487,0.,-0.965925826289077));
#20482=DIRECTION('',(-0.258819045102487,0.,0.965925826289077));
#20483=DIRECTION('',(-0.258819045102487,0.,0.965925826289077));
#20484=DIRECTION('',(0.,1.,0.));
#20485=DIRECTION('center_axis',(-0.25108343875234,0.,0.967965447102478));
#20486=DIRECTION('ref_axis',(0.967965447102478,0.,0.25108343875234));
#20487=DIRECTION('',(-0.967965447102478,0.,-0.25108343875234));
#20488=DIRECTION('',(-0.967965447102478,0.,-0.25108343875234));
#20489=DIRECTION('center_axis',(0.,1.,0.));
#20490=DIRECTION('ref_axis',(1.,0.,0.));
#20491=DIRECTION('center_axis',(-1.,0.,0.));
#20492=DIRECTION('ref_axis',(0.,0.,1.));
#20493=DIRECTION('',(0.,0.,-1.));
#20494=DIRECTION('',(0.,1.,0.));
#20495=DIRECTION('',(0.,0.,-1.));
#20496=DIRECTION('',(0.,1.,0.));
#20497=DIRECTION('center_axis',(0.00799991466693849,0.,-0.999968000170666));
#20498=DIRECTION('ref_axis',(-0.999968000170666,0.,-0.00799991466693849));
#20499=DIRECTION('',(0.999968000170666,0.,0.00799991466693849));
#20500=DIRECTION('',(0.999968000170666,0.,0.00799991466693849));
#20501=DIRECTION('',(0.,1.,0.));
#20502=DIRECTION('center_axis',(1.,0.,0.));
#20503=DIRECTION('ref_axis',(0.,0.,-1.));
#20504=DIRECTION('',(0.,0.,1.));
#20505=DIRECTION('',(0.,0.,1.));
#20506=DIRECTION('',(0.,1.,0.));
#20507=DIRECTION('center_axis',(0.00799991466693849,0.,0.999968000170666));
#20508=DIRECTION('ref_axis',(0.999968000170666,0.,-0.00799991466693849));
#20509=DIRECTION('',(-0.999968000170666,0.,0.00799991466693849));
#20510=DIRECTION('',(-0.999968000170666,0.,0.00799991466693849));
#20511=DIRECTION('center_axis',(0.,1.,0.));
#20512=DIRECTION('ref_axis',(1.,0.,0.));
#20513=DIRECTION('center_axis',(-0.965925826289065,0.,0.258819045102534));
#20514=DIRECTION('ref_axis',(0.258819045102534,0.,0.965925826289065));
#20515=DIRECTION('',(-0.258819045102534,0.,-0.965925826289065));
#20516=DIRECTION('',(0.,1.,0.));
#20517=DIRECTION('',(-0.258819045102534,0.,-0.965925826289065));
#20518=DIRECTION('',(0.,1.,0.));
#20519=DIRECTION('center_axis',(-0.251083438752344,0.,-0.967965447102477));
#20520=DIRECTION('ref_axis',(-0.967965447102477,0.,0.251083438752344));
#20521=DIRECTION('',(0.967965447102477,0.,-0.251083438752344));
#20522=DIRECTION('',(0.967965447102477,0.,-0.251083438752344));
#20523=DIRECTION('',(0.,1.,0.));
#20524=DIRECTION('center_axis',(0.965925826289061,0.,-0.258819045102548));
#20525=DIRECTION('ref_axis',(-0.258819045102548,0.,-0.965925826289061));
#20526=DIRECTION('',(0.258819045102548,0.,0.965925826289061));
#20527=DIRECTION('',(0.258819045102548,0.,0.965925826289061));
#20528=DIRECTION('',(0.,1.,0.));
#20529=DIRECTION('center_axis',(0.266538087122154,0.,0.963824386552479));
#20530=DIRECTION('ref_axis',(0.963824386552479,0.,-0.266538087122154));
#20531=DIRECTION('',(-0.963824386552479,0.,0.266538087122154));
#20532=DIRECTION('',(-0.963824386552479,0.,0.266538087122154));
#20533=DIRECTION('center_axis',(0.,1.,0.));
#20534=DIRECTION('ref_axis',(1.,0.,0.));
#20535=DIRECTION('center_axis',(-0.866025403784429,0.,0.500000000000017));
#20536=DIRECTION('ref_axis',(0.500000000000017,0.,0.866025403784429));
#20537=DIRECTION('',(-0.500000000000017,0.,-0.866025403784429));
#20538=DIRECTION('',(0.,1.,0.));
#20539=DIRECTION('',(-0.500000000000017,0.,-0.866025403784429));
#20540=DIRECTION('',(0.,1.,0.));
#20541=DIRECTION('center_axis',(-0.493055870755655,0.,-0.869997648452789));
#20542=DIRECTION('ref_axis',(-0.869997648452789,0.,0.493055870755655));
#20543=DIRECTION('',(0.869997648452789,0.,-0.493055870755655));
#20544=DIRECTION('',(0.869997648452789,0.,-0.493055870755655));
#20545=DIRECTION('',(0.,1.,0.));
#20546=DIRECTION('center_axis',(0.866025403784452,0.,-0.499999999999976));
#20547=DIRECTION('ref_axis',(-0.499999999999976,0.,-0.866025403784452));
#20548=DIRECTION('',(0.499999999999976,0.,0.866025403784452));
#20549=DIRECTION('',(0.499999999999976,0.,0.866025403784452));
#20550=DIRECTION('',(0.,1.,0.));
#20551=DIRECTION('center_axis',(0.506912129415013,0.,0.861997733785848));
#20552=DIRECTION('ref_axis',(0.861997733785848,0.,-0.506912129415013));
#20553=DIRECTION('',(-0.861997733785848,0.,0.506912129415013));
#20554=DIRECTION('',(-0.861997733785848,0.,0.506912129415013));
#20555=DIRECTION('center_axis',(0.,1.,0.));
#20556=DIRECTION('ref_axis',(1.,0.,0.));
#20557=DIRECTION('center_axis',(-0.707106781186548,0.,0.707106781186548));
#20558=DIRECTION('ref_axis',(0.707106781186548,0.,0.707106781186548));
#20559=DIRECTION('',(-0.707106781186548,0.,-0.707106781186548));
#20560=DIRECTION('',(0.,1.,0.));
#20561=DIRECTION('',(-0.707106781186548,0.,-0.707106781186548));
#20562=DIRECTION('',(0.,1.,0.));
#20563=DIRECTION('center_axis',(-0.701427359980324,0.,-0.712740947800134));
#20564=DIRECTION('ref_axis',(-0.712740947800134,0.,0.701427359980324));
#20565=DIRECTION('',(0.712740947800134,0.,-0.701427359980324));
#20566=DIRECTION('',(0.712740947800134,0.,-0.701427359980324));
#20567=DIRECTION('',(0.,1.,0.));
#20568=DIRECTION('center_axis',(0.707106781186548,0.,-0.707106781186548));
#20569=DIRECTION('ref_axis',(-0.707106781186548,0.,-0.707106781186548));
#20570=DIRECTION('',(0.707106781186548,0.,0.707106781186548));
#20571=DIRECTION('',(0.707106781186548,0.,0.707106781186548));
#20572=DIRECTION('',(0.,1.,0.));
#20573=DIRECTION('center_axis',(0.712740947800134,0.,0.701427359980324));
#20574=DIRECTION('ref_axis',(0.701427359980324,0.,-0.712740947800134));
#20575=DIRECTION('',(-0.701427359980324,0.,0.712740947800134));
#20576=DIRECTION('',(-0.701427359980324,0.,0.712740947800134));
#20577=DIRECTION('center_axis',(0.,1.,0.));
#20578=DIRECTION('ref_axis',(1.,0.,0.));
#20579=DIRECTION('center_axis',(-0.50000000000003,0.,0.866025403784422));
#20580=DIRECTION('ref_axis',(0.866025403784422,0.,0.50000000000003));
#20581=DIRECTION('',(-0.866025403784422,0.,-0.50000000000003));
#20582=DIRECTION('',(0.,1.,0.));
#20583=DIRECTION('',(-0.866025403784422,0.,-0.50000000000003));
#20584=DIRECTION('',(0.,1.,0.));
#20585=DIRECTION('center_axis',(-0.861997733785848,0.,-0.506912129415013));
#20586=DIRECTION('ref_axis',(-0.506912129415013,0.,0.861997733785848));
#20587=DIRECTION('',(0.506912129415013,0.,-0.861997733785848));
#20588=DIRECTION('',(0.506912129415013,0.,-0.861997733785848));
#20589=DIRECTION('',(0.,1.,0.));
#20590=DIRECTION('center_axis',(0.500000000000001,0.,-0.866025403784438));
#20591=DIRECTION('ref_axis',(-0.866025403784438,0.,-0.500000000000001));
#20592=DIRECTION('',(0.866025403784438,0.,0.500000000000001));
#20593=DIRECTION('',(0.866025403784438,0.,0.500000000000001));
#20594=DIRECTION('',(0.,1.,0.));
#20595=DIRECTION('center_axis',(0.869997648452786,0.,0.49305587075566));
#20596=DIRECTION('ref_axis',(0.49305587075566,0.,-0.869997648452786));
#20597=DIRECTION('',(-0.49305587075566,0.,0.869997648452786));
#20598=DIRECTION('',(-0.49305587075566,0.,0.869997648452786));
#20599=DIRECTION('center_axis',(0.,1.,0.));
#20600=DIRECTION('ref_axis',(1.,0.,0.));
#20601=DIRECTION('center_axis',(-0.258819045102541,0.,0.965925826289063));
#20602=DIRECTION('ref_axis',(0.965925826289063,0.,0.258819045102541));
#20603=DIRECTION('',(-0.965925826289063,0.,-0.258819045102541));
#20604=DIRECTION('',(0.,1.,0.));
#20605=DIRECTION('',(-0.965925826289063,0.,-0.258819045102541));
#20606=DIRECTION('',(0.,1.,0.));
#20607=DIRECTION('center_axis',(-0.963824386552478,0.,-0.26653808712216));
#20608=DIRECTION('ref_axis',(-0.26653808712216,0.,0.963824386552478));
#20609=DIRECTION('',(0.26653808712216,0.,-0.963824386552478));
#20610=DIRECTION('',(0.26653808712216,0.,-0.963824386552478));
#20611=DIRECTION('',(0.,1.,0.));
#20612=DIRECTION('center_axis',(0.258819045102503,0.,-0.965925826289073));
#20613=DIRECTION('ref_axis',(-0.965925826289073,0.,-0.258819045102503));
#20614=DIRECTION('',(0.965925826289073,0.,0.258819045102503));
#20615=DIRECTION('',(0.965925826289073,0.,0.258819045102503));
#20616=DIRECTION('',(0.,1.,0.));
#20617=DIRECTION('center_axis',(0.967965447102477,0.,0.251083438752344));
#20618=DIRECTION('ref_axis',(0.251083438752344,0.,-0.967965447102477));
#20619=DIRECTION('',(-0.251083438752344,0.,0.967965447102477));
#20620=DIRECTION('',(-0.251083438752344,0.,0.967965447102477));
#20621=DIRECTION('center_axis',(0.,1.,0.));
#20622=DIRECTION('ref_axis',(1.,0.,0.));
#20623=DIRECTION('center_axis',(0.,0.,1.));
#20624=DIRECTION('ref_axis',(1.,0.,0.));
#20625=DIRECTION('',(-1.,0.,0.));
#20626=DIRECTION('',(0.,1.,0.));
#20627=DIRECTION('',(-1.,0.,0.));
#20628=DIRECTION('',(0.,1.,0.));
#20629=DIRECTION('center_axis',(-0.999968000170666,0.,-0.00799991466693405));
#20630=DIRECTION('ref_axis',(-0.00799991466693405,0.,0.999968000170666));
#20631=DIRECTION('',(0.00799991466693405,0.,-0.999968000170666));
#20632=DIRECTION('',(0.00799991466693405,0.,-0.999968000170666));
#20633=DIRECTION('',(0.,1.,0.));
#20634=DIRECTION('center_axis',(0.,0.,-1.));
#20635=DIRECTION('ref_axis',(-1.,0.,0.));
#20636=DIRECTION('',(1.,0.,0.));
#20637=DIRECTION('',(1.,0.,0.));
#20638=DIRECTION('',(0.,1.,0.));
#20639=DIRECTION('center_axis',(0.999968000170666,0.,-0.00799991466694293));
#20640=DIRECTION('ref_axis',(-0.00799991466694293,0.,-0.999968000170666));
#20641=DIRECTION('',(0.00799991466694293,0.,0.999968000170666));
#20642=DIRECTION('',(0.00799991466694293,0.,0.999968000170666));
#20643=DIRECTION('center_axis',(0.,1.,0.));
#20644=DIRECTION('ref_axis',(1.,0.,0.));
#20645=DIRECTION('center_axis',(0.258819045102527,0.,0.965925826289067));
#20646=DIRECTION('ref_axis',(0.965925826289067,0.,-0.258819045102527));
#20647=DIRECTION('',(-0.965925826289067,0.,0.258819045102527));
#20648=DIRECTION('',(0.,1.,0.));
#20649=DIRECTION('',(-0.965925826289067,0.,0.258819045102527));
#20650=DIRECTION('',(0.,1.,0.));
#20651=DIRECTION('center_axis',(-0.967965447102479,0.,0.251083438752335));
#20652=DIRECTION('ref_axis',(0.251083438752335,0.,0.967965447102479));
#20653=DIRECTION('',(-0.251083438752335,0.,-0.967965447102479));
#20654=DIRECTION('',(-0.251083438752335,0.,-0.967965447102479));
#20655=DIRECTION('',(0.,1.,0.));
#20656=DIRECTION('center_axis',(-0.258819045102503,0.,-0.965925826289073));
#20657=DIRECTION('ref_axis',(-0.965925826289073,0.,0.258819045102503));
#20658=DIRECTION('',(0.965925826289073,0.,-0.258819045102503));
#20659=DIRECTION('',(0.965925826289073,0.,-0.258819045102503));
#20660=DIRECTION('',(0.,1.,0.));
#20661=DIRECTION('center_axis',(0.963824386552478,0.,-0.26653808712216));
#20662=DIRECTION('ref_axis',(-0.26653808712216,0.,-0.963824386552478));
#20663=DIRECTION('',(0.26653808712216,0.,0.963824386552478));
#20664=DIRECTION('',(0.26653808712216,0.,0.963824386552478));
#20665=DIRECTION('center_axis',(0.,1.,0.));
#20666=DIRECTION('ref_axis',(1.,0.,0.));
#20667=DIRECTION('center_axis',(0.500000000000008,0.,0.866025403784434));
#20668=DIRECTION('ref_axis',(0.866025403784434,0.,-0.500000000000008));
#20669=DIRECTION('',(-0.866025403784434,0.,0.500000000000008));
#20670=DIRECTION('',(0.,1.,0.));
#20671=DIRECTION('',(-0.866025403784434,0.,0.500000000000008));
#20672=DIRECTION('',(0.,1.,0.));
#20673=DIRECTION('center_axis',(-0.86999764845279,0.,0.493055870755653));
#20674=DIRECTION('ref_axis',(0.493055870755653,0.,0.86999764845279));
#20675=DIRECTION('',(-0.493055870755653,0.,-0.86999764845279));
#20676=DIRECTION('',(-0.493055870755653,0.,-0.86999764845279));
#20677=DIRECTION('',(0.,1.,0.));
#20678=DIRECTION('center_axis',(-0.500000000000004,0.,-0.866025403784436));
#20679=DIRECTION('ref_axis',(-0.866025403784436,0.,0.500000000000004));
#20680=DIRECTION('',(0.866025403784436,0.,-0.500000000000004));
#20681=DIRECTION('',(0.866025403784436,0.,-0.500000000000004));
#20682=DIRECTION('',(0.,1.,0.));
#20683=DIRECTION('center_axis',(0.861997733785848,0.,-0.506912129415013));
#20684=DIRECTION('ref_axis',(-0.506912129415013,0.,-0.861997733785848));
#20685=DIRECTION('',(0.506912129415013,0.,0.861997733785848));
#20686=DIRECTION('',(0.506912129415013,0.,0.861997733785848));
#20687=DIRECTION('center_axis',(0.,1.,0.));
#20688=DIRECTION('ref_axis',(1.,0.,0.));
#20689=DIRECTION('center_axis',(0.707106781186533,0.,0.707106781186562));
#20690=DIRECTION('ref_axis',(0.707106781186562,0.,-0.707106781186533));
#20691=DIRECTION('',(-0.707106781186562,0.,0.707106781186533));
#20692=DIRECTION('',(0.,1.,0.));
#20693=DIRECTION('',(-0.707106781186562,0.,0.707106781186533));
#20694=DIRECTION('',(0.,1.,0.));
#20695=DIRECTION('center_axis',(-0.712740947800136,0.,0.701427359980322));
#20696=DIRECTION('ref_axis',(0.701427359980322,0.,0.712740947800136));
#20697=DIRECTION('',(-0.701427359980322,0.,-0.712740947800136));
#20698=DIRECTION('',(-0.701427359980322,0.,-0.712740947800136));
#20699=DIRECTION('',(0.,1.,0.));
#20700=DIRECTION('center_axis',(-0.707106781186564,0.,-0.707106781186531));
#20701=DIRECTION('ref_axis',(-0.707106781186531,0.,0.707106781186564));
#20702=DIRECTION('',(0.707106781186531,0.,-0.707106781186564));
#20703=DIRECTION('',(0.707106781186531,0.,-0.707106781186564));
#20704=DIRECTION('',(0.,1.,0.));
#20705=DIRECTION('center_axis',(0.701427359980322,0.,-0.712740947800136));
#20706=DIRECTION('ref_axis',(-0.712740947800136,0.,-0.701427359980322));
#20707=DIRECTION('',(0.712740947800136,0.,0.701427359980322));
#20708=DIRECTION('',(0.712740947800136,0.,0.701427359980322));
#20709=DIRECTION('center_axis',(0.,1.,0.));
#20710=DIRECTION('ref_axis',(1.,0.,0.));
#20711=DIRECTION('center_axis',(0.866025403784429,0.,0.500000000000017));
#20712=DIRECTION('ref_axis',(0.500000000000017,0.,-0.866025403784429));
#20713=DIRECTION('',(-0.500000000000017,0.,0.866025403784429));
#20714=DIRECTION('',(0.,1.,0.));
#20715=DIRECTION('',(-0.500000000000017,0.,0.866025403784429));
#20716=DIRECTION('',(0.,1.,0.));
#20717=DIRECTION('center_axis',(-0.506912129415013,0.,0.861997733785848));
#20718=DIRECTION('ref_axis',(0.861997733785848,0.,0.506912129415013));
#20719=DIRECTION('',(-0.861997733785848,0.,-0.506912129415013));
#20720=DIRECTION('',(-0.861997733785848,0.,-0.506912129415013));
#20721=DIRECTION('',(0.,1.,0.));
#20722=DIRECTION('center_axis',(-0.866025403784438,0.,-0.500000000000001));
#20723=DIRECTION('ref_axis',(-0.500000000000001,0.,0.866025403784438));
#20724=DIRECTION('',(0.500000000000001,0.,-0.866025403784438));
#20725=DIRECTION('',(0.500000000000001,0.,-0.866025403784438));
#20726=DIRECTION('',(0.,1.,0.));
#20727=DIRECTION('center_axis',(0.493055870755657,0.,-0.869997648452788));
#20728=DIRECTION('ref_axis',(-0.869997648452788,0.,-0.493055870755657));
#20729=DIRECTION('',(0.869997648452788,0.,0.493055870755657));
#20730=DIRECTION('',(0.869997648452788,0.,0.493055870755657));
#20731=DIRECTION('center_axis',(0.,1.,0.));
#20732=DIRECTION('ref_axis',(1.,0.,0.));
#20733=DIRECTION('center_axis',(0.965925826289079,0.,0.258819045102479));
#20734=DIRECTION('ref_axis',(0.258819045102479,0.,-0.965925826289079));
#20735=DIRECTION('',(-0.258819045102479,0.,0.965925826289079));
#20736=DIRECTION('',(0.,1.,0.));
#20737=DIRECTION('',(-0.258819045102479,0.,0.965925826289079));
#20738=DIRECTION('',(0.,1.,0.));
#20739=DIRECTION('center_axis',(-0.266538087122154,0.,0.963824386552479));
#20740=DIRECTION('ref_axis',(0.963824386552479,0.,0.266538087122154));
#20741=DIRECTION('',(-0.963824386552479,0.,-0.266538087122154));
#20742=DIRECTION('',(-0.963824386552479,0.,-0.266538087122154));
#20743=DIRECTION('',(0.,1.,0.));
#20744=DIRECTION('center_axis',(-0.965925826289075,0.,-0.258819045102495));
#20745=DIRECTION('ref_axis',(-0.258819045102495,0.,0.965925826289075));
#20746=DIRECTION('',(0.258819045102495,0.,-0.965925826289075));
#20747=DIRECTION('',(0.258819045102495,0.,-0.965925826289075));
#20748=DIRECTION('',(0.,1.,0.));
#20749=DIRECTION('center_axis',(0.25108343875234,0.,-0.967965447102478));
#20750=DIRECTION('ref_axis',(-0.967965447102478,0.,-0.25108343875234));
#20751=DIRECTION('',(0.967965447102478,0.,0.25108343875234));
#20752=DIRECTION('',(0.967965447102478,0.,0.25108343875234));
#20753=DIRECTION('center_axis',(0.,1.,0.));
#20754=DIRECTION('ref_axis',(1.,0.,0.));
#20755=DIRECTION('center_axis',(1.,0.,0.));
#20756=DIRECTION('ref_axis',(0.,0.,-1.));
#20757=DIRECTION('',(0.,0.,1.));
#20758=DIRECTION('',(0.,1.,0.));
#20759=DIRECTION('',(0.,0.,1.));
#20760=DIRECTION('',(0.,1.,0.));
#20761=DIRECTION('center_axis',(-0.00799991466693849,0.,0.999968000170666));
#20762=DIRECTION('ref_axis',(0.999968000170666,0.,0.00799991466693849));
#20763=DIRECTION('',(-0.999968000170666,0.,-0.00799991466693849));
#20764=DIRECTION('',(-0.999968000170666,0.,-0.00799991466693849));
#20765=DIRECTION('',(0.,1.,0.));
#20766=DIRECTION('center_axis',(-1.,0.,0.));
#20767=DIRECTION('ref_axis',(0.,0.,1.));
#20768=DIRECTION('',(0.,0.,-1.));
#20769=DIRECTION('',(0.,0.,-1.));
#20770=DIRECTION('',(0.,1.,0.));
#20771=DIRECTION('center_axis',(-0.00799991466693849,0.,-0.999968000170666));
#20772=DIRECTION('ref_axis',(-0.999968000170666,0.,0.00799991466693849));
#20773=DIRECTION('',(0.999968000170666,0.,-0.00799991466693849));
#20774=DIRECTION('',(0.999968000170666,0.,-0.00799991466693849));
#20775=DIRECTION('center_axis',(0.,1.,0.));
#20776=DIRECTION('ref_axis',(1.,0.,0.));
#20777=DIRECTION('center_axis',(0.,1.,0.));
#20778=DIRECTION('ref_axis',(1.,0.,0.));
#20779=DIRECTION('center_axis',(0.,1.,0.));
#20780=DIRECTION('ref_axis',(1.,0.,0.));
#20781=DIRECTION('',(0.,1.,0.));
#20782=DIRECTION('center_axis',(0.,-1.,0.));
#20783=DIRECTION('ref_axis',(1.,0.,0.));
#20784=DIRECTION('center_axis',(0.,1.,0.));
#20785=DIRECTION('ref_axis',(1.,0.,0.));
#20786=DIRECTION('center_axis',(0.,1.,0.));
#20787=DIRECTION('ref_axis',(1.,0.,0.));
#20788=DIRECTION('',(0.,1.,0.));
#20789=DIRECTION('center_axis',(0.,-1.,0.));
#20790=DIRECTION('ref_axis',(1.,0.,0.));
#20791=DIRECTION('center_axis',(0.,1.,0.));
#20792=DIRECTION('ref_axis',(1.,0.,0.));
#20793=DIRECTION('center_axis',(0.,1.,0.));
#20794=DIRECTION('ref_axis',(1.,0.,0.));
#20795=DIRECTION('',(0.,1.,0.));
#20796=DIRECTION('center_axis',(0.,-1.,0.));
#20797=DIRECTION('ref_axis',(1.,0.,0.));
#20798=DIRECTION('center_axis',(-1.,0.,0.));
#20799=DIRECTION('ref_axis',(0.,0.,1.));
#20800=DIRECTION('',(0.,1.,0.));
#20801=DIRECTION('',(0.,0.,-1.));
#20802=DIRECTION('',(0.,1.,0.));
#20803=DIRECTION('',(0.,0.,1.));
#20804=DIRECTION('center_axis',(-1.,0.,0.));
#20805=DIRECTION('ref_axis',(0.,0.,1.));
#20806=DIRECTION('',(0.,-1.,0.));
#20807=DIRECTION('',(0.,0.,1.));
#20808=DIRECTION('',(0.,1.,0.));
#20809=DIRECTION('',(0.,0.,-1.));
#20810=DIRECTION('center_axis',(0.,0.,-1.));
#20811=DIRECTION('ref_axis',(-1.,0.,0.));
#20812=DIRECTION('',(1.,0.,0.));
#20813=DIRECTION('',(-1.,0.,0.));
#20814=DIRECTION('',(0.,1.,0.));
#20815=DIRECTION('center_axis',(1.,0.,0.));
#20816=DIRECTION('ref_axis',(0.,0.,-1.));
#20817=DIRECTION('',(0.,0.,1.));
#20818=DIRECTION('',(0.,0.,-1.));
#20819=DIRECTION('',(0.,1.,0.));
#20820=DIRECTION('center_axis',(0.,0.,1.));
#20821=DIRECTION('ref_axis',(1.,0.,0.));
#20822=DIRECTION('',(-1.,0.,0.));
#20823=DIRECTION('',(1.,0.,0.));
#20824=DIRECTION('center_axis',(0.,0.,-1.));
#20825=DIRECTION('ref_axis',(-1.,0.,0.));
#20826=DIRECTION('',(1.,0.,0.));
#20827=DIRECTION('',(0.,-1.,0.));
#20828=DIRECTION('',(-1.,0.,0.));
#20829=DIRECTION('center_axis',(0.,1.,0.));
#20830=DIRECTION('ref_axis',(1.,0.,0.));
#20831=DIRECTION('',(-1.,0.,0.));
#20832=DIRECTION('center_axis',(0.,1.,0.));
#20833=DIRECTION('ref_axis',(1.,0.,0.));
#20834=DIRECTION('center_axis',(0.,0.,1.));
#20835=DIRECTION('ref_axis',(1.,0.,0.));
#20836=DIRECTION('',(1.,0.,0.));
#20837=DIRECTION('',(0.,1.,0.));
#20838=DIRECTION('center_axis',(0.,1.,0.));
#20839=DIRECTION('ref_axis',(1.,0.,0.));
#20840=DIRECTION('center_axis',(0.,1.,0.));
#20841=DIRECTION('ref_axis',(1.,0.,0.));
#20842=DIRECTION('center_axis',(0.,1.,0.));
#20843=DIRECTION('ref_axis',(-1.,0.,-1.22464679914735E-16));
#20844=DIRECTION('axis',(0.,0.,1.));
#20845=DIRECTION('refdir',(1.,0.,0.));
#20846=DIRECTION('center_axis',(0.,1.,0.));
#20847=DIRECTION('ref_axis',(1.,0.,0.));
#20848=DIRECTION('center_axis',(0.,1.,0.));
#20849=DIRECTION('ref_axis',(1.,0.,0.));
#20850=DIRECTION('',(0.,1.,0.));
#20851=DIRECTION('center_axis',(0.,-1.,0.));
#20852=DIRECTION('ref_axis',(1.,0.,0.));
#20853=DIRECTION('center_axis',(0.,1.,0.));
#20854=DIRECTION('ref_axis',(1.,0.,0.));
#20855=DIRECTION('center_axis',(0.,1.,0.));
#20856=DIRECTION('ref_axis',(1.,0.,0.));
#20857=DIRECTION('',(0.,-1.,0.));
#20858=DIRECTION('center_axis',(0.,1.,0.));
#20859=DIRECTION('ref_axis',(1.,0.,0.));
#20860=DIRECTION('center_axis',(0.,1.,0.));
#20861=DIRECTION('ref_axis',(1.,0.,0.));
#20862=DIRECTION('center_axis',(0.,1.,0.));
#20863=DIRECTION('ref_axis',(1.,0.,0.));
#20864=DIRECTION('axis',(0.,0.,1.));
#20865=DIRECTION('refdir',(1.,0.,0.));
#20866=DIRECTION('center_axis',(0.,1.,0.));
#20867=DIRECTION('ref_axis',(1.,0.,0.));
#20868=DIRECTION('center_axis',(0.,1.,0.));
#20869=DIRECTION('ref_axis',(1.,0.,0.));
#20870=DIRECTION('',(0.,1.,0.));
#20871=DIRECTION('center_axis',(0.,-1.,0.));
#20872=DIRECTION('ref_axis',(1.,0.,0.));
#20873=DIRECTION('center_axis',(0.,1.,0.));
#20874=DIRECTION('ref_axis',(1.,0.,0.));
#20875=DIRECTION('center_axis',(0.,1.,0.));
#20876=DIRECTION('ref_axis',(1.,0.,0.));
#20877=DIRECTION('',(0.,-1.,0.));
#20878=DIRECTION('center_axis',(0.,1.,0.));
#20879=DIRECTION('ref_axis',(1.,0.,0.));
#20880=DIRECTION('center_axis',(0.,1.,0.));
#20881=DIRECTION('ref_axis',(1.,0.,0.));
#20882=DIRECTION('center_axis',(0.,1.,0.));
#20883=DIRECTION('ref_axis',(1.,0.,0.));
#20884=DIRECTION('axis',(0.,0.,1.));
#20885=DIRECTION('refdir',(1.,0.,0.));
#20886=DIRECTION('center_axis',(0.,1.,0.));
#20887=DIRECTION('ref_axis',(-1.,0.,0.));
#20888=DIRECTION('',(-1.,0.,0.));
#20889=DIRECTION('',(0.,0.,1.));
#20890=DIRECTION('',(-1.,0.,0.));
#20891=DIRECTION('',(0.,0.,1.));
#20892=DIRECTION('center_axis',(1.,0.,0.));
#20893=DIRECTION('ref_axis',(0.,1.,0.));
#20894=DIRECTION('',(0.,1.,0.));
#20895=DIRECTION('',(0.,1.,0.));
#20896=DIRECTION('',(0.,0.,1.));
#20897=DIRECTION('center_axis',(0.,-1.,0.));
#20898=DIRECTION('ref_axis',(1.,0.,0.));
#20899=DIRECTION('',(1.,0.,0.));
#20900=DIRECTION('',(1.,0.,0.));
#20901=DIRECTION('',(0.,0.,1.));
#20902=DIRECTION('center_axis',(-1.,0.,0.));
#20903=DIRECTION('ref_axis',(0.,-1.,0.));
#20904=DIRECTION('',(0.,-1.,0.));
#20905=DIRECTION('',(0.,-1.,0.));
#20906=DIRECTION('center_axis',(0.,0.,1.));
#20907=DIRECTION('ref_axis',(1.,0.,0.));
#20908=DIRECTION('center_axis',(0.,0.,1.));
#20909=DIRECTION('ref_axis',(1.,0.,0.));
#20910=DIRECTION('axis',(0.,0.,1.));
#20911=DIRECTION('refdir',(1.,0.,0.));
#20912=DIRECTION('center_axis',(0.,1.,0.));
#20913=DIRECTION('ref_axis',(-1.,0.,0.));
#20914=DIRECTION('',(-1.,0.,0.));
#20915=DIRECTION('',(0.,0.,1.));
#20916=DIRECTION('',(-1.,0.,0.));
#20917=DIRECTION('',(0.,0.,1.));
#20918=DIRECTION('center_axis',(1.,0.,0.));
#20919=DIRECTION('ref_axis',(0.,1.,0.));
#20920=DIRECTION('',(0.,1.,0.));
#20921=DIRECTION('',(0.,1.,0.));
#20922=DIRECTION('',(0.,0.,1.));
#20923=DIRECTION('center_axis',(0.,-1.,0.));
#20924=DIRECTION('ref_axis',(1.,0.,0.));
#20925=DIRECTION('',(1.,0.,0.));
#20926=DIRECTION('',(1.,0.,0.));
#20927=DIRECTION('',(0.,0.,1.));
#20928=DIRECTION('center_axis',(-1.,0.,0.));
#20929=DIRECTION('ref_axis',(0.,-1.,0.));
#20930=DIRECTION('',(0.,-1.,0.));
#20931=DIRECTION('',(0.,-1.,0.));
#20932=DIRECTION('center_axis',(0.,0.,1.));
#20933=DIRECTION('ref_axis',(1.,0.,0.));
#20934=DIRECTION('center_axis',(0.,0.,1.));
#20935=DIRECTION('ref_axis',(1.,0.,0.));
#20936=DIRECTION('axis',(0.,0.,1.));
#20937=DIRECTION('refdir',(1.,0.,0.));
#20938=DIRECTION('center_axis',(0.866025403784439,0.,-0.5));
#20939=DIRECTION('ref_axis',(0.5,0.,0.866025403784439));
#20940=DIRECTION('',(-0.5,0.,-0.866025403784439));
#20941=DIRECTION('',(0.,-1.,0.));
#20942=DIRECTION('',(0.5,0.,0.866025403784439));
#20943=DIRECTION('',(0.,-1.,0.));
#20944=DIRECTION('center_axis',(1.60246890531964E-16,0.,-1.));
#20945=DIRECTION('ref_axis',(1.,0.,1.60246890531964E-16));
#20946=DIRECTION('',(-1.,0.,-1.60246890531964E-16));
#20947=DIRECTION('',(0.,-1.,0.));
#20948=DIRECTION('',(1.,0.,1.60246890531964E-16));
#20949=DIRECTION('center_axis',(-0.866025403784439,0.,-0.5));
#20950=DIRECTION('ref_axis',(0.5,0.,-0.866025403784439));
#20951=DIRECTION('',(-0.5,0.,0.866025403784439));
#20952=DIRECTION('',(0.,-1.,0.));
#20953=DIRECTION('',(0.5,0.,-0.866025403784439));
#20954=DIRECTION('center_axis',(-0.866025403784439,0.,0.5));
#20955=DIRECTION('ref_axis',(-0.5,0.,-0.866025403784439));
#20956=DIRECTION('',(0.5,0.,0.866025403784439));
#20957=DIRECTION('',(0.,-1.,0.));
#20958=DIRECTION('',(-0.5,0.,-0.866025403784439));
#20959=DIRECTION('center_axis',(-1.60246890531964E-16,0.,1.));
#20960=DIRECTION('ref_axis',(-1.,0.,-1.60246890531964E-16));
#20961=DIRECTION('',(1.,0.,1.60246890531964E-16));
#20962=DIRECTION('',(0.,-1.,0.));
#20963=DIRECTION('',(-1.,0.,-1.60246890531964E-16));
#20964=DIRECTION('center_axis',(0.866025403784439,0.,0.5));
#20965=DIRECTION('ref_axis',(-0.5,0.,0.866025403784439));
#20966=DIRECTION('',(0.5,0.,-0.866025403784439));
#20967=DIRECTION('',(-0.5,0.,0.866025403784439));
#20968=DIRECTION('center_axis',(0.,1.,0.));
#20969=DIRECTION('ref_axis',(1.,0.,0.));
#20970=DIRECTION('center_axis',(0.,-1.,0.));
#20971=DIRECTION('ref_axis',(0.,0.,-1.));
#20972=DIRECTION('center_axis',(0.,1.,0.));
#20973=DIRECTION('ref_axis',(1.,0.,0.));
#20974=DIRECTION('center_axis',(0.,1.,0.));
#20975=DIRECTION('ref_axis',(1.,0.,0.));
#20976=DIRECTION('center_axis',(0.,1.,0.));
#20977=DIRECTION('ref_axis',(1.,0.,0.));
#20978=DIRECTION('center_axis',(0.,1.,0.));
#20979=DIRECTION('ref_axis',(1.,0.,0.));
#20980=DIRECTION('',(0.,-1.,0.));
#20981=DIRECTION('center_axis',(0.,1.,0.));
#20982=DIRECTION('ref_axis',(1.,0.,0.));
#20983=DIRECTION('center_axis',(0.,1.,0.));
#20984=DIRECTION('ref_axis',(1.,0.,0.));
#20985=DIRECTION('center_axis',(0.,1.,0.));
#20986=DIRECTION('ref_axis',(0.,0.,1.));
#20987=DIRECTION('center_axis',(0.,-1.,0.));
#20988=DIRECTION('ref_axis',(1.,0.,0.));
#20989=DIRECTION('center_axis',(0.,-1.,0.));
#20990=DIRECTION('ref_axis',(1.,0.,0.));
#20991=DIRECTION('center_axis',(0.,-1.,0.));
#20992=DIRECTION('ref_axis',(1.,0.,0.));
#20993=DIRECTION('',(0.707106781186547,0.707106781186548,8.65956056235493E-17));
#20994=DIRECTION('center_axis',(0.,-1.,0.));
#20995=DIRECTION('ref_axis',(1.,0.,0.));
#20996=DIRECTION('center_axis',(0.,-1.,0.));
#20997=DIRECTION('ref_axis',(1.,0.,0.));
#20998=DIRECTION('',(0.,1.,0.));
#20999=DIRECTION('center_axis',(0.,1.,0.));
#21000=DIRECTION('ref_axis',(1.,0.,0.));
#21001=DIRECTION('center_axis',(0.,-1.,0.));
#21002=DIRECTION('ref_axis',(1.,0.,0.));
#21003=DIRECTION('',(-0.707106781186547,0.707106781186548,-8.65956056235493E-17));
#21004=DIRECTION('center_axis',(0.,-1.,0.));
#21005=DIRECTION('ref_axis',(0.,0.,-1.));
#21006=DIRECTION('center_axis',(0.,-1.,0.));
#21007=DIRECTION('ref_axis',(1.,0.,0.));
#21008=DIRECTION('center_axis',(0.,1.,0.));
#21009=DIRECTION('ref_axis',(1.,0.,0.));
#21010=DIRECTION('center_axis',(0.,1.,0.));
#21011=DIRECTION('ref_axis',(1.,0.,0.));
#21012=DIRECTION('',(-0.447213595499958,0.894427190999916,-5.47678698264203E-17));
#21013=DIRECTION('center_axis',(0.,-1.,0.));
#21014=DIRECTION('ref_axis',(1.,0.,0.));
#21015=DIRECTION('',(0.,1.,0.));
#21016=DIRECTION('axis',(0.,0.,1.));
#21017=DIRECTION('refdir',(1.,0.,0.));
#21018=DIRECTION('axis',(0.,0.,1.));
#21019=DIRECTION('refdir',(1.,0.,0.));
#21020=DIRECTION('center_axis',(0.,1.,0.));
#21021=DIRECTION('ref_axis',(1.,0.,0.));
#21022=DIRECTION('center_axis',(0.,1.,0.));
#21023=DIRECTION('ref_axis',(1.,0.,0.));
#21024=DIRECTION('',(0.,1.,0.));
#21025=DIRECTION('center_axis',(0.,-1.,0.));
#21026=DIRECTION('ref_axis',(1.,0.,0.));
#21027=DIRECTION('center_axis',(0.,1.,0.));
#21028=DIRECTION('ref_axis',(1.,0.,0.));
#21029=DIRECTION('center_axis',(-1.,0.,0.));
#21030=DIRECTION('ref_axis',(0.,0.,1.));
#21031=DIRECTION('',(0.,-1.,0.));
#21032=DIRECTION('',(0.,0.,1.));
#21033=DIRECTION('',(0.,1.,0.));
#21034=DIRECTION('',(0.,0.,-1.));
#21035=DIRECTION('center_axis',(0.,1.,0.));
#21036=DIRECTION('ref_axis',(1.,0.,0.));
#21037=DIRECTION('center_axis',(0.,-1.,0.));
#21038=DIRECTION('ref_axis',(1.,0.,0.));
#21039=DIRECTION('',(-1.,0.,0.));
#21040=DIRECTION('',(0.,0.,1.));
#21041=DIRECTION('center_axis',(1.,0.,0.));
#21042=DIRECTION('ref_axis',(0.,0.,-1.));
#21043=DIRECTION('',(0.,1.,0.));
#21044=DIRECTION('',(0.,1.,0.));
#21045=DIRECTION('',(0.,0.,-1.));
#21046=DIRECTION('center_axis',(0.,0.,1.));
#21047=DIRECTION('ref_axis',(1.,0.,0.));
#21048=DIRECTION('',(1.,0.,0.));
#21049=DIRECTION('center_axis',(0.,1.,0.));
#21050=DIRECTION('ref_axis',(0.,0.,1.));
#21051=DIRECTION('center_axis',(0.,1.,0.));
#21052=DIRECTION('ref_axis',(1.,0.,0.));
#21053=DIRECTION('center_axis',(-1.,0.,0.));
#21054=DIRECTION('ref_axis',(0.,0.,1.));
#21055=DIRECTION('',(0.,-1.,0.));
#21056=DIRECTION('',(0.,0.,1.));
#21057=DIRECTION('',(0.,1.,0.));
#21058=DIRECTION('',(0.,0.,-1.));
#21059=DIRECTION('center_axis',(0.,1.,0.));
#21060=DIRECTION('ref_axis',(1.,0.,0.));
#21061=DIRECTION('center_axis',(0.,-1.,0.));
#21062=DIRECTION('ref_axis',(1.,0.,0.));
#21063=DIRECTION('',(-1.,0.,0.));
#21064=DIRECTION('',(0.,0.,1.));
#21065=DIRECTION('center_axis',(1.,0.,0.));
#21066=DIRECTION('ref_axis',(0.,0.,-1.));
#21067=DIRECTION('',(0.,1.,0.));
#21068=DIRECTION('',(0.,1.,0.));
#21069=DIRECTION('',(0.,0.,-1.));
#21070=DIRECTION('center_axis',(0.,0.,1.));
#21071=DIRECTION('ref_axis',(1.,0.,0.));
#21072=DIRECTION('',(1.,0.,0.));
#21073=DIRECTION('center_axis',(0.,1.,0.));
#21074=DIRECTION('ref_axis',(0.,0.,1.));
#21075=DIRECTION('center_axis',(0.,1.,0.));
#21076=DIRECTION('ref_axis',(1.,0.,0.));
#21077=DIRECTION('center_axis',(0.,1.,0.));
#21078=DIRECTION('ref_axis',(1.,0.,0.));
#21079=DIRECTION('center_axis',(0.,1.,0.));
#21080=DIRECTION('ref_axis',(1.,0.,0.));
#21081=DIRECTION('center_axis',(0.,1.,0.));
#21082=DIRECTION('ref_axis',(1.,0.,0.));
#21083=DIRECTION('center_axis',(0.,1.,0.));
#21084=DIRECTION('ref_axis',(1.,0.,0.));
#21085=DIRECTION('center_axis',(0.,1.,0.));
#21086=DIRECTION('ref_axis',(1.,0.,0.));
#21087=DIRECTION('center_axis',(0.,-1.,0.));
#21088=DIRECTION('ref_axis',(1.,0.,0.));
#21089=DIRECTION('center_axis',(0.,1.,0.));
#21090=DIRECTION('ref_axis',(1.,0.,0.));
#21091=DIRECTION('',(0.,-1.,0.));
#21092=DIRECTION('center_axis',(0.,1.,0.));
#21093=DIRECTION('ref_axis',(1.,0.,0.));
#21094=DIRECTION('',(0.,-1.,0.));
#21095=DIRECTION('center_axis',(0.,1.,0.));
#21096=DIRECTION('ref_axis',(1.,0.,0.));
#21097=DIRECTION('center_axis',(0.,1.,0.));
#21098=DIRECTION('ref_axis',(1.,0.,0.));
#21099=DIRECTION('center_axis',(0.,1.,0.));
#21100=DIRECTION('ref_axis',(1.,0.,0.));
#21101=DIRECTION('',(0.,-1.,0.));
#21102=DIRECTION('center_axis',(0.,1.,0.));
#21103=DIRECTION('ref_axis',(1.,0.,0.));
#21104=DIRECTION('center_axis',(0.,1.,0.));
#21105=DIRECTION('ref_axis',(1.,0.,0.));
#21106=DIRECTION('axis',(0.,0.,1.));
#21107=DIRECTION('refdir',(1.,0.,0.));
#21108=DIRECTION('center_axis',(0.,1.,0.));
#21109=DIRECTION('ref_axis',(1.,0.,0.));
#21110=DIRECTION('center_axis',(0.,-1.,0.));
#21111=DIRECTION('ref_axis',(1.,0.,0.));
#21112=DIRECTION('',(0.,-1.,0.));
#21113=DIRECTION('center_axis',(0.,-1.,0.));
#21114=DIRECTION('ref_axis',(1.,0.,0.));
#21115=DIRECTION('center_axis',(0.,1.,0.));
#21116=DIRECTION('ref_axis',(1.,0.,0.));
#21117=DIRECTION('center_axis',(0.,1.,0.));
#21118=DIRECTION('ref_axis',(1.,0.,0.));
#21119=DIRECTION('',(0.,-1.,0.));
#21120=DIRECTION('center_axis',(0.,1.,0.));
#21121=DIRECTION('ref_axis',(1.,0.,0.));
#21122=DIRECTION('center_axis',(0.,1.,0.));
#21123=DIRECTION('ref_axis',(1.,0.,0.));
#21124=DIRECTION('center_axis',(0.,1.,0.));
#21125=DIRECTION('ref_axis',(1.,0.,0.));
#21126=DIRECTION('axis',(0.,0.,1.));
#21127=DIRECTION('refdir',(1.,0.,0.));
#21128=DIRECTION('center_axis',(0.,1.,0.));
#21129=DIRECTION('ref_axis',(1.,0.,0.));
#21130=DIRECTION('center_axis',(0.,-1.,0.));
#21131=DIRECTION('ref_axis',(1.,0.,0.));
#21132=DIRECTION('',(0.,-1.,0.));
#21133=DIRECTION('center_axis',(0.,-1.,0.));
#21134=DIRECTION('ref_axis',(1.,0.,0.));
#21135=DIRECTION('center_axis',(0.,1.,0.));
#21136=DIRECTION('ref_axis',(1.,0.,0.));
#21137=DIRECTION('center_axis',(0.,1.,0.));
#21138=DIRECTION('ref_axis',(1.,0.,0.));
#21139=DIRECTION('',(0.,-1.,0.));
#21140=DIRECTION('center_axis',(0.,1.,0.));
#21141=DIRECTION('ref_axis',(1.,0.,0.));
#21142=DIRECTION('center_axis',(0.,1.,0.));
#21143=DIRECTION('ref_axis',(1.,0.,0.));
#21144=DIRECTION('center_axis',(0.,1.,0.));
#21145=DIRECTION('ref_axis',(1.,0.,0.));
#21146=DIRECTION('axis',(0.,0.,1.));
#21147=DIRECTION('refdir',(1.,0.,0.));
#21148=DIRECTION('center_axis',(0.,0.,1.));
#21149=DIRECTION('ref_axis',(1.,0.,0.));
#21150=DIRECTION('',(0.,1.,0.));
#21151=DIRECTION('center_axis',(0.,0.,1.));
#21152=DIRECTION('ref_axis',(1.,0.,0.));
#21153=DIRECTION('center_axis',(0.,0.,1.));
#21154=DIRECTION('ref_axis',(1.,0.,0.));
#21155=DIRECTION('center_axis',(0.,0.,1.));
#21156=DIRECTION('ref_axis',(1.,0.,0.));
#21157=DIRECTION('',(0.,0.,1.));
#21158=DIRECTION('center_axis',(0.,0.,1.));
#21159=DIRECTION('ref_axis',(1.,0.,0.));
#21160=DIRECTION('center_axis',(0.,0.,1.));
#21161=DIRECTION('ref_axis',(1.,0.,0.));
#21162=DIRECTION('',(0.,-1.,0.));
#21163=DIRECTION('center_axis',(0.,1.,0.));
#21164=DIRECTION('ref_axis',(1.,0.,0.));
#21165=DIRECTION('center_axis',(0.,-1.,0.));
#21166=DIRECTION('ref_axis',(1.,0.,0.));
#21167=DIRECTION('',(0.,-1.,0.));
#21168=DIRECTION('center_axis',(0.,-1.,0.));
#21169=DIRECTION('ref_axis',(1.,0.,0.));
#21170=DIRECTION('center_axis',(0.,1.,0.));
#21171=DIRECTION('ref_axis',(1.,0.,0.));
#21172=DIRECTION('center_axis',(0.,1.,0.));
#21173=DIRECTION('ref_axis',(1.,0.,0.));
#21174=DIRECTION('',(0.,-1.,0.));
#21175=DIRECTION('center_axis',(0.,1.,0.));
#21176=DIRECTION('ref_axis',(1.,0.,0.));
#21177=DIRECTION('center_axis',(0.,1.,0.));
#21178=DIRECTION('ref_axis',(1.,0.,0.));
#21179=DIRECTION('center_axis',(0.,1.,0.));
#21180=DIRECTION('ref_axis',(1.,0.,0.));
#21181=DIRECTION('axis',(0.,0.,1.));
#21182=DIRECTION('refdir',(1.,0.,0.));
#21183=DIRECTION('center_axis',(0.,1.,0.));
#21184=DIRECTION('ref_axis',(1.,0.,0.));
#21185=DIRECTION('center_axis',(0.,1.,0.));
#21186=DIRECTION('ref_axis',(1.,0.,0.));
#21187=DIRECTION('',(0.,1.,0.));
#21188=DIRECTION('center_axis',(0.,-1.,0.));
#21189=DIRECTION('ref_axis',(1.,0.,0.));
#21190=DIRECTION('center_axis',(-1.,0.,0.));
#21191=DIRECTION('ref_axis',(0.,0.,1.));
#21192=DIRECTION('',(0.,0.,1.));
#21193=DIRECTION('',(0.,1.,0.));
#21194=DIRECTION('',(0.,0.,-1.));
#21195=DIRECTION('',(0.,1.,0.));
#21196=DIRECTION('center_axis',(0.,0.,-1.));
#21197=DIRECTION('ref_axis',(-1.,0.,0.));
#21198=DIRECTION('',(-1.,0.,0.));
#21199=DIRECTION('',(0.,1.,0.));
#21200=DIRECTION('',(1.,0.,0.));
#21201=DIRECTION('center_axis',(1.,0.,0.));
#21202=DIRECTION('ref_axis',(0.,0.,-1.));
#21203=DIRECTION('',(0.,0.,-1.));
#21204=DIRECTION('',(0.,-1.,0.));
#21205=DIRECTION('',(0.,0.,1.));
#21206=DIRECTION('center_axis',(0.,1.,0.));
#21207=DIRECTION('ref_axis',(1.,0.,0.));
#21208=DIRECTION('center_axis',(0.,1.,0.));
#21209=DIRECTION('ref_axis',(1.,0.,0.));
#21210=DIRECTION('center_axis',(0.,-1.,0.));
#21211=DIRECTION('ref_axis',(1.,0.,0.));
#21212=DIRECTION('center_axis',(0.,1.,0.));
#21213=DIRECTION('ref_axis',(-1.83697019872103E-16,0.,1.));
#21214=DIRECTION('center_axis',(0.,-1.,0.));
#21215=DIRECTION('ref_axis',(1.,0.,0.));
#21216=DIRECTION('center_axis',(0.,1.,0.));
#21217=DIRECTION('ref_axis',(6.12323399573677E-17,0.,1.));
#21218=DIRECTION('',(0.,-1.,0.));
#21219=DIRECTION('center_axis',(0.,1.,0.));
#21220=DIRECTION('ref_axis',(1.,0.,0.));
#21221=DIRECTION('',(0.,1.,0.));
#21222=DIRECTION('center_axis',(0.,1.,0.));
#21223=DIRECTION('ref_axis',(1.,0.,0.));
#21224=DIRECTION('center_axis',(0.,1.,0.));
#21225=DIRECTION('ref_axis',(1.,0.,0.));
#21226=DIRECTION('',(0.,0.,-1.));
#21227=DIRECTION('center_axis',(0.,-1.,0.));
#21228=DIRECTION('ref_axis',(1.,0.,0.));
#21229=DIRECTION('',(0.,0.,1.));
#21230=DIRECTION('center_axis',(-1.,0.,0.));
#21231=DIRECTION('ref_axis',(0.,0.,1.));
#21232=DIRECTION('',(0.,0.,1.));
#21233=DIRECTION('',(0.,1.,0.));
#21234=DIRECTION('center_axis',(0.,1.,0.));
#21235=DIRECTION('ref_axis',(0.,0.,1.));
#21236=DIRECTION('',(0.,0.,-1.));
#21237=DIRECTION('center_axis',(0.,1.,0.));
#21238=DIRECTION('ref_axis',(1.,0.,0.));
#21239=DIRECTION('center_axis',(1.,0.,0.));
#21240=DIRECTION('ref_axis',(0.,0.,-1.));
#21241=DIRECTION('',(0.,-1.,0.));
#21242=DIRECTION('center_axis',(0.,1.,0.));
#21243=DIRECTION('ref_axis',(1.,0.,0.));
#21244=DIRECTION('',(0.,-1.,0.));
#21245=DIRECTION('center_axis',(0.,1.,0.));
#21246=DIRECTION('ref_axis',(1.,0.,0.));
#21247=DIRECTION('center_axis',(0.,1.,0.));
#21248=DIRECTION('ref_axis',(1.,0.,0.));
#21249=DIRECTION('axis',(0.,0.,1.));
#21250=DIRECTION('refdir',(1.,0.,0.));
#21251=DIRECTION('center_axis',(0.,1.,0.));
#21252=DIRECTION('ref_axis',(1.,0.,0.));
#21253=DIRECTION('center_axis',(0.,-1.,0.));
#21254=DIRECTION('ref_axis',(1.,0.,0.));
#21255=DIRECTION('',(0.,-1.,0.));
#21256=DIRECTION('center_axis',(0.,-1.,0.));
#21257=DIRECTION('ref_axis',(1.,0.,0.));
#21258=DIRECTION('center_axis',(0.,1.,0.));
#21259=DIRECTION('ref_axis',(1.,0.,0.));
#21260=DIRECTION('center_axis',(0.,1.,0.));
#21261=DIRECTION('ref_axis',(1.,0.,0.));
#21262=DIRECTION('',(0.,-1.,0.));
#21263=DIRECTION('center_axis',(0.,1.,0.));
#21264=DIRECTION('ref_axis',(1.,0.,0.));
#21265=DIRECTION('center_axis',(0.,1.,0.));
#21266=DIRECTION('ref_axis',(1.,0.,0.));
#21267=DIRECTION('center_axis',(0.,1.,0.));
#21268=DIRECTION('ref_axis',(1.,0.,0.));
#21269=DIRECTION('axis',(0.,0.,1.));
#21270=DIRECTION('refdir',(1.,0.,0.));
#21271=DIRECTION('center_axis',(0.,1.,0.));
#21272=DIRECTION('ref_axis',(1.,0.,0.));
#21273=DIRECTION('center_axis',(0.,-1.,0.));
#21274=DIRECTION('ref_axis',(1.,0.,0.));
#21275=DIRECTION('',(0.,-1.,0.));
#21276=DIRECTION('center_axis',(0.,-1.,0.));
#21277=DIRECTION('ref_axis',(1.,0.,0.));
#21278=DIRECTION('center_axis',(0.,1.,0.));
#21279=DIRECTION('ref_axis',(1.,0.,0.));
#21280=DIRECTION('center_axis',(0.,1.,0.));
#21281=DIRECTION('ref_axis',(1.,0.,0.));
#21282=DIRECTION('',(0.,-1.,0.));
#21283=DIRECTION('center_axis',(0.,1.,0.));
#21284=DIRECTION('ref_axis',(1.,0.,0.));
#21285=DIRECTION('center_axis',(0.,1.,0.));
#21286=DIRECTION('ref_axis',(1.,0.,0.));
#21287=DIRECTION('center_axis',(0.,1.,0.));
#21288=DIRECTION('ref_axis',(1.,0.,0.));
#21289=DIRECTION('axis',(0.,0.,1.));
#21290=DIRECTION('refdir',(1.,0.,0.));
#21291=DIRECTION('center_axis',(0.,1.,0.));
#21292=DIRECTION('ref_axis',(1.,0.,0.));
#21293=DIRECTION('center_axis',(0.,-1.,0.));
#21294=DIRECTION('ref_axis',(1.,0.,0.));
#21295=DIRECTION('',(0.,-1.,0.));
#21296=DIRECTION('center_axis',(0.,-1.,0.));
#21297=DIRECTION('ref_axis',(1.,0.,0.));
#21298=DIRECTION('center_axis',(0.,1.,0.));
#21299=DIRECTION('ref_axis',(1.,0.,0.));
#21300=DIRECTION('center_axis',(0.,1.,0.));
#21301=DIRECTION('ref_axis',(1.,0.,0.));
#21302=DIRECTION('',(0.,-1.,0.));
#21303=DIRECTION('center_axis',(0.,1.,0.));
#21304=DIRECTION('ref_axis',(1.,0.,0.));
#21305=DIRECTION('center_axis',(0.,1.,0.));
#21306=DIRECTION('ref_axis',(1.,0.,0.));
#21307=DIRECTION('center_axis',(0.,1.,0.));
#21308=DIRECTION('ref_axis',(1.,0.,0.));
#21309=DIRECTION('axis',(0.,0.,1.));
#21310=DIRECTION('refdir',(1.,0.,0.));
#21311=DIRECTION('center_axis',(0.,1.,0.));
#21312=DIRECTION('ref_axis',(1.,0.,0.));
#21313=DIRECTION('center_axis',(0.,-1.,0.));
#21314=DIRECTION('ref_axis',(1.,0.,0.));
#21315=DIRECTION('',(0.,-1.,0.));
#21316=DIRECTION('center_axis',(0.,-1.,0.));
#21317=DIRECTION('ref_axis',(1.,0.,0.));
#21318=DIRECTION('center_axis',(0.,1.,0.));
#21319=DIRECTION('ref_axis',(1.,0.,0.));
#21320=DIRECTION('center_axis',(0.,1.,0.));
#21321=DIRECTION('ref_axis',(1.,0.,0.));
#21322=DIRECTION('',(0.,-1.,0.));
#21323=DIRECTION('center_axis',(0.,1.,0.));
#21324=DIRECTION('ref_axis',(1.,0.,0.));
#21325=DIRECTION('center_axis',(0.,1.,0.));
#21326=DIRECTION('ref_axis',(1.,0.,0.));
#21327=DIRECTION('center_axis',(0.,1.,0.));
#21328=DIRECTION('ref_axis',(1.,0.,0.));
#21329=DIRECTION('axis',(0.,0.,1.));
#21330=DIRECTION('refdir',(1.,0.,0.));
#21331=DIRECTION('center_axis',(0.,1.,0.));
#21332=DIRECTION('ref_axis',(1.,0.,0.));
#21333=DIRECTION('center_axis',(0.,-1.,0.));
#21334=DIRECTION('ref_axis',(1.,0.,0.));
#21335=DIRECTION('',(0.,-1.,0.));
#21336=DIRECTION('center_axis',(0.,-1.,0.));
#21337=DIRECTION('ref_axis',(1.,0.,0.));
#21338=DIRECTION('center_axis',(0.,1.,0.));
#21339=DIRECTION('ref_axis',(1.,0.,0.));
#21340=DIRECTION('center_axis',(0.,1.,0.));
#21341=DIRECTION('ref_axis',(1.,0.,0.));
#21342=DIRECTION('',(0.,-1.,0.));
#21343=DIRECTION('center_axis',(0.,1.,0.));
#21344=DIRECTION('ref_axis',(1.,0.,0.));
#21345=DIRECTION('center_axis',(0.,1.,0.));
#21346=DIRECTION('ref_axis',(1.,0.,0.));
#21347=DIRECTION('center_axis',(0.,1.,0.));
#21348=DIRECTION('ref_axis',(1.,0.,0.));
#21349=DIRECTION('axis',(0.,0.,1.));
#21350=DIRECTION('refdir',(1.,0.,0.));
#21351=DIRECTION('center_axis',(0.866025403784439,0.,-0.5));
#21352=DIRECTION('ref_axis',(0.5,0.,0.866025403784439));
#21353=DIRECTION('',(-0.5,0.,-0.866025403784439));
#21354=DIRECTION('',(0.,-1.,0.));
#21355=DIRECTION('',(0.5,0.,0.866025403784439));
#21356=DIRECTION('',(0.,-1.,0.));
#21357=DIRECTION('center_axis',(1.92296268638356E-16,0.,-1.));
#21358=DIRECTION('ref_axis',(1.,0.,1.92296268638356E-16));
#21359=DIRECTION('',(-1.,0.,-1.92296268638356E-16));
#21360=DIRECTION('',(0.,-1.,0.));
#21361=DIRECTION('',(1.,0.,1.92296268638356E-16));
#21362=DIRECTION('center_axis',(-0.866025403784439,0.,-0.5));
#21363=DIRECTION('ref_axis',(0.5,0.,-0.866025403784439));
#21364=DIRECTION('',(-0.5,0.,0.866025403784438));
#21365=DIRECTION('',(0.,-1.,0.));
#21366=DIRECTION('',(0.5,0.,-0.866025403784438));
#21367=DIRECTION('center_axis',(-0.866025403784439,0.,0.5));
#21368=DIRECTION('ref_axis',(-0.5,0.,-0.866025403784439));
#21369=DIRECTION('',(0.5,0.,0.866025403784439));
#21370=DIRECTION('',(0.,-1.,0.));
#21371=DIRECTION('',(-0.5,0.,-0.866025403784439));
#21372=DIRECTION('center_axis',(-1.92296268638356E-16,0.,1.));
#21373=DIRECTION('ref_axis',(-1.,0.,-1.92296268638356E-16));
#21374=DIRECTION('',(1.,0.,1.92296268638356E-16));
#21375=DIRECTION('',(0.,-1.,0.));
#21376=DIRECTION('',(-1.,0.,-1.92296268638356E-16));
#21377=DIRECTION('center_axis',(0.866025403784439,0.,0.5));
#21378=DIRECTION('ref_axis',(-0.5,0.,0.866025403784439));
#21379=DIRECTION('',(0.5,0.,-0.866025403784439));
#21380=DIRECTION('',(-0.5,0.,0.866025403784439));
#21381=DIRECTION('center_axis',(0.,1.,0.));
#21382=DIRECTION('ref_axis',(1.,0.,0.));
#21383=DIRECTION('center_axis',(0.,-1.,0.));
#21384=DIRECTION('ref_axis',(0.,0.,-1.));
#21385=DIRECTION('center_axis',(0.,1.,0.));
#21386=DIRECTION('ref_axis',(1.,0.,0.));
#21387=DIRECTION('center_axis',(0.,1.,0.));
#21388=DIRECTION('ref_axis',(1.,0.,0.));
#21389=DIRECTION('center_axis',(0.,1.,0.));
#21390=DIRECTION('ref_axis',(1.,0.,0.));
#21391=DIRECTION('center_axis',(0.,1.,0.));
#21392=DIRECTION('ref_axis',(1.,0.,0.));
#21393=DIRECTION('',(0.,-1.,0.));
#21394=DIRECTION('center_axis',(0.,1.,0.));
#21395=DIRECTION('ref_axis',(1.,0.,0.));
#21396=DIRECTION('center_axis',(0.,1.,0.));
#21397=DIRECTION('ref_axis',(1.,0.,0.));
#21398=DIRECTION('center_axis',(0.,1.,0.));
#21399=DIRECTION('ref_axis',(0.,0.,1.));
#21400=DIRECTION('center_axis',(0.,-1.,0.));
#21401=DIRECTION('ref_axis',(1.,0.,0.));
#21402=DIRECTION('center_axis',(0.,-1.,0.));
#21403=DIRECTION('ref_axis',(1.,0.,0.));
#21404=DIRECTION('center_axis',(0.,-1.,0.));
#21405=DIRECTION('ref_axis',(1.,0.,0.));
#21406=DIRECTION('',(0.707106781186548,0.707106781186547,8.65956056235494E-17));
#21407=DIRECTION('center_axis',(0.,-1.,0.));
#21408=DIRECTION('ref_axis',(1.,0.,0.));
#21409=DIRECTION('center_axis',(0.,-1.,0.));
#21410=DIRECTION('ref_axis',(1.,0.,0.));
#21411=DIRECTION('',(0.,1.,0.));
#21412=DIRECTION('center_axis',(0.,1.,0.));
#21413=DIRECTION('ref_axis',(1.,0.,0.));
#21414=DIRECTION('center_axis',(0.,-1.,0.));
#21415=DIRECTION('ref_axis',(1.,0.,0.));
#21416=DIRECTION('',(-0.707106781186547,0.707106781186548,-8.65956056235493E-17));
#21417=DIRECTION('center_axis',(0.,-1.,0.));
#21418=DIRECTION('ref_axis',(0.,0.,-1.));
#21419=DIRECTION('center_axis',(0.,-1.,0.));
#21420=DIRECTION('ref_axis',(1.,0.,0.));
#21421=DIRECTION('center_axis',(0.,1.,0.));
#21422=DIRECTION('ref_axis',(1.,0.,0.));
#21423=DIRECTION('center_axis',(0.,1.,0.));
#21424=DIRECTION('ref_axis',(1.,0.,0.));
#21425=DIRECTION('',(-0.447213595499958,0.894427190999916,-5.47678698264203E-17));
#21426=DIRECTION('center_axis',(0.,-1.,0.));
#21427=DIRECTION('ref_axis',(1.,0.,0.));
#21428=DIRECTION('',(0.,1.,0.));
#21429=DIRECTION('axis',(0.,0.,1.));
#21430=DIRECTION('refdir',(1.,0.,0.));
#21431=DIRECTION('axis',(0.,0.,1.));
#21432=DIRECTION('refdir',(1.,0.,0.));
#21433=DIRECTION('center_axis',(0.,1.,0.));
#21434=DIRECTION('ref_axis',(1.,0.,0.));
#21435=DIRECTION('center_axis',(0.,1.,0.));
#21436=DIRECTION('ref_axis',(1.,0.,0.));
#21437=DIRECTION('',(0.,1.,0.));
#21438=DIRECTION('center_axis',(0.,-1.,0.));
#21439=DIRECTION('ref_axis',(1.,0.,0.));
#21440=DIRECTION('center_axis',(0.,1.,0.));
#21441=DIRECTION('ref_axis',(1.,0.,0.));
#21442=DIRECTION('center_axis',(-1.,0.,0.));
#21443=DIRECTION('ref_axis',(0.,0.,1.));
#21444=DIRECTION('',(0.,-1.,0.));
#21445=DIRECTION('',(0.,0.,1.));
#21446=DIRECTION('',(0.,1.,0.));
#21447=DIRECTION('',(0.,0.,-1.));
#21448=DIRECTION('center_axis',(0.,1.,0.));
#21449=DIRECTION('ref_axis',(1.,0.,0.));
#21450=DIRECTION('center_axis',(0.,-1.,0.));
#21451=DIRECTION('ref_axis',(1.,0.,0.));
#21452=DIRECTION('',(-1.,0.,0.));
#21453=DIRECTION('',(0.,0.,1.));
#21454=DIRECTION('center_axis',(1.,0.,0.));
#21455=DIRECTION('ref_axis',(0.,0.,-1.));
#21456=DIRECTION('',(0.,1.,0.));
#21457=DIRECTION('',(0.,1.,0.));
#21458=DIRECTION('',(0.,0.,-1.));
#21459=DIRECTION('center_axis',(0.,0.,1.));
#21460=DIRECTION('ref_axis',(1.,0.,0.));
#21461=DIRECTION('',(1.,0.,0.));
#21462=DIRECTION('center_axis',(0.,1.,0.));
#21463=DIRECTION('ref_axis',(0.,0.,1.));
#21464=DIRECTION('center_axis',(0.,1.,0.));
#21465=DIRECTION('ref_axis',(1.,0.,0.));
#21466=DIRECTION('center_axis',(0.,1.,0.));
#21467=DIRECTION('ref_axis',(1.,0.,0.));
#21468=DIRECTION('center_axis',(0.,1.,0.));
#21469=DIRECTION('ref_axis',(1.,0.,0.));
#21470=DIRECTION('center_axis',(0.,1.,0.));
#21471=DIRECTION('ref_axis',(1.,0.,0.));
#21472=DIRECTION('center_axis',(0.,1.,0.));
#21473=DIRECTION('ref_axis',(1.,0.,0.));
#21474=DIRECTION('center_axis',(0.,1.,0.));
#21475=DIRECTION('ref_axis',(1.,0.,0.));
#21476=DIRECTION('center_axis',(0.,-1.,0.));
#21477=DIRECTION('ref_axis',(1.,0.,0.));
#21478=DIRECTION('center_axis',(0.,1.,0.));
#21479=DIRECTION('ref_axis',(1.,0.,0.));
#21480=DIRECTION('',(0.,-1.,0.));
#21481=DIRECTION('center_axis',(0.,1.,0.));
#21482=DIRECTION('ref_axis',(1.,0.,0.));
#21483=DIRECTION('',(0.,-1.,0.));
#21484=DIRECTION('center_axis',(0.,1.,0.));
#21485=DIRECTION('ref_axis',(1.,0.,0.));
#21486=DIRECTION('center_axis',(0.,1.,0.));
#21487=DIRECTION('ref_axis',(1.,0.,0.));
#21488=DIRECTION('center_axis',(0.,1.,0.));
#21489=DIRECTION('ref_axis',(1.,0.,0.));
#21490=DIRECTION('',(0.,-1.,0.));
#21491=DIRECTION('center_axis',(0.,1.,0.));
#21492=DIRECTION('ref_axis',(1.,0.,0.));
#21493=DIRECTION('center_axis',(0.,1.,0.));
#21494=DIRECTION('ref_axis',(1.,0.,0.));
#21495=DIRECTION('axis',(0.,0.,1.));
#21496=DIRECTION('refdir',(1.,0.,0.));
#21497=DIRECTION('center_axis',(0.,1.,0.));
#21498=DIRECTION('ref_axis',(1.,0.,0.));
#21499=DIRECTION('center_axis',(0.,-1.,0.));
#21500=DIRECTION('ref_axis',(1.,0.,0.));
#21501=DIRECTION('',(0.,-1.,0.));
#21502=DIRECTION('center_axis',(0.,-1.,0.));
#21503=DIRECTION('ref_axis',(1.,0.,0.));
#21504=DIRECTION('center_axis',(0.,1.,0.));
#21505=DIRECTION('ref_axis',(1.,0.,0.));
#21506=DIRECTION('center_axis',(0.,1.,0.));
#21507=DIRECTION('ref_axis',(1.,0.,0.));
#21508=DIRECTION('',(0.,-1.,0.));
#21509=DIRECTION('center_axis',(0.,1.,0.));
#21510=DIRECTION('ref_axis',(1.,0.,0.));
#21511=DIRECTION('center_axis',(0.,1.,0.));
#21512=DIRECTION('ref_axis',(1.,0.,0.));
#21513=DIRECTION('center_axis',(0.,1.,0.));
#21514=DIRECTION('ref_axis',(1.,0.,0.));
#21515=DIRECTION('axis',(0.,0.,1.));
#21516=DIRECTION('refdir',(1.,0.,0.));
#21517=DIRECTION('center_axis',(0.,1.,0.));
#21518=DIRECTION('ref_axis',(1.,0.,0.));
#21519=DIRECTION('center_axis',(0.,-1.,0.));
#21520=DIRECTION('ref_axis',(1.,0.,0.));
#21521=DIRECTION('',(0.,-1.,0.));
#21522=DIRECTION('center_axis',(0.,-1.,0.));
#21523=DIRECTION('ref_axis',(1.,0.,0.));
#21524=DIRECTION('center_axis',(0.,1.,0.));
#21525=DIRECTION('ref_axis',(1.,0.,0.));
#21526=DIRECTION('center_axis',(0.,1.,0.));
#21527=DIRECTION('ref_axis',(1.,0.,0.));
#21528=DIRECTION('',(0.,-1.,0.));
#21529=DIRECTION('center_axis',(0.,1.,0.));
#21530=DIRECTION('ref_axis',(1.,0.,0.));
#21531=DIRECTION('center_axis',(0.,1.,0.));
#21532=DIRECTION('ref_axis',(1.,0.,0.));
#21533=DIRECTION('center_axis',(0.,1.,0.));
#21534=DIRECTION('ref_axis',(1.,0.,0.));
#21535=DIRECTION('axis',(0.,0.,1.));
#21536=DIRECTION('refdir',(1.,0.,0.));
#21537=DIRECTION('center_axis',(0.,0.,1.));
#21538=DIRECTION('ref_axis',(1.,0.,0.));
#21539=DIRECTION('',(0.,1.,0.));
#21540=DIRECTION('center_axis',(0.,0.,1.));
#21541=DIRECTION('ref_axis',(1.,0.,0.));
#21542=DIRECTION('center_axis',(0.,0.,1.));
#21543=DIRECTION('ref_axis',(1.,0.,0.));
#21544=DIRECTION('center_axis',(0.,0.,1.));
#21545=DIRECTION('ref_axis',(1.,0.,0.));
#21546=DIRECTION('',(0.,0.,1.));
#21547=DIRECTION('center_axis',(0.,0.,1.));
#21548=DIRECTION('ref_axis',(1.,0.,0.));
#21549=DIRECTION('center_axis',(0.,0.,1.));
#21550=DIRECTION('ref_axis',(1.,0.,0.));
#21551=DIRECTION('',(0.,-1.,0.));
#21552=DIRECTION('center_axis',(0.,1.,0.));
#21553=DIRECTION('ref_axis',(1.,0.,0.));
#21554=DIRECTION('center_axis',(0.,-1.,0.));
#21555=DIRECTION('ref_axis',(1.,0.,0.));
#21556=DIRECTION('',(0.,-1.,0.));
#21557=DIRECTION('center_axis',(0.,-1.,0.));
#21558=DIRECTION('ref_axis',(1.,0.,0.));
#21559=DIRECTION('center_axis',(0.,1.,0.));
#21560=DIRECTION('ref_axis',(1.,0.,0.));
#21561=DIRECTION('center_axis',(0.,1.,0.));
#21562=DIRECTION('ref_axis',(1.,0.,0.));
#21563=DIRECTION('',(0.,-1.,0.));
#21564=DIRECTION('center_axis',(0.,1.,0.));
#21565=DIRECTION('ref_axis',(1.,0.,0.));
#21566=DIRECTION('center_axis',(0.,1.,0.));
#21567=DIRECTION('ref_axis',(1.,0.,0.));
#21568=DIRECTION('center_axis',(0.,1.,0.));
#21569=DIRECTION('ref_axis',(1.,0.,0.));
#21570=DIRECTION('axis',(0.,0.,1.));
#21571=DIRECTION('refdir',(1.,0.,0.));
#21572=DIRECTION('center_axis',(0.,1.,0.));
#21573=DIRECTION('ref_axis',(1.,0.,0.));
#21574=DIRECTION('center_axis',(0.,-1.,0.));
#21575=DIRECTION('ref_axis',(1.,0.,0.));
#21576=DIRECTION('',(0.,-1.,0.));
#21577=DIRECTION('center_axis',(0.,-1.,0.));
#21578=DIRECTION('ref_axis',(1.,0.,0.));
#21579=DIRECTION('center_axis',(0.,1.,0.));
#21580=DIRECTION('ref_axis',(1.,0.,0.));
#21581=DIRECTION('center_axis',(0.,1.,0.));
#21582=DIRECTION('ref_axis',(1.,0.,0.));
#21583=DIRECTION('',(0.,-1.,0.));
#21584=DIRECTION('center_axis',(0.,1.,0.));
#21585=DIRECTION('ref_axis',(1.,0.,0.));
#21586=DIRECTION('center_axis',(0.,1.,0.));
#21587=DIRECTION('ref_axis',(1.,0.,0.));
#21588=DIRECTION('center_axis',(0.,1.,0.));
#21589=DIRECTION('ref_axis',(1.,0.,0.));
#21590=DIRECTION('axis',(0.,0.,1.));
#21591=DIRECTION('refdir',(1.,0.,0.));
#21592=DIRECTION('axis',(0.,0.,1.));
#21593=DIRECTION('refdir',(1.,0.,0.));
#21594=DIRECTION('center_axis',(0.,1.,0.));
#21595=DIRECTION('ref_axis',(1.,0.,0.));
#21596=DIRECTION('center_axis',(0.,1.,0.));
#21597=DIRECTION('ref_axis',(1.,0.,0.));
#21598=DIRECTION('',(0.,1.,0.));
#21599=DIRECTION('center_axis',(0.,-1.,0.));
#21600=DIRECTION('ref_axis',(1.,0.,0.));
#21601=DIRECTION('center_axis',(0.,1.,0.));
#21602=DIRECTION('ref_axis',(1.,0.,0.));
#21603=DIRECTION('center_axis',(-1.,0.,0.));
#21604=DIRECTION('ref_axis',(0.,0.,1.));
#21605=DIRECTION('',(0.,-1.,0.));
#21606=DIRECTION('',(0.,0.,1.));
#21607=DIRECTION('',(0.,1.,0.));
#21608=DIRECTION('',(0.,0.,-1.));
#21609=DIRECTION('center_axis',(0.,1.,0.));
#21610=DIRECTION('ref_axis',(1.,0.,0.));
#21611=DIRECTION('center_axis',(0.,-1.,0.));
#21612=DIRECTION('ref_axis',(1.,0.,0.));
#21613=DIRECTION('',(-1.,0.,0.));
#21614=DIRECTION('',(0.,0.,1.));
#21615=DIRECTION('center_axis',(1.,0.,0.));
#21616=DIRECTION('ref_axis',(0.,0.,-1.));
#21617=DIRECTION('',(0.,1.,0.));
#21618=DIRECTION('',(0.,1.,0.));
#21619=DIRECTION('',(0.,0.,-1.));
#21620=DIRECTION('center_axis',(0.,0.,1.));
#21621=DIRECTION('ref_axis',(1.,0.,0.));
#21622=DIRECTION('',(1.,0.,0.));
#21623=DIRECTION('center_axis',(0.,1.,0.));
#21624=DIRECTION('ref_axis',(0.,0.,1.));
#21625=DIRECTION('center_axis',(0.,1.,0.));
#21626=DIRECTION('ref_axis',(1.,0.,0.));
#21627=DIRECTION('center_axis',(0.,1.,0.));
#21628=DIRECTION('ref_axis',(1.,0.,0.));
#21629=DIRECTION('center_axis',(0.,1.,0.));
#21630=DIRECTION('ref_axis',(1.,0.,0.));
#21631=DIRECTION('center_axis',(0.,1.,0.));
#21632=DIRECTION('ref_axis',(1.,0.,0.));
#21633=DIRECTION('center_axis',(0.,1.,0.));
#21634=DIRECTION('ref_axis',(1.,0.,0.));
#21635=DIRECTION('center_axis',(0.,1.,0.));
#21636=DIRECTION('ref_axis',(1.,0.,0.));
#21637=DIRECTION('center_axis',(0.,-1.,0.));
#21638=DIRECTION('ref_axis',(1.,0.,0.));
#21639=DIRECTION('center_axis',(0.,1.,0.));
#21640=DIRECTION('ref_axis',(1.,0.,0.));
#21641=DIRECTION('',(0.,-1.,0.));
#21642=DIRECTION('center_axis',(0.,1.,0.));
#21643=DIRECTION('ref_axis',(1.,0.,0.));
#21644=DIRECTION('',(0.,-1.,0.));
#21645=DIRECTION('center_axis',(0.,1.,0.));
#21646=DIRECTION('ref_axis',(1.,0.,0.));
#21647=DIRECTION('center_axis',(0.,1.,0.));
#21648=DIRECTION('ref_axis',(1.,0.,0.));
#21649=DIRECTION('center_axis',(0.,1.,0.));
#21650=DIRECTION('ref_axis',(1.,0.,0.));
#21651=DIRECTION('',(0.,-1.,0.));
#21652=DIRECTION('center_axis',(0.,1.,0.));
#21653=DIRECTION('ref_axis',(1.,0.,0.));
#21654=DIRECTION('center_axis',(0.,1.,0.));
#21655=DIRECTION('ref_axis',(1.,0.,0.));
#21656=DIRECTION('axis',(0.,0.,1.));
#21657=DIRECTION('refdir',(1.,0.,0.));
#21658=DIRECTION('center_axis',(0.,1.,0.));
#21659=DIRECTION('ref_axis',(1.,0.,0.));
#21660=DIRECTION('center_axis',(0.,-1.,0.));
#21661=DIRECTION('ref_axis',(1.,0.,0.));
#21662=DIRECTION('',(0.,-1.,0.));
#21663=DIRECTION('center_axis',(0.,-1.,0.));
#21664=DIRECTION('ref_axis',(1.,0.,0.));
#21665=DIRECTION('center_axis',(0.,1.,0.));
#21666=DIRECTION('ref_axis',(1.,0.,0.));
#21667=DIRECTION('center_axis',(0.,1.,0.));
#21668=DIRECTION('ref_axis',(1.,0.,0.));
#21669=DIRECTION('',(0.,-1.,0.));
#21670=DIRECTION('center_axis',(0.,1.,0.));
#21671=DIRECTION('ref_axis',(1.,0.,0.));
#21672=DIRECTION('center_axis',(0.,1.,0.));
#21673=DIRECTION('ref_axis',(1.,0.,0.));
#21674=DIRECTION('center_axis',(0.,1.,0.));
#21675=DIRECTION('ref_axis',(1.,0.,0.));
#21676=DIRECTION('axis',(0.,0.,1.));
#21677=DIRECTION('refdir',(1.,0.,0.));
#21678=DIRECTION('center_axis',(0.,1.,0.));
#21679=DIRECTION('ref_axis',(1.,0.,0.));
#21680=DIRECTION('center_axis',(0.,-1.,0.));
#21681=DIRECTION('ref_axis',(1.,0.,0.));
#21682=DIRECTION('',(0.,-1.,0.));
#21683=DIRECTION('center_axis',(0.,-1.,0.));
#21684=DIRECTION('ref_axis',(1.,0.,0.));
#21685=DIRECTION('center_axis',(0.,1.,0.));
#21686=DIRECTION('ref_axis',(1.,0.,0.));
#21687=DIRECTION('center_axis',(0.,1.,0.));
#21688=DIRECTION('ref_axis',(1.,0.,0.));
#21689=DIRECTION('',(0.,-1.,0.));
#21690=DIRECTION('center_axis',(0.,1.,0.));
#21691=DIRECTION('ref_axis',(1.,0.,0.));
#21692=DIRECTION('center_axis',(0.,1.,0.));
#21693=DIRECTION('ref_axis',(1.,0.,0.));
#21694=DIRECTION('center_axis',(0.,1.,0.));
#21695=DIRECTION('ref_axis',(1.,0.,0.));
#21696=DIRECTION('axis',(0.,0.,1.));
#21697=DIRECTION('refdir',(1.,0.,0.));
#21698=DIRECTION('center_axis',(0.,0.,1.));
#21699=DIRECTION('ref_axis',(1.,0.,0.));
#21700=DIRECTION('',(0.,1.,0.));
#21701=DIRECTION('center_axis',(0.,0.,1.));
#21702=DIRECTION('ref_axis',(1.,0.,0.));
#21703=DIRECTION('center_axis',(0.,0.,1.));
#21704=DIRECTION('ref_axis',(1.,0.,0.));
#21705=DIRECTION('center_axis',(0.,0.,1.));
#21706=DIRECTION('ref_axis',(1.,0.,0.));
#21707=DIRECTION('',(0.,0.,1.));
#21708=DIRECTION('center_axis',(0.,0.,1.));
#21709=DIRECTION('ref_axis',(1.,0.,0.));
#21710=DIRECTION('center_axis',(0.,0.,1.));
#21711=DIRECTION('ref_axis',(1.,0.,0.));
#21712=DIRECTION('',(0.,-1.,0.));
#21713=DIRECTION('center_axis',(0.,1.,0.));
#21714=DIRECTION('ref_axis',(1.,0.,0.));
#21715=DIRECTION('center_axis',(0.,-1.,0.));
#21716=DIRECTION('ref_axis',(1.,0.,0.));
#21717=DIRECTION('',(0.,-1.,0.));
#21718=DIRECTION('center_axis',(0.,-1.,0.));
#21719=DIRECTION('ref_axis',(1.,0.,0.));
#21720=DIRECTION('center_axis',(0.,1.,0.));
#21721=DIRECTION('ref_axis',(1.,0.,0.));
#21722=DIRECTION('center_axis',(0.,1.,0.));
#21723=DIRECTION('ref_axis',(1.,0.,0.));
#21724=DIRECTION('',(0.,-1.,0.));
#21725=DIRECTION('center_axis',(0.,1.,0.));
#21726=DIRECTION('ref_axis',(1.,0.,0.));
#21727=DIRECTION('center_axis',(0.,1.,0.));
#21728=DIRECTION('ref_axis',(1.,0.,0.));
#21729=DIRECTION('center_axis',(0.,1.,0.));
#21730=DIRECTION('ref_axis',(1.,0.,0.));
#21731=DIRECTION('axis',(0.,0.,1.));
#21732=DIRECTION('refdir',(1.,0.,0.));
#21733=DIRECTION('center_axis',(0.,1.,0.));
#21734=DIRECTION('ref_axis',(1.,0.,0.));
#21735=DIRECTION('center_axis',(0.,-1.,0.));
#21736=DIRECTION('ref_axis',(1.,0.,0.));
#21737=DIRECTION('',(0.,-1.,0.));
#21738=DIRECTION('center_axis',(0.,-1.,0.));
#21739=DIRECTION('ref_axis',(1.,0.,0.));
#21740=DIRECTION('center_axis',(0.,1.,0.));
#21741=DIRECTION('ref_axis',(1.,0.,0.));
#21742=DIRECTION('center_axis',(0.,1.,0.));
#21743=DIRECTION('ref_axis',(1.,0.,0.));
#21744=DIRECTION('',(0.,-1.,0.));
#21745=DIRECTION('center_axis',(0.,1.,0.));
#21746=DIRECTION('ref_axis',(1.,0.,0.));
#21747=DIRECTION('center_axis',(0.,1.,0.));
#21748=DIRECTION('ref_axis',(1.,0.,0.));
#21749=DIRECTION('center_axis',(0.,1.,0.));
#21750=DIRECTION('ref_axis',(1.,0.,0.));
#21751=DIRECTION('axis',(0.,0.,1.));
#21752=DIRECTION('refdir',(1.,0.,0.));
#21753=DIRECTION('center_axis',(1.,0.,0.));
#21754=DIRECTION('ref_axis',(0.,0.,-1.));
#21755=DIRECTION('',(0.,0.,1.));
#21756=DIRECTION('',(0.,1.,0.));
#21757=DIRECTION('',(0.,0.,-1.));
#21758=DIRECTION('',(0.,-1.,0.));
#21759=DIRECTION('center_axis',(0.,0.,-1.));
#21760=DIRECTION('ref_axis',(-1.,0.,0.));
#21761=DIRECTION('',(1.,0.,0.));
#21762=DIRECTION('',(0.,-1.,0.));
#21763=DIRECTION('',(-1.,0.,0.));
#21764=DIRECTION('center_axis',(-1.,0.,0.));
#21765=DIRECTION('ref_axis',(0.,0.,1.));
#21766=DIRECTION('',(0.,0.,-1.));
#21767=DIRECTION('',(0.,1.,0.));
#21768=DIRECTION('',(0.,0.,1.));
#21769=DIRECTION('center_axis',(0.,1.,0.));
#21770=DIRECTION('ref_axis',(1.,0.,0.));
#21771=DIRECTION('center_axis',(0.,-1.,0.));
#21772=DIRECTION('ref_axis',(1.,0.,0.));
#21773=DIRECTION('',(-0.587785252292473,0.,0.809016994374947));
#21774=DIRECTION('center_axis',(0.,-1.,0.));
#21775=DIRECTION('ref_axis',(1.,0.,0.));
#21776=DIRECTION('',(-0.809016994374948,0.,0.587785252292473));
#21777=DIRECTION('center_axis',(0.,-1.,0.));
#21778=DIRECTION('ref_axis',(1.,0.,0.));
#21779=DIRECTION('',(-0.951056516295154,0.,0.309016994374947));
#21780=DIRECTION('center_axis',(0.,-1.,0.));
#21781=DIRECTION('ref_axis',(1.,0.,0.));
#21782=DIRECTION('',(-1.,0.,-1.83697019872103E-16));
#21783=DIRECTION('center_axis',(0.,-1.,0.));
#21784=DIRECTION('ref_axis',(1.,0.,0.));
#21785=DIRECTION('',(-0.951056516295154,0.,-0.309016994374948));
#21786=DIRECTION('center_axis',(0.,-1.,0.));
#21787=DIRECTION('ref_axis',(1.,0.,0.));
#21788=DIRECTION('',(-0.809016994374947,0.,-0.587785252292473));
#21789=DIRECTION('center_axis',(0.,-1.,0.));
#21790=DIRECTION('ref_axis',(1.,0.,0.));
#21791=DIRECTION('',(-0.587785252292473,0.,-0.809016994374948));
#21792=DIRECTION('center_axis',(0.,-1.,0.));
#21793=DIRECTION('ref_axis',(1.,0.,0.));
#21794=DIRECTION('',(-0.309016994374947,0.,-0.951056516295154));
#21795=DIRECTION('center_axis',(0.,-1.,0.));
#21796=DIRECTION('ref_axis',(1.,0.,0.));
#21797=DIRECTION('',(1.22464679914735E-16,0.,-1.));
#21798=DIRECTION('center_axis',(0.,-1.,0.));
#21799=DIRECTION('ref_axis',(1.,0.,0.));
#21800=DIRECTION('',(0.309016994374948,0.,-0.951056516295154));
#21801=DIRECTION('center_axis',(0.,-1.,0.));
#21802=DIRECTION('ref_axis',(1.,0.,0.));
#21803=DIRECTION('',(0.587785252292473,0.,-0.809016994374947));
#21804=DIRECTION('center_axis',(0.,-1.,0.));
#21805=DIRECTION('ref_axis',(1.,0.,0.));
#21806=DIRECTION('',(0.809016994374948,0.,-0.587785252292473));
#21807=DIRECTION('center_axis',(0.,-1.,0.));
#21808=DIRECTION('ref_axis',(1.,0.,0.));
#21809=DIRECTION('',(0.951056516295154,0.,-0.309016994374947));
#21810=DIRECTION('center_axis',(0.,-1.,0.));
#21811=DIRECTION('ref_axis',(1.,0.,0.));
#21812=DIRECTION('',(1.,0.,6.12323399573677E-17));
#21813=DIRECTION('center_axis',(0.,-1.,0.));
#21814=DIRECTION('ref_axis',(1.,0.,0.));
#21815=DIRECTION('',(0.951056516295154,0.,0.309016994374948));
#21816=DIRECTION('center_axis',(0.,-1.,0.));
#21817=DIRECTION('ref_axis',(1.,0.,0.));
#21818=DIRECTION('',(0.809016994374947,0.,0.587785252292473));
#21819=DIRECTION('center_axis',(0.,-1.,0.));
#21820=DIRECTION('ref_axis',(1.,0.,0.));
#21821=DIRECTION('',(0.587785252292473,0.,0.809016994374947));
#21822=DIRECTION('center_axis',(0.,-1.,0.));
#21823=DIRECTION('ref_axis',(1.,0.,0.));
#21824=DIRECTION('',(0.309016994374947,0.,0.951056516295154));
#21825=DIRECTION('center_axis',(0.,-1.,0.));
#21826=DIRECTION('ref_axis',(1.,0.,0.));
#21827=DIRECTION('',(0.,0.,1.));
#21828=DIRECTION('center_axis',(0.,-1.,0.));
#21829=DIRECTION('ref_axis',(1.,0.,0.));
#21830=DIRECTION('',(-0.309016994374948,0.,0.951056516295154));
#21831=DIRECTION('center_axis',(0.,1.,0.));
#21832=DIRECTION('ref_axis',(1.,0.,0.));
#21833=DIRECTION('center_axis',(0.,1.,0.));
#21834=DIRECTION('ref_axis',(6.12323399573677E-17,0.,1.));
#21835=DIRECTION('center_axis',(0.,-1.,0.));
#21836=DIRECTION('ref_axis',(1.,0.,0.));
#21837=DIRECTION('center_axis',(0.,1.,0.));
#21838=DIRECTION('ref_axis',(1.,0.,0.));
#21839=DIRECTION('center_axis',(0.,1.,0.));
#21840=DIRECTION('ref_axis',(1.,0.,0.));
#21841=DIRECTION('',(0.,-1.,0.));
#21842=DIRECTION('center_axis',(0.,-1.,0.));
#21843=DIRECTION('ref_axis',(1.,0.,0.));
#21844=DIRECTION('center_axis',(0.,1.,0.));
#21845=DIRECTION('ref_axis',(1.,0.,0.));
#21846=DIRECTION('',(0.,-1.,0.));
#21847=DIRECTION('',(0.,1.,0.));
#21848=DIRECTION('center_axis',(0.951056516295154,0.,0.309016994374948));
#21849=DIRECTION('ref_axis',(0.309016994374948,0.,-0.951056516295154));
#21850=DIRECTION('',(0.309016994374948,0.,-0.951056516295154));
#21851=DIRECTION('',(0.,1.,0.));
#21852=DIRECTION('',(0.,1.,0.));
#21853=DIRECTION('center_axis',(0.,1.,0.));
#21854=DIRECTION('ref_axis',(1.,0.,0.));
#21855=DIRECTION('center_axis',(0.,1.,0.));
#21856=DIRECTION('ref_axis',(1.,0.,0.));
#21857=DIRECTION('',(0.,-1.,0.));
#21858=DIRECTION('',(0.,1.,0.));
#21859=DIRECTION('center_axis',(0.809016994374947,0.,0.587785252292473));
#21860=DIRECTION('ref_axis',(0.587785252292473,0.,-0.809016994374947));
#21861=DIRECTION('',(0.587785252292473,0.,-0.809016994374947));
#21862=DIRECTION('',(0.,1.,0.));
#21863=DIRECTION('',(0.,1.,0.));
#21864=DIRECTION('center_axis',(0.,1.,0.));
#21865=DIRECTION('ref_axis',(1.,0.,0.));
#21866=DIRECTION('center_axis',(0.,1.,0.));
#21867=DIRECTION('ref_axis',(1.,0.,0.));
#21868=DIRECTION('',(0.,-1.,0.));
#21869=DIRECTION('',(0.,1.,0.));
#21870=DIRECTION('center_axis',(0.587785252292473,0.,0.809016994374948));
#21871=DIRECTION('ref_axis',(0.809016994374948,0.,-0.587785252292473));
#21872=DIRECTION('',(0.809016994374948,0.,-0.587785252292473));
#21873=DIRECTION('',(0.,1.,0.));
#21874=DIRECTION('',(0.,1.,0.));
#21875=DIRECTION('center_axis',(0.,1.,0.));
#21876=DIRECTION('ref_axis',(1.,0.,0.));
#21877=DIRECTION('center_axis',(0.,1.,0.));
#21878=DIRECTION('ref_axis',(1.,0.,0.));
#21879=DIRECTION('',(0.,-1.,0.));
#21880=DIRECTION('',(0.,1.,0.));
#21881=DIRECTION('center_axis',(0.309016994374947,0.,0.951056516295154));
#21882=DIRECTION('ref_axis',(0.951056516295154,0.,-0.309016994374947));
#21883=DIRECTION('',(0.951056516295154,0.,-0.309016994374947));
#21884=DIRECTION('',(0.,1.,0.));
#21885=DIRECTION('',(0.,1.,0.));
#21886=DIRECTION('center_axis',(0.,1.,0.));
#21887=DIRECTION('ref_axis',(1.,0.,0.));
#21888=DIRECTION('center_axis',(0.,1.,0.));
#21889=DIRECTION('ref_axis',(1.,0.,0.));
#21890=DIRECTION('',(0.,-1.,0.));
#21891=DIRECTION('',(0.,1.,0.));
#21892=DIRECTION('center_axis',(-1.83697019872103E-16,0.,1.));
#21893=DIRECTION('ref_axis',(1.,0.,1.83697019872103E-16));
#21894=DIRECTION('',(1.,0.,1.83697019872103E-16));
#21895=DIRECTION('',(0.,1.,0.));
#21896=DIRECTION('',(0.,1.,0.));
#21897=DIRECTION('center_axis',(0.,1.,0.));
#21898=DIRECTION('ref_axis',(1.,0.,0.));
#21899=DIRECTION('center_axis',(0.,1.,0.));
#21900=DIRECTION('ref_axis',(1.,0.,0.));
#21901=DIRECTION('',(0.,-1.,0.));
#21902=DIRECTION('',(0.,1.,0.));
#21903=DIRECTION('center_axis',(-0.309016994374948,0.,0.951056516295154));
#21904=DIRECTION('ref_axis',(0.951056516295154,0.,0.309016994374948));
#21905=DIRECTION('',(0.951056516295154,0.,0.309016994374948));
#21906=DIRECTION('',(0.,1.,0.));
#21907=DIRECTION('',(0.,1.,0.));
#21908=DIRECTION('center_axis',(0.,1.,0.));
#21909=DIRECTION('ref_axis',(1.,0.,0.));
#21910=DIRECTION('center_axis',(0.,1.,0.));
#21911=DIRECTION('ref_axis',(1.,0.,0.));
#21912=DIRECTION('',(0.,-1.,0.));
#21913=DIRECTION('',(0.,1.,0.));
#21914=DIRECTION('center_axis',(-0.587785252292473,0.,0.809016994374947));
#21915=DIRECTION('ref_axis',(0.809016994374947,0.,0.587785252292473));
#21916=DIRECTION('',(0.809016994374947,0.,0.587785252292473));
#21917=DIRECTION('',(0.,1.,0.));
#21918=DIRECTION('',(0.,1.,0.));
#21919=DIRECTION('center_axis',(0.,1.,0.));
#21920=DIRECTION('ref_axis',(1.,0.,0.));
#21921=DIRECTION('center_axis',(0.,1.,0.));
#21922=DIRECTION('ref_axis',(1.,0.,0.));
#21923=DIRECTION('',(0.,-1.,0.));
#21924=DIRECTION('',(0.,1.,0.));
#21925=DIRECTION('center_axis',(-0.809016994374948,0.,0.587785252292473));
#21926=DIRECTION('ref_axis',(0.587785252292473,0.,0.809016994374948));
#21927=DIRECTION('',(0.587785252292473,0.,0.809016994374948));
#21928=DIRECTION('',(0.,1.,0.));
#21929=DIRECTION('',(0.,1.,0.));
#21930=DIRECTION('center_axis',(0.,1.,0.));
#21931=DIRECTION('ref_axis',(1.,0.,0.));
#21932=DIRECTION('center_axis',(0.,1.,0.));
#21933=DIRECTION('ref_axis',(1.,0.,0.));
#21934=DIRECTION('',(0.,-1.,0.));
#21935=DIRECTION('',(0.,1.,0.));
#21936=DIRECTION('center_axis',(-0.951056516295154,0.,0.309016994374947));
#21937=DIRECTION('ref_axis',(0.309016994374947,0.,0.951056516295154));
#21938=DIRECTION('',(0.309016994374947,0.,0.951056516295154));
#21939=DIRECTION('',(0.,1.,0.));
#21940=DIRECTION('',(0.,1.,0.));
#21941=DIRECTION('center_axis',(0.,1.,0.));
#21942=DIRECTION('ref_axis',(1.,0.,0.));
#21943=DIRECTION('center_axis',(0.,1.,0.));
#21944=DIRECTION('ref_axis',(1.,0.,0.));
#21945=DIRECTION('',(0.,-1.,0.));
#21946=DIRECTION('',(0.,1.,0.));
#21947=DIRECTION('center_axis',(-1.,0.,-1.22464679914735E-16));
#21948=DIRECTION('ref_axis',(-1.22464679914735E-16,0.,1.));
#21949=DIRECTION('',(-1.22464679914735E-16,0.,1.));
#21950=DIRECTION('',(0.,1.,0.));
#21951=DIRECTION('',(0.,1.,0.));
#21952=DIRECTION('center_axis',(0.,1.,0.));
#21953=DIRECTION('ref_axis',(1.,0.,0.));
#21954=DIRECTION('center_axis',(0.,1.,0.));
#21955=DIRECTION('ref_axis',(1.,0.,0.));
#21956=DIRECTION('',(0.,-1.,0.));
#21957=DIRECTION('',(0.,1.,0.));
#21958=DIRECTION('center_axis',(-0.951056516295154,0.,-0.309016994374948));
#21959=DIRECTION('ref_axis',(-0.309016994374948,0.,0.951056516295154));
#21960=DIRECTION('',(-0.309016994374948,0.,0.951056516295154));
#21961=DIRECTION('',(0.,1.,0.));
#21962=DIRECTION('',(0.,1.,0.));
#21963=DIRECTION('center_axis',(0.,1.,0.));
#21964=DIRECTION('ref_axis',(1.,0.,0.));
#21965=DIRECTION('center_axis',(0.,1.,0.));
#21966=DIRECTION('ref_axis',(1.,0.,0.));
#21967=DIRECTION('',(0.,-1.,0.));
#21968=DIRECTION('',(0.,1.,0.));
#21969=DIRECTION('center_axis',(-0.809016994374947,0.,-0.587785252292473));
#21970=DIRECTION('ref_axis',(-0.587785252292473,0.,0.809016994374947));
#21971=DIRECTION('',(-0.587785252292473,0.,0.809016994374947));
#21972=DIRECTION('',(0.,1.,0.));
#21973=DIRECTION('',(0.,1.,0.));
#21974=DIRECTION('center_axis',(0.,1.,0.));
#21975=DIRECTION('ref_axis',(1.,0.,0.));
#21976=DIRECTION('center_axis',(0.,1.,0.));
#21977=DIRECTION('ref_axis',(1.,0.,0.));
#21978=DIRECTION('',(0.,-1.,0.));
#21979=DIRECTION('',(0.,1.,0.));
#21980=DIRECTION('center_axis',(-0.587785252292473,0.,-0.809016994374948));
#21981=DIRECTION('ref_axis',(-0.809016994374948,0.,0.587785252292473));
#21982=DIRECTION('',(-0.809016994374948,0.,0.587785252292473));
#21983=DIRECTION('',(0.,1.,0.));
#21984=DIRECTION('',(0.,1.,0.));
#21985=DIRECTION('center_axis',(0.,1.,0.));
#21986=DIRECTION('ref_axis',(1.,0.,0.));
#21987=DIRECTION('center_axis',(0.,1.,0.));
#21988=DIRECTION('ref_axis',(1.,0.,0.));
#21989=DIRECTION('',(0.,-1.,0.));
#21990=DIRECTION('',(0.,1.,0.));
#21991=DIRECTION('center_axis',(-0.309016994374947,0.,-0.951056516295154));
#21992=DIRECTION('ref_axis',(-0.951056516295154,0.,0.309016994374947));
#21993=DIRECTION('',(-0.951056516295154,0.,0.309016994374947));
#21994=DIRECTION('',(0.,1.,0.));
#21995=DIRECTION('',(0.,1.,0.));
#21996=DIRECTION('center_axis',(0.,1.,0.));
#21997=DIRECTION('ref_axis',(1.,0.,0.));
#21998=DIRECTION('center_axis',(0.,1.,0.));
#21999=DIRECTION('ref_axis',(1.,0.,0.));
#22000=DIRECTION('',(0.,-1.,0.));
#22001=DIRECTION('',(0.,1.,0.));
#22002=DIRECTION('center_axis',(6.12323399573677E-17,0.,-1.));
#22003=DIRECTION('ref_axis',(-1.,0.,-6.12323399573677E-17));
#22004=DIRECTION('',(-1.,0.,-6.12323399573677E-17));
#22005=DIRECTION('',(0.,1.,0.));
#22006=DIRECTION('',(0.,1.,0.));
#22007=DIRECTION('center_axis',(0.,1.,0.));
#22008=DIRECTION('ref_axis',(1.,0.,0.));
#22009=DIRECTION('center_axis',(0.,1.,0.));
#22010=DIRECTION('ref_axis',(1.,0.,0.));
#22011=DIRECTION('',(0.,-1.,0.));
#22012=DIRECTION('',(0.,1.,0.));
#22013=DIRECTION('center_axis',(0.309016994374948,0.,-0.951056516295154));
#22014=DIRECTION('ref_axis',(-0.951056516295154,0.,-0.309016994374948));
#22015=DIRECTION('',(-0.951056516295154,0.,-0.309016994374948));
#22016=DIRECTION('',(0.,1.,0.));
#22017=DIRECTION('',(0.,1.,0.));
#22018=DIRECTION('center_axis',(0.,1.,0.));
#22019=DIRECTION('ref_axis',(1.,0.,0.));
#22020=DIRECTION('center_axis',(0.,1.,0.));
#22021=DIRECTION('ref_axis',(1.,0.,0.));
#22022=DIRECTION('',(0.,-1.,0.));
#22023=DIRECTION('',(0.,1.,0.));
#22024=DIRECTION('center_axis',(0.587785252292473,0.,-0.809016994374947));
#22025=DIRECTION('ref_axis',(-0.809016994374947,0.,-0.587785252292473));
#22026=DIRECTION('',(-0.809016994374947,0.,-0.587785252292473));
#22027=DIRECTION('',(0.,1.,0.));
#22028=DIRECTION('',(0.,1.,0.));
#22029=DIRECTION('center_axis',(0.,1.,0.));
#22030=DIRECTION('ref_axis',(1.,0.,0.));
#22031=DIRECTION('center_axis',(0.,1.,0.));
#22032=DIRECTION('ref_axis',(1.,0.,0.));
#22033=DIRECTION('',(0.,-1.,0.));
#22034=DIRECTION('',(0.,1.,0.));
#22035=DIRECTION('center_axis',(0.809016994374947,0.,-0.587785252292473));
#22036=DIRECTION('ref_axis',(-0.587785252292473,0.,-0.809016994374947));
#22037=DIRECTION('',(-0.587785252292473,0.,-0.809016994374947));
#22038=DIRECTION('',(0.,1.,0.));
#22039=DIRECTION('',(0.,1.,0.));
#22040=DIRECTION('center_axis',(0.,1.,0.));
#22041=DIRECTION('ref_axis',(1.,0.,0.));
#22042=DIRECTION('center_axis',(0.,1.,0.));
#22043=DIRECTION('ref_axis',(1.,0.,0.));
#22044=DIRECTION('',(0.,-1.,0.));
#22045=DIRECTION('',(0.,1.,0.));
#22046=DIRECTION('center_axis',(0.951056516295154,0.,-0.309016994374947));
#22047=DIRECTION('ref_axis',(-0.309016994374947,0.,-0.951056516295154));
#22048=DIRECTION('',(-0.309016994374947,0.,-0.951056516295154));
#22049=DIRECTION('',(0.,1.,0.));
#22050=DIRECTION('',(0.,1.,0.));
#22051=DIRECTION('center_axis',(0.,1.,0.));
#22052=DIRECTION('ref_axis',(1.,0.,0.));
#22053=DIRECTION('center_axis',(0.,1.,0.));
#22054=DIRECTION('ref_axis',(1.,0.,0.));
#22055=DIRECTION('',(0.,-1.,0.));
#22056=DIRECTION('',(0.,1.,0.));
#22057=DIRECTION('center_axis',(1.,0.,0.));
#22058=DIRECTION('ref_axis',(0.,0.,-1.));
#22059=DIRECTION('',(0.,0.,-1.));
#22060=DIRECTION('',(0.,1.,0.));
#22061=DIRECTION('',(0.,1.,0.));
#22062=DIRECTION('center_axis',(0.,1.,0.));
#22063=DIRECTION('ref_axis',(1.,0.,0.));
#22064=DIRECTION('center_axis',(0.,1.,0.));
#22065=DIRECTION('ref_axis',(1.,0.,0.));
#22066=DIRECTION('center_axis',(0.,1.,0.));
#22067=DIRECTION('ref_axis',(1.,0.,0.));
#22068=DIRECTION('axis',(0.,0.,1.));
#22069=DIRECTION('refdir',(1.,0.,0.));
#22070=DIRECTION('center_axis',(1.,0.,0.));
#22071=DIRECTION('ref_axis',(0.,0.,-1.));
#22072=DIRECTION('',(0.,0.707106781186547,-0.707106781186548));
#22073=DIRECTION('',(0.,1.,0.));
#22074=DIRECTION('',(0.,0.707106781186547,0.707106781186548));
#22075=DIRECTION('',(0.,0.,1.));
#22076=DIRECTION('',(0.,-0.707106781186548,0.707106781186548));
#22077=DIRECTION('',(0.,-1.,0.));
#22078=DIRECTION('',(0.,-0.707106781186548,-0.707106781186548));
#22079=DIRECTION('',(0.,0.,-1.));
#22080=DIRECTION('center_axis',(0.,-0.707106781186548,-0.707106781186548));
#22081=DIRECTION('ref_axis',(-1.,0.,0.));
#22082=DIRECTION('',(-1.,0.,0.));
#22083=DIRECTION('',(0.,0.707106781186548,-0.707106781186548));
#22084=DIRECTION('',(1.,0.,0.));
#22085=DIRECTION('center_axis',(0.,-1.,0.));
#22086=DIRECTION('ref_axis',(1.,0.,0.));
#22087=DIRECTION('',(1.,0.,0.));
#22088=DIRECTION('',(0.,0.,-1.));
#22089=DIRECTION('center_axis',(0.,-0.707106781186548,0.707106781186547));
#22090=DIRECTION('ref_axis',(1.,0.,0.));
#22091=DIRECTION('',(-1.,0.,0.));
#22092=DIRECTION('',(0.,-0.707106781186547,-0.707106781186548));
#22093=DIRECTION('center_axis',(0.,0.,1.));
#22094=DIRECTION('ref_axis',(1.,0.,0.));
#22095=DIRECTION('',(1.,0.,0.));
#22096=DIRECTION('',(0.,-1.,0.));
#22097=DIRECTION('center_axis',(1.,0.,0.));
#22098=DIRECTION('ref_axis',(0.,0.,-1.));
#22099=DIRECTION('',(0.,-0.707106781186547,0.707106781186548));
#22100=DIRECTION('',(0.,0.,1.));
#22101=DIRECTION('',(0.,0.707106781186548,0.707106781186548));
#22102=DIRECTION('',(0.,1.,0.));
#22103=DIRECTION('center_axis',(0.,0.707106781186548,0.707106781186547));
#22104=DIRECTION('ref_axis',(1.,0.,0.));
#22105=DIRECTION('',(-1.,0.,0.));
#22106=DIRECTION('center_axis',(0.,1.,0.));
#22107=DIRECTION('ref_axis',(-1.,0.,0.));
#22108=DIRECTION('',(1.,0.,0.));
#22109=DIRECTION('center_axis',(0.,0.707106781186548,-0.707106781186548));
#22110=DIRECTION('ref_axis',(-1.,0.,0.));
#22111=DIRECTION('',(-1.,0.,0.));
#22112=DIRECTION('center_axis',(0.,0.,1.));
#22113=DIRECTION('ref_axis',(1.,0.,0.));
#22114=DIRECTION('axis',(0.,0.,1.));
#22115=DIRECTION('refdir',(1.,0.,0.));
#22116=DIRECTION('axis',(0.,0.,1.));
#22117=DIRECTION('refdir',(1.,0.,0.));
#22118=DIRECTION('center_axis',(0.,1.,0.));
#22119=DIRECTION('ref_axis',(1.,0.,0.));
#22120=DIRECTION('center_axis',(0.,1.,0.));
#22121=DIRECTION('ref_axis',(1.,0.,0.));
#22122=DIRECTION('',(0.,1.,0.));
#22123=DIRECTION('center_axis',(0.,-1.,0.));
#22124=DIRECTION('ref_axis',(1.,0.,0.));
#22125=DIRECTION('center_axis',(0.,1.,0.));
#22126=DIRECTION('ref_axis',(1.,0.,0.));
#22127=DIRECTION('center_axis',(-1.,0.,0.));
#22128=DIRECTION('ref_axis',(0.,0.,1.));
#22129=DIRECTION('',(0.,-1.,0.));
#22130=DIRECTION('',(0.,0.,1.));
#22131=DIRECTION('',(0.,1.,0.));
#22132=DIRECTION('',(0.,0.,-1.));
#22133=DIRECTION('center_axis',(0.,1.,0.));
#22134=DIRECTION('ref_axis',(1.,0.,0.));
#22135=DIRECTION('center_axis',(0.,-1.,0.));
#22136=DIRECTION('ref_axis',(1.,0.,0.));
#22137=DIRECTION('',(-1.,0.,0.));
#22138=DIRECTION('',(0.,0.,1.));
#22139=DIRECTION('center_axis',(1.,0.,0.));
#22140=DIRECTION('ref_axis',(0.,0.,-1.));
#22141=DIRECTION('',(0.,1.,0.));
#22142=DIRECTION('',(0.,1.,0.));
#22143=DIRECTION('',(0.,0.,-1.));
#22144=DIRECTION('center_axis',(0.,0.,1.));
#22145=DIRECTION('ref_axis',(1.,0.,0.));
#22146=DIRECTION('',(1.,0.,0.));
#22147=DIRECTION('center_axis',(0.,1.,0.));
#22148=DIRECTION('ref_axis',(0.,0.,1.));
#22149=DIRECTION('center_axis',(0.,1.,0.));
#22150=DIRECTION('ref_axis',(1.,0.,0.));
#22151=DIRECTION('center_axis',(0.,1.,0.));
#22152=DIRECTION('ref_axis',(1.,0.,0.));
#22153=DIRECTION('center_axis',(0.,1.,0.));
#22154=DIRECTION('ref_axis',(1.,0.,0.));
#22155=DIRECTION('center_axis',(0.,1.,0.));
#22156=DIRECTION('ref_axis',(1.,0.,0.));
#22157=DIRECTION('center_axis',(0.,1.,0.));
#22158=DIRECTION('ref_axis',(1.,0.,0.));
#22159=DIRECTION('center_axis',(0.,1.,0.));
#22160=DIRECTION('ref_axis',(1.,0.,0.));
#22161=DIRECTION('center_axis',(0.,-1.,0.));
#22162=DIRECTION('ref_axis',(1.,0.,0.));
#22163=DIRECTION('center_axis',(0.,1.,0.));
#22164=DIRECTION('ref_axis',(1.,0.,0.));
#22165=DIRECTION('',(0.,-1.,0.));
#22166=DIRECTION('center_axis',(0.,1.,0.));
#22167=DIRECTION('ref_axis',(1.,0.,0.));
#22168=DIRECTION('',(0.,-1.,0.));
#22169=DIRECTION('center_axis',(0.,1.,0.));
#22170=DIRECTION('ref_axis',(1.,0.,0.));
#22171=DIRECTION('center_axis',(0.,1.,0.));
#22172=DIRECTION('ref_axis',(1.,0.,0.));
#22173=DIRECTION('center_axis',(0.,1.,0.));
#22174=DIRECTION('ref_axis',(1.,0.,0.));
#22175=DIRECTION('',(0.,-1.,0.));
#22176=DIRECTION('center_axis',(0.,1.,0.));
#22177=DIRECTION('ref_axis',(1.,0.,0.));
#22178=DIRECTION('center_axis',(0.,1.,0.));
#22179=DIRECTION('ref_axis',(1.,0.,0.));
#22180=DIRECTION('axis',(0.,0.,1.));
#22181=DIRECTION('refdir',(1.,0.,0.));
#22182=DIRECTION('center_axis',(0.,1.,0.));
#22183=DIRECTION('ref_axis',(1.,0.,0.));
#22184=DIRECTION('center_axis',(0.,-1.,0.));
#22185=DIRECTION('ref_axis',(1.,0.,0.));
#22186=DIRECTION('',(0.,-1.,0.));
#22187=DIRECTION('center_axis',(0.,-1.,0.));
#22188=DIRECTION('ref_axis',(1.,0.,0.));
#22189=DIRECTION('center_axis',(0.,1.,0.));
#22190=DIRECTION('ref_axis',(1.,0.,0.));
#22191=DIRECTION('center_axis',(0.,1.,0.));
#22192=DIRECTION('ref_axis',(1.,0.,0.));
#22193=DIRECTION('',(0.,-1.,0.));
#22194=DIRECTION('center_axis',(0.,1.,0.));
#22195=DIRECTION('ref_axis',(1.,0.,0.));
#22196=DIRECTION('center_axis',(0.,1.,0.));
#22197=DIRECTION('ref_axis',(1.,0.,0.));
#22198=DIRECTION('center_axis',(0.,1.,0.));
#22199=DIRECTION('ref_axis',(1.,0.,0.));
#22200=DIRECTION('axis',(0.,0.,1.));
#22201=DIRECTION('refdir',(1.,0.,0.));
#22202=DIRECTION('center_axis',(0.,1.,0.));
#22203=DIRECTION('ref_axis',(1.,0.,0.));
#22204=DIRECTION('center_axis',(0.,-1.,0.));
#22205=DIRECTION('ref_axis',(1.,0.,0.));
#22206=DIRECTION('',(0.,-1.,0.));
#22207=DIRECTION('center_axis',(0.,-1.,0.));
#22208=DIRECTION('ref_axis',(1.,0.,0.));
#22209=DIRECTION('center_axis',(0.,1.,0.));
#22210=DIRECTION('ref_axis',(1.,0.,0.));
#22211=DIRECTION('center_axis',(0.,1.,0.));
#22212=DIRECTION('ref_axis',(1.,0.,0.));
#22213=DIRECTION('',(0.,-1.,0.));
#22214=DIRECTION('center_axis',(0.,1.,0.));
#22215=DIRECTION('ref_axis',(1.,0.,0.));
#22216=DIRECTION('center_axis',(0.,1.,0.));
#22217=DIRECTION('ref_axis',(1.,0.,0.));
#22218=DIRECTION('center_axis',(0.,1.,0.));
#22219=DIRECTION('ref_axis',(1.,0.,0.));
#22220=DIRECTION('axis',(0.,0.,1.));
#22221=DIRECTION('refdir',(1.,0.,0.));
#22222=DIRECTION('center_axis',(0.,0.,1.));
#22223=DIRECTION('ref_axis',(1.,0.,0.));
#22224=DIRECTION('',(0.,1.,0.));
#22225=DIRECTION('center_axis',(0.,0.,1.));
#22226=DIRECTION('ref_axis',(1.,0.,0.));
#22227=DIRECTION('center_axis',(0.,0.,1.));
#22228=DIRECTION('ref_axis',(1.,0.,0.));
#22229=DIRECTION('center_axis',(0.,0.,1.));
#22230=DIRECTION('ref_axis',(1.,0.,0.));
#22231=DIRECTION('',(0.,0.,1.));
#22232=DIRECTION('center_axis',(0.,0.,1.));
#22233=DIRECTION('ref_axis',(1.,0.,0.));
#22234=DIRECTION('center_axis',(0.,0.,1.));
#22235=DIRECTION('ref_axis',(1.,0.,0.));
#22236=DIRECTION('',(0.,-1.,0.));
#22237=DIRECTION('center_axis',(0.,1.,0.));
#22238=DIRECTION('ref_axis',(1.,0.,0.));
#22239=DIRECTION('center_axis',(0.,-1.,0.));
#22240=DIRECTION('ref_axis',(1.,0.,0.));
#22241=DIRECTION('',(0.,-1.,0.));
#22242=DIRECTION('center_axis',(0.,-1.,0.));
#22243=DIRECTION('ref_axis',(1.,0.,0.));
#22244=DIRECTION('center_axis',(0.,1.,0.));
#22245=DIRECTION('ref_axis',(1.,0.,0.));
#22246=DIRECTION('center_axis',(0.,1.,0.));
#22247=DIRECTION('ref_axis',(1.,0.,0.));
#22248=DIRECTION('',(0.,-1.,0.));
#22249=DIRECTION('center_axis',(0.,1.,0.));
#22250=DIRECTION('ref_axis',(1.,0.,0.));
#22251=DIRECTION('center_axis',(0.,1.,0.));
#22252=DIRECTION('ref_axis',(1.,0.,0.));
#22253=DIRECTION('center_axis',(0.,1.,0.));
#22254=DIRECTION('ref_axis',(1.,0.,0.));
#22255=DIRECTION('axis',(0.,0.,1.));
#22256=DIRECTION('refdir',(1.,0.,0.));
#22257=DIRECTION('center_axis',(0.,1.,0.));
#22258=DIRECTION('ref_axis',(1.,0.,0.));
#22259=DIRECTION('center_axis',(0.,-1.,0.));
#22260=DIRECTION('ref_axis',(1.,0.,0.));
#22261=DIRECTION('',(0.,-1.,0.));
#22262=DIRECTION('center_axis',(0.,-1.,0.));
#22263=DIRECTION('ref_axis',(1.,0.,0.));
#22264=DIRECTION('center_axis',(0.,1.,0.));
#22265=DIRECTION('ref_axis',(1.,0.,0.));
#22266=DIRECTION('center_axis',(0.,1.,0.));
#22267=DIRECTION('ref_axis',(1.,0.,0.));
#22268=DIRECTION('',(0.,-1.,0.));
#22269=DIRECTION('center_axis',(0.,1.,0.));
#22270=DIRECTION('ref_axis',(1.,0.,0.));
#22271=DIRECTION('center_axis',(0.,1.,0.));
#22272=DIRECTION('ref_axis',(1.,0.,0.));
#22273=DIRECTION('center_axis',(0.,1.,0.));
#22274=DIRECTION('ref_axis',(1.,0.,0.));
#22275=DIRECTION('axis',(0.,0.,1.));
#22276=DIRECTION('refdir',(1.,0.,0.));
#22277=DIRECTION('center_axis',(0.,1.,0.));
#22278=DIRECTION('ref_axis',(1.,0.,0.));
#22279=DIRECTION('center_axis',(0.,-1.,0.));
#22280=DIRECTION('ref_axis',(1.,0.,0.));
#22281=DIRECTION('',(0.,-1.,0.));
#22282=DIRECTION('center_axis',(0.,-1.,0.));
#22283=DIRECTION('ref_axis',(1.,0.,0.));
#22284=DIRECTION('center_axis',(0.,1.,0.));
#22285=DIRECTION('ref_axis',(1.,0.,0.));
#22286=DIRECTION('center_axis',(0.,1.,0.));
#22287=DIRECTION('ref_axis',(1.,0.,0.));
#22288=DIRECTION('',(0.,-1.,0.));
#22289=DIRECTION('center_axis',(0.,1.,0.));
#22290=DIRECTION('ref_axis',(1.,0.,0.));
#22291=DIRECTION('center_axis',(0.,1.,0.));
#22292=DIRECTION('ref_axis',(1.,0.,0.));
#22293=DIRECTION('center_axis',(0.,1.,0.));
#22294=DIRECTION('ref_axis',(1.,0.,0.));
#22295=DIRECTION('axis',(0.,0.,1.));
#22296=DIRECTION('refdir',(1.,0.,0.));
#22297=DIRECTION('center_axis',(0.,0.,1.));
#22298=DIRECTION('ref_axis',(1.,0.,0.));
#22299=DIRECTION('',(0.,1.,0.));
#22300=DIRECTION('center_axis',(0.,0.,1.));
#22301=DIRECTION('ref_axis',(1.,0.,0.));
#22302=DIRECTION('center_axis',(0.,0.,1.));
#22303=DIRECTION('ref_axis',(1.,0.,0.));
#22304=DIRECTION('center_axis',(0.,0.,1.));
#22305=DIRECTION('ref_axis',(1.,0.,0.));
#22306=DIRECTION('',(0.,0.,1.));
#22307=DIRECTION('center_axis',(0.,0.,1.));
#22308=DIRECTION('ref_axis',(1.,0.,0.));
#22309=DIRECTION('center_axis',(0.,0.,1.));
#22310=DIRECTION('ref_axis',(1.,0.,0.));
#22311=DIRECTION('',(0.,-1.,0.));
#22312=DIRECTION('center_axis',(-0.045218998239459,0.,0.998977097934793));
#22313=DIRECTION('ref_axis',(0.998977097934793,0.,0.045218998239459));
#22314=DIRECTION('',(0.,1.,0.));
#22315=DIRECTION('',(0.998977097934793,0.,0.045218998239459));
#22316=DIRECTION('',(0.,1.,0.));
#22317=DIRECTION('',(0.998977097934793,0.,0.045218998239459));
#22318=DIRECTION('center_axis',(0.,1.,0.));
#22319=DIRECTION('ref_axis',(1.,0.,0.));
#22320=DIRECTION('center_axis',(0.,-1.,0.));
#22321=DIRECTION('ref_axis',(1.,0.,0.));
#22322=DIRECTION('',(-0.993771205694266,0.,-0.111439628198257));
#22323=DIRECTION('center_axis',(0.,1.,0.));
#22324=DIRECTION('ref_axis',(0.,0.,1.));
#22325=DIRECTION('center_axis',(0.,1.,0.));
#22326=DIRECTION('ref_axis',(1.,0.,0.));
#22327=DIRECTION('',(-0.993771205694266,0.,-0.111439628198257));
#22328=DIRECTION('center_axis',(0.111439628198257,0.,-0.993771205694266));
#22329=DIRECTION('ref_axis',(-0.993771205694266,0.,-0.111439628198257));
#22330=DIRECTION('',(0.,-1.,0.));
#22331=DIRECTION('center_axis',(0.,1.,0.));
#22332=DIRECTION('ref_axis',(1.,0.,0.));
#22333=DIRECTION('center_axis',(0.,-1.,0.));
#22334=DIRECTION('ref_axis',(1.,0.,0.));
#22335=DIRECTION('',(0.,-1.,0.));
#22336=DIRECTION('center_axis',(0.,-1.,0.));
#22337=DIRECTION('ref_axis',(1.,0.,0.));
#22338=DIRECTION('center_axis',(0.,1.,0.));
#22339=DIRECTION('ref_axis',(1.,0.,0.));
#22340=DIRECTION('center_axis',(0.,1.,0.));
#22341=DIRECTION('ref_axis',(1.,0.,0.));
#22342=DIRECTION('',(0.,-1.,0.));
#22343=DIRECTION('center_axis',(0.,1.,0.));
#22344=DIRECTION('ref_axis',(1.,0.,0.));
#22345=DIRECTION('center_axis',(0.,1.,0.));
#22346=DIRECTION('ref_axis',(1.,0.,0.));
#22347=DIRECTION('center_axis',(0.,1.,0.));
#22348=DIRECTION('ref_axis',(1.,0.,0.));
#22349=DIRECTION('axis',(0.,0.,1.));
#22350=DIRECTION('refdir',(1.,0.,0.));
#22351=DIRECTION('center_axis',(0.,1.,0.));
#22352=DIRECTION('ref_axis',(1.,0.,0.));
#22353=DIRECTION('center_axis',(0.,-1.,0.));
#22354=DIRECTION('ref_axis',(1.,0.,0.));
#22355=DIRECTION('',(0.,-1.,0.));
#22356=DIRECTION('center_axis',(0.,-1.,0.));
#22357=DIRECTION('ref_axis',(1.,0.,0.));
#22358=DIRECTION('center_axis',(0.,1.,0.));
#22359=DIRECTION('ref_axis',(1.,0.,0.));
#22360=DIRECTION('center_axis',(0.,1.,0.));
#22361=DIRECTION('ref_axis',(1.,0.,0.));
#22362=DIRECTION('',(0.,-1.,0.));
#22363=DIRECTION('center_axis',(0.,1.,0.));
#22364=DIRECTION('ref_axis',(1.,0.,0.));
#22365=DIRECTION('center_axis',(0.,1.,0.));
#22366=DIRECTION('ref_axis',(1.,0.,0.));
#22367=DIRECTION('center_axis',(0.,1.,0.));
#22368=DIRECTION('ref_axis',(1.,0.,0.));
#22369=DIRECTION('axis',(0.,0.,1.));
#22370=DIRECTION('refdir',(1.,0.,0.));
#22371=DIRECTION('center_axis',(1.,0.,0.));
#22372=DIRECTION('ref_axis',(0.,0.,-1.));
#22373=DIRECTION('',(0.,0.,1.));
#22374=DIRECTION('',(0.,1.,0.));
#22375=DIRECTION('',(0.,0.,-1.));
#22376=DIRECTION('',(0.,-1.,0.));
#22377=DIRECTION('center_axis',(0.,0.,-1.));
#22378=DIRECTION('ref_axis',(-1.,0.,0.));
#22379=DIRECTION('',(1.,0.,0.));
#22380=DIRECTION('',(0.,-1.,0.));
#22381=DIRECTION('',(-1.,0.,0.));
#22382=DIRECTION('center_axis',(-1.,0.,0.));
#22383=DIRECTION('ref_axis',(0.,0.,1.));
#22384=DIRECTION('',(0.,0.,-1.));
#22385=DIRECTION('',(0.,1.,0.));
#22386=DIRECTION('',(0.,0.,1.));
#22387=DIRECTION('center_axis',(0.,1.,0.));
#22388=DIRECTION('ref_axis',(1.,0.,0.));
#22389=DIRECTION('center_axis',(0.,-1.,0.));
#22390=DIRECTION('ref_axis',(1.,0.,0.));
#22391=DIRECTION('',(-0.309016994374948,0.,0.951056516295154));
#22392=DIRECTION('center_axis',(0.,-1.,0.));
#22393=DIRECTION('ref_axis',(1.,0.,0.));
#22394=DIRECTION('',(-0.453990499739547,0.,0.891006524188368));
#22395=DIRECTION('center_axis',(0.,-1.,0.));
#22396=DIRECTION('ref_axis',(1.,0.,0.));
#22397=DIRECTION('',(-0.587785252292473,0.,0.809016994374947));
#22398=DIRECTION('center_axis',(0.,-1.,0.));
#22399=DIRECTION('ref_axis',(1.,0.,0.));
#22400=DIRECTION('',(-0.707106781186548,0.,0.707106781186547));
#22401=DIRECTION('center_axis',(0.,-1.,0.));
#22402=DIRECTION('ref_axis',(1.,0.,0.));
#22403=DIRECTION('',(-0.809016994374948,0.,0.587785252292473));
#22404=DIRECTION('center_axis',(0.,-1.,0.));
#22405=DIRECTION('ref_axis',(1.,0.,0.));
#22406=DIRECTION('',(-0.891006524188368,0.,0.453990499739547));
#22407=DIRECTION('center_axis',(0.,-1.,0.));
#22408=DIRECTION('ref_axis',(1.,0.,0.));
#22409=DIRECTION('',(-0.951056516295154,0.,0.309016994374947));
#22410=DIRECTION('center_axis',(0.,-1.,0.));
#22411=DIRECTION('ref_axis',(1.,0.,0.));
#22412=DIRECTION('',(-0.987688340595138,0.,0.156434465040231));
#22413=DIRECTION('center_axis',(0.,-1.,0.));
#22414=DIRECTION('ref_axis',(1.,0.,0.));
#22415=DIRECTION('',(-1.,0.,-1.83697019872103E-16));
#22416=DIRECTION('center_axis',(0.,-1.,0.));
#22417=DIRECTION('ref_axis',(1.,0.,0.));
#22418=DIRECTION('',(-0.987688340595138,0.,-0.156434465040231));
#22419=DIRECTION('center_axis',(0.,-1.,0.));
#22420=DIRECTION('ref_axis',(1.,0.,0.));
#22421=DIRECTION('',(-0.951056516295154,0.,-0.309016994374948));
#22422=DIRECTION('center_axis',(0.,-1.,0.));
#22423=DIRECTION('ref_axis',(1.,0.,0.));
#22424=DIRECTION('',(-0.891006524188368,0.,-0.453990499739547));
#22425=DIRECTION('center_axis',(0.,-1.,0.));
#22426=DIRECTION('ref_axis',(1.,0.,0.));
#22427=DIRECTION('',(-0.809016994374947,0.,-0.587785252292473));
#22428=DIRECTION('center_axis',(0.,-1.,0.));
#22429=DIRECTION('ref_axis',(1.,0.,0.));
#22430=DIRECTION('',(-0.707106781186547,0.,-0.707106781186548));
#22431=DIRECTION('center_axis',(0.,-1.,0.));
#22432=DIRECTION('ref_axis',(1.,0.,0.));
#22433=DIRECTION('',(-0.587785252292473,0.,-0.809016994374948));
#22434=DIRECTION('center_axis',(0.,-1.,0.));
#22435=DIRECTION('ref_axis',(1.,0.,0.));
#22436=DIRECTION('',(-0.453990499739547,0.,-0.891006524188368));
#22437=DIRECTION('center_axis',(0.,-1.,0.));
#22438=DIRECTION('ref_axis',(1.,0.,0.));
#22439=DIRECTION('',(-0.309016994374947,0.,-0.951056516295154));
#22440=DIRECTION('center_axis',(0.,-1.,0.));
#22441=DIRECTION('ref_axis',(1.,0.,0.));
#22442=DIRECTION('',(-0.156434465040231,0.,-0.987688340595138));
#22443=DIRECTION('center_axis',(0.,-1.,0.));
#22444=DIRECTION('ref_axis',(1.,0.,0.));
#22445=DIRECTION('',(1.22464679914735E-16,0.,-1.));
#22446=DIRECTION('center_axis',(0.,-1.,0.));
#22447=DIRECTION('ref_axis',(1.,0.,0.));
#22448=DIRECTION('',(0.156434465040231,0.,-0.987688340595138));
#22449=DIRECTION('center_axis',(0.,-1.,0.));
#22450=DIRECTION('ref_axis',(1.,0.,0.));
#22451=DIRECTION('',(0.309016994374948,0.,-0.951056516295154));
#22452=DIRECTION('center_axis',(0.,-1.,0.));
#22453=DIRECTION('ref_axis',(1.,0.,0.));
#22454=DIRECTION('',(0.453990499739547,0.,-0.891006524188368));
#22455=DIRECTION('center_axis',(0.,-1.,0.));
#22456=DIRECTION('ref_axis',(1.,0.,0.));
#22457=DIRECTION('',(0.587785252292473,0.,-0.809016994374947));
#22458=DIRECTION('center_axis',(0.,-1.,0.));
#22459=DIRECTION('ref_axis',(1.,0.,0.));
#22460=DIRECTION('',(0.707106781186548,0.,-0.707106781186547));
#22461=DIRECTION('center_axis',(0.,-1.,0.));
#22462=DIRECTION('ref_axis',(1.,0.,0.));
#22463=DIRECTION('',(0.809016994374948,0.,-0.587785252292473));
#22464=DIRECTION('center_axis',(0.,-1.,0.));
#22465=DIRECTION('ref_axis',(1.,0.,0.));
#22466=DIRECTION('',(0.891006524188368,0.,-0.453990499739547));
#22467=DIRECTION('center_axis',(0.,-1.,0.));
#22468=DIRECTION('ref_axis',(1.,0.,0.));
#22469=DIRECTION('',(0.951056516295154,0.,-0.309016994374947));
#22470=DIRECTION('center_axis',(0.,-1.,0.));
#22471=DIRECTION('ref_axis',(1.,0.,0.));
#22472=DIRECTION('',(0.987688340595138,0.,-0.156434465040231));
#22473=DIRECTION('center_axis',(0.,-1.,0.));
#22474=DIRECTION('ref_axis',(1.,0.,0.));
#22475=DIRECTION('',(1.,0.,6.12323399573677E-17));
#22476=DIRECTION('center_axis',(0.,-1.,0.));
#22477=DIRECTION('ref_axis',(1.,0.,0.));
#22478=DIRECTION('',(0.987688340595138,0.,0.156434465040231));
#22479=DIRECTION('center_axis',(0.,-1.,0.));
#22480=DIRECTION('ref_axis',(1.,0.,0.));
#22481=DIRECTION('',(0.951056516295154,0.,0.309016994374948));
#22482=DIRECTION('center_axis',(0.,-1.,0.));
#22483=DIRECTION('ref_axis',(1.,0.,0.));
#22484=DIRECTION('',(0.891006524188368,0.,0.453990499739547));
#22485=DIRECTION('center_axis',(0.,-1.,0.));
#22486=DIRECTION('ref_axis',(1.,0.,0.));
#22487=DIRECTION('',(0.809016994374947,0.,0.587785252292473));
#22488=DIRECTION('center_axis',(0.,-1.,0.));
#22489=DIRECTION('ref_axis',(1.,0.,0.));
#22490=DIRECTION('',(0.707106781186547,0.,0.707106781186548));
#22491=DIRECTION('center_axis',(0.,-1.,0.));
#22492=DIRECTION('ref_axis',(1.,0.,0.));
#22493=DIRECTION('',(0.587785252292473,0.,0.809016994374947));
#22494=DIRECTION('center_axis',(0.,-1.,0.));
#22495=DIRECTION('ref_axis',(1.,0.,0.));
#22496=DIRECTION('',(0.453990499739547,0.,0.891006524188368));
#22497=DIRECTION('center_axis',(0.,-1.,0.));
#22498=DIRECTION('ref_axis',(1.,0.,0.));
#22499=DIRECTION('',(0.309016994374947,0.,0.951056516295154));
#22500=DIRECTION('center_axis',(0.,-1.,0.));
#22501=DIRECTION('ref_axis',(1.,0.,0.));
#22502=DIRECTION('',(0.156434465040231,0.,0.987688340595138));
#22503=DIRECTION('center_axis',(0.,-1.,0.));
#22504=DIRECTION('ref_axis',(1.,0.,0.));
#22505=DIRECTION('',(0.,0.,1.));
#22506=DIRECTION('center_axis',(0.,-1.,0.));
#22507=DIRECTION('ref_axis',(1.,0.,0.));
#22508=DIRECTION('',(-0.156434465040231,0.,0.987688340595138));
#22509=DIRECTION('center_axis',(0.,1.,0.));
#22510=DIRECTION('ref_axis',(1.,0.,0.));
#22511=DIRECTION('center_axis',(0.,1.,0.));
#22512=DIRECTION('ref_axis',(6.12323399573677E-17,0.,1.));
#22513=DIRECTION('center_axis',(0.,-1.,0.));
#22514=DIRECTION('ref_axis',(1.,0.,0.));
#22515=DIRECTION('center_axis',(0.,1.,0.));
#22516=DIRECTION('ref_axis',(1.,0.,0.));
#22517=DIRECTION('center_axis',(0.,1.,0.));
#22518=DIRECTION('ref_axis',(1.,0.,0.));
#22519=DIRECTION('',(0.,-1.,0.));
#22520=DIRECTION('center_axis',(0.,-1.,0.));
#22521=DIRECTION('ref_axis',(1.,0.,0.));
#22522=DIRECTION('center_axis',(0.,1.,0.));
#22523=DIRECTION('ref_axis',(1.,0.,0.));
#22524=DIRECTION('',(0.,1.,0.));
#22525=DIRECTION('',(0.,1.,0.));
#22526=DIRECTION('center_axis',(0.987688340595138,0.,0.156434465040231));
#22527=DIRECTION('ref_axis',(0.156434465040231,0.,-0.987688340595138));
#22528=DIRECTION('',(0.156434465040231,0.,-0.987688340595138));
#22529=DIRECTION('center_axis',(0.,1.,0.));
#22530=DIRECTION('ref_axis',(1.,0.,0.));
#22531=DIRECTION('center_axis',(0.,1.,0.));
#22532=DIRECTION('ref_axis',(1.,0.,0.));
#22533=DIRECTION('',(0.,1.,0.));
#22534=DIRECTION('',(0.,1.,0.));
#22535=DIRECTION('center_axis',(0.951056516295154,0.,0.309016994374948));
#22536=DIRECTION('ref_axis',(0.309016994374948,0.,-0.951056516295154));
#22537=DIRECTION('',(0.309016994374948,0.,-0.951056516295154));
#22538=DIRECTION('center_axis',(0.,1.,0.));
#22539=DIRECTION('ref_axis',(1.,0.,0.));
#22540=DIRECTION('center_axis',(0.,1.,0.));
#22541=DIRECTION('ref_axis',(1.,0.,0.));
#22542=DIRECTION('',(0.,1.,0.));
#22543=DIRECTION('',(0.,1.,0.));
#22544=DIRECTION('center_axis',(0.891006524188368,0.,0.453990499739547));
#22545=DIRECTION('ref_axis',(0.453990499739547,0.,-0.891006524188368));
#22546=DIRECTION('',(0.453990499739547,0.,-0.891006524188368));
#22547=DIRECTION('center_axis',(0.,1.,0.));
#22548=DIRECTION('ref_axis',(1.,0.,0.));
#22549=DIRECTION('center_axis',(0.,1.,0.));
#22550=DIRECTION('ref_axis',(1.,0.,0.));
#22551=DIRECTION('',(0.,1.,0.));
#22552=DIRECTION('',(0.,1.,0.));
#22553=DIRECTION('center_axis',(0.809016994374947,0.,0.587785252292473));
#22554=DIRECTION('ref_axis',(0.587785252292473,0.,-0.809016994374947));
#22555=DIRECTION('',(0.587785252292473,0.,-0.809016994374947));
#22556=DIRECTION('center_axis',(0.,1.,0.));
#22557=DIRECTION('ref_axis',(1.,0.,0.));
#22558=DIRECTION('center_axis',(0.,1.,0.));
#22559=DIRECTION('ref_axis',(1.,0.,0.));
#22560=DIRECTION('',(0.,1.,0.));
#22561=DIRECTION('',(0.,1.,0.));
#22562=DIRECTION('center_axis',(0.707106781186547,0.,0.707106781186548));
#22563=DIRECTION('ref_axis',(0.707106781186548,0.,-0.707106781186547));
#22564=DIRECTION('',(0.707106781186548,0.,-0.707106781186547));
#22565=DIRECTION('center_axis',(0.,1.,0.));
#22566=DIRECTION('ref_axis',(1.,0.,0.));
#22567=DIRECTION('center_axis',(0.,1.,0.));
#22568=DIRECTION('ref_axis',(1.,0.,0.));
#22569=DIRECTION('',(0.,1.,0.));
#22570=DIRECTION('',(0.,1.,0.));
#22571=DIRECTION('center_axis',(0.587785252292473,0.,0.809016994374948));
#22572=DIRECTION('ref_axis',(0.809016994374948,0.,-0.587785252292473));
#22573=DIRECTION('',(0.809016994374948,0.,-0.587785252292473));
#22574=DIRECTION('center_axis',(0.,1.,0.));
#22575=DIRECTION('ref_axis',(1.,0.,0.));
#22576=DIRECTION('center_axis',(0.,1.,0.));
#22577=DIRECTION('ref_axis',(1.,0.,0.));
#22578=DIRECTION('',(0.,1.,0.));
#22579=DIRECTION('',(0.,1.,0.));
#22580=DIRECTION('center_axis',(0.453990499739547,0.,0.891006524188368));
#22581=DIRECTION('ref_axis',(0.891006524188368,0.,-0.453990499739547));
#22582=DIRECTION('',(0.891006524188368,0.,-0.453990499739547));
#22583=DIRECTION('center_axis',(0.,1.,0.));
#22584=DIRECTION('ref_axis',(1.,0.,0.));
#22585=DIRECTION('center_axis',(0.,1.,0.));
#22586=DIRECTION('ref_axis',(1.,0.,0.));
#22587=DIRECTION('',(0.,1.,0.));
#22588=DIRECTION('',(0.,1.,0.));
#22589=DIRECTION('center_axis',(0.309016994374947,0.,0.951056516295154));
#22590=DIRECTION('ref_axis',(0.951056516295154,0.,-0.309016994374947));
#22591=DIRECTION('',(0.951056516295154,0.,-0.309016994374947));
#22592=DIRECTION('center_axis',(0.,1.,0.));
#22593=DIRECTION('ref_axis',(1.,0.,0.));
#22594=DIRECTION('center_axis',(0.,1.,0.));
#22595=DIRECTION('ref_axis',(1.,0.,0.));
#22596=DIRECTION('',(0.,1.,0.));
#22597=DIRECTION('',(0.,1.,0.));
#22598=DIRECTION('center_axis',(0.156434465040231,0.,0.987688340595138));
#22599=DIRECTION('ref_axis',(0.987688340595138,0.,-0.156434465040231));
#22600=DIRECTION('',(0.987688340595138,0.,-0.156434465040231));
#22601=DIRECTION('center_axis',(0.,1.,0.));
#22602=DIRECTION('ref_axis',(1.,0.,0.));
#22603=DIRECTION('center_axis',(0.,1.,0.));
#22604=DIRECTION('ref_axis',(1.,0.,0.));
#22605=DIRECTION('',(0.,1.,0.));
#22606=DIRECTION('',(0.,1.,0.));
#22607=DIRECTION('center_axis',(-1.83697019872103E-16,0.,1.));
#22608=DIRECTION('ref_axis',(1.,0.,1.83697019872103E-16));
#22609=DIRECTION('',(1.,0.,1.83697019872103E-16));
#22610=DIRECTION('center_axis',(0.,1.,0.));
#22611=DIRECTION('ref_axis',(1.,0.,0.));
#22612=DIRECTION('center_axis',(0.,1.,0.));
#22613=DIRECTION('ref_axis',(1.,0.,0.));
#22614=DIRECTION('',(0.,1.,0.));
#22615=DIRECTION('',(0.,1.,0.));
#22616=DIRECTION('center_axis',(-0.156434465040231,0.,0.987688340595138));
#22617=DIRECTION('ref_axis',(0.987688340595138,0.,0.156434465040231));
#22618=DIRECTION('',(0.987688340595138,0.,0.156434465040231));
#22619=DIRECTION('center_axis',(0.,1.,0.));
#22620=DIRECTION('ref_axis',(1.,0.,0.));
#22621=DIRECTION('center_axis',(0.,1.,0.));
#22622=DIRECTION('ref_axis',(1.,0.,0.));
#22623=DIRECTION('',(0.,1.,0.));
#22624=DIRECTION('',(0.,1.,0.));
#22625=DIRECTION('center_axis',(-0.309016994374948,0.,0.951056516295154));
#22626=DIRECTION('ref_axis',(0.951056516295154,0.,0.309016994374948));
#22627=DIRECTION('',(0.951056516295154,0.,0.309016994374948));
#22628=DIRECTION('center_axis',(0.,1.,0.));
#22629=DIRECTION('ref_axis',(1.,0.,0.));
#22630=DIRECTION('center_axis',(0.,1.,0.));
#22631=DIRECTION('ref_axis',(1.,0.,0.));
#22632=DIRECTION('',(0.,1.,0.));
#22633=DIRECTION('',(0.,1.,0.));
#22634=DIRECTION('center_axis',(-0.453990499739547,0.,0.891006524188368));
#22635=DIRECTION('ref_axis',(0.891006524188368,0.,0.453990499739547));
#22636=DIRECTION('',(0.891006524188368,0.,0.453990499739547));
#22637=DIRECTION('center_axis',(0.,1.,0.));
#22638=DIRECTION('ref_axis',(1.,0.,0.));
#22639=DIRECTION('center_axis',(0.,1.,0.));
#22640=DIRECTION('ref_axis',(1.,0.,0.));
#22641=DIRECTION('',(0.,1.,0.));
#22642=DIRECTION('',(0.,1.,0.));
#22643=DIRECTION('center_axis',(-0.587785252292473,0.,0.809016994374947));
#22644=DIRECTION('ref_axis',(0.809016994374947,0.,0.587785252292473));
#22645=DIRECTION('',(0.809016994374947,0.,0.587785252292473));
#22646=DIRECTION('center_axis',(0.,1.,0.));
#22647=DIRECTION('ref_axis',(1.,0.,0.));
#22648=DIRECTION('center_axis',(0.,1.,0.));
#22649=DIRECTION('ref_axis',(1.,0.,0.));
#22650=DIRECTION('',(0.,1.,0.));
#22651=DIRECTION('',(0.,1.,0.));
#22652=DIRECTION('center_axis',(-0.707106781186548,0.,0.707106781186547));
#22653=DIRECTION('ref_axis',(0.707106781186547,0.,0.707106781186548));
#22654=DIRECTION('',(0.707106781186547,0.,0.707106781186548));
#22655=DIRECTION('center_axis',(0.,1.,0.));
#22656=DIRECTION('ref_axis',(1.,0.,0.));
#22657=DIRECTION('center_axis',(0.,1.,0.));
#22658=DIRECTION('ref_axis',(1.,0.,0.));
#22659=DIRECTION('',(0.,1.,0.));
#22660=DIRECTION('',(0.,1.,0.));
#22661=DIRECTION('center_axis',(-0.809016994374948,0.,0.587785252292473));
#22662=DIRECTION('ref_axis',(0.587785252292473,0.,0.809016994374948));
#22663=DIRECTION('',(0.587785252292473,0.,0.809016994374948));
#22664=DIRECTION('center_axis',(0.,1.,0.));
#22665=DIRECTION('ref_axis',(1.,0.,0.));
#22666=DIRECTION('center_axis',(0.,1.,0.));
#22667=DIRECTION('ref_axis',(1.,0.,0.));
#22668=DIRECTION('',(0.,1.,0.));
#22669=DIRECTION('',(0.,1.,0.));
#22670=DIRECTION('center_axis',(-0.891006524188368,0.,0.453990499739547));
#22671=DIRECTION('ref_axis',(0.453990499739547,0.,0.891006524188368));
#22672=DIRECTION('',(0.453990499739547,0.,0.891006524188368));
#22673=DIRECTION('center_axis',(0.,1.,0.));
#22674=DIRECTION('ref_axis',(1.,0.,0.));
#22675=DIRECTION('center_axis',(0.,1.,0.));
#22676=DIRECTION('ref_axis',(1.,0.,0.));
#22677=DIRECTION('',(0.,1.,0.));
#22678=DIRECTION('',(0.,1.,0.));
#22679=DIRECTION('center_axis',(-0.951056516295154,0.,0.309016994374947));
#22680=DIRECTION('ref_axis',(0.309016994374947,0.,0.951056516295154));
#22681=DIRECTION('',(0.309016994374947,0.,0.951056516295154));
#22682=DIRECTION('center_axis',(0.,1.,0.));
#22683=DIRECTION('ref_axis',(1.,0.,0.));
#22684=DIRECTION('center_axis',(0.,1.,0.));
#22685=DIRECTION('ref_axis',(1.,0.,0.));
#22686=DIRECTION('',(0.,1.,0.));
#22687=DIRECTION('',(0.,1.,0.));
#22688=DIRECTION('center_axis',(-0.987688340595138,0.,0.156434465040231));
#22689=DIRECTION('ref_axis',(0.156434465040231,0.,0.987688340595138));
#22690=DIRECTION('',(0.156434465040231,0.,0.987688340595138));
#22691=DIRECTION('center_axis',(0.,1.,0.));
#22692=DIRECTION('ref_axis',(1.,0.,0.));
#22693=DIRECTION('center_axis',(0.,1.,0.));
#22694=DIRECTION('ref_axis',(1.,0.,0.));
#22695=DIRECTION('',(0.,1.,0.));
#22696=DIRECTION('',(0.,1.,0.));
#22697=DIRECTION('center_axis',(-1.,0.,-1.22464679914735E-16));
#22698=DIRECTION('ref_axis',(-1.22464679914735E-16,0.,1.));
#22699=DIRECTION('',(-1.22464679914735E-16,0.,1.));
#22700=DIRECTION('center_axis',(0.,1.,0.));
#22701=DIRECTION('ref_axis',(1.,0.,0.));
#22702=DIRECTION('center_axis',(0.,1.,0.));
#22703=DIRECTION('ref_axis',(1.,0.,0.));
#22704=DIRECTION('',(0.,1.,0.));
#22705=DIRECTION('',(0.,1.,0.));
#22706=DIRECTION('center_axis',(-0.987688340595138,0.,-0.156434465040231));
#22707=DIRECTION('ref_axis',(-0.156434465040231,0.,0.987688340595138));
#22708=DIRECTION('',(-0.156434465040231,0.,0.987688340595138));
#22709=DIRECTION('center_axis',(0.,1.,0.));
#22710=DIRECTION('ref_axis',(1.,0.,0.));
#22711=DIRECTION('center_axis',(0.,1.,0.));
#22712=DIRECTION('ref_axis',(1.,0.,0.));
#22713=DIRECTION('',(0.,1.,0.));
#22714=DIRECTION('',(0.,1.,0.));
#22715=DIRECTION('center_axis',(-0.951056516295154,0.,-0.309016994374948));
#22716=DIRECTION('ref_axis',(-0.309016994374948,0.,0.951056516295154));
#22717=DIRECTION('',(-0.309016994374948,0.,0.951056516295154));
#22718=DIRECTION('center_axis',(0.,1.,0.));
#22719=DIRECTION('ref_axis',(1.,0.,0.));
#22720=DIRECTION('center_axis',(0.,1.,0.));
#22721=DIRECTION('ref_axis',(1.,0.,0.));
#22722=DIRECTION('',(0.,1.,0.));
#22723=DIRECTION('',(0.,1.,0.));
#22724=DIRECTION('center_axis',(-0.891006524188368,0.,-0.453990499739547));
#22725=DIRECTION('ref_axis',(-0.453990499739547,0.,0.891006524188368));
#22726=DIRECTION('',(-0.453990499739547,0.,0.891006524188368));
#22727=DIRECTION('center_axis',(0.,1.,0.));
#22728=DIRECTION('ref_axis',(1.,0.,0.));
#22729=DIRECTION('center_axis',(0.,1.,0.));
#22730=DIRECTION('ref_axis',(1.,0.,0.));
#22731=DIRECTION('',(0.,1.,0.));
#22732=DIRECTION('',(0.,1.,0.));
#22733=DIRECTION('center_axis',(-0.809016994374947,0.,-0.587785252292473));
#22734=DIRECTION('ref_axis',(-0.587785252292473,0.,0.809016994374947));
#22735=DIRECTION('',(-0.587785252292473,0.,0.809016994374947));
#22736=DIRECTION('center_axis',(0.,1.,0.));
#22737=DIRECTION('ref_axis',(1.,0.,0.));
#22738=DIRECTION('center_axis',(0.,1.,0.));
#22739=DIRECTION('ref_axis',(1.,0.,0.));
#22740=DIRECTION('',(0.,1.,0.));
#22741=DIRECTION('',(0.,1.,0.));
#22742=DIRECTION('center_axis',(-0.707106781186547,0.,-0.707106781186548));
#22743=DIRECTION('ref_axis',(-0.707106781186548,0.,0.707106781186547));
#22744=DIRECTION('',(-0.707106781186548,0.,0.707106781186547));
#22745=DIRECTION('center_axis',(0.,1.,0.));
#22746=DIRECTION('ref_axis',(1.,0.,0.));
#22747=DIRECTION('center_axis',(0.,1.,0.));
#22748=DIRECTION('ref_axis',(1.,0.,0.));
#22749=DIRECTION('',(0.,1.,0.));
#22750=DIRECTION('',(0.,1.,0.));
#22751=DIRECTION('center_axis',(-0.587785252292473,0.,-0.809016994374948));
#22752=DIRECTION('ref_axis',(-0.809016994374948,0.,0.587785252292473));
#22753=DIRECTION('',(-0.809016994374948,0.,0.587785252292473));
#22754=DIRECTION('center_axis',(0.,1.,0.));
#22755=DIRECTION('ref_axis',(1.,0.,0.));
#22756=DIRECTION('center_axis',(0.,1.,0.));
#22757=DIRECTION('ref_axis',(1.,0.,0.));
#22758=DIRECTION('',(0.,1.,0.));
#22759=DIRECTION('',(0.,1.,0.));
#22760=DIRECTION('center_axis',(-0.453990499739547,0.,-0.891006524188368));
#22761=DIRECTION('ref_axis',(-0.891006524188368,0.,0.453990499739547));
#22762=DIRECTION('',(-0.891006524188368,0.,0.453990499739547));
#22763=DIRECTION('center_axis',(0.,1.,0.));
#22764=DIRECTION('ref_axis',(1.,0.,0.));
#22765=DIRECTION('center_axis',(0.,1.,0.));
#22766=DIRECTION('ref_axis',(1.,0.,0.));
#22767=DIRECTION('',(0.,1.,0.));
#22768=DIRECTION('',(0.,1.,0.));
#22769=DIRECTION('center_axis',(-0.309016994374947,0.,-0.951056516295154));
#22770=DIRECTION('ref_axis',(-0.951056516295154,0.,0.309016994374947));
#22771=DIRECTION('',(-0.951056516295154,0.,0.309016994374947));
#22772=DIRECTION('center_axis',(0.,1.,0.));
#22773=DIRECTION('ref_axis',(1.,0.,0.));
#22774=DIRECTION('center_axis',(0.,1.,0.));
#22775=DIRECTION('ref_axis',(1.,0.,0.));
#22776=DIRECTION('',(0.,1.,0.));
#22777=DIRECTION('',(0.,1.,0.));
#22778=DIRECTION('center_axis',(-0.156434465040231,0.,-0.987688340595138));
#22779=DIRECTION('ref_axis',(-0.987688340595138,0.,0.156434465040231));
#22780=DIRECTION('',(-0.987688340595138,0.,0.156434465040231));
#22781=DIRECTION('center_axis',(0.,1.,0.));
#22782=DIRECTION('ref_axis',(1.,0.,0.));
#22783=DIRECTION('center_axis',(0.,1.,0.));
#22784=DIRECTION('ref_axis',(1.,0.,0.));
#22785=DIRECTION('',(0.,1.,0.));
#22786=DIRECTION('',(0.,1.,0.));
#22787=DIRECTION('center_axis',(6.12323399573677E-17,0.,-1.));
#22788=DIRECTION('ref_axis',(-1.,0.,-6.12323399573677E-17));
#22789=DIRECTION('',(-1.,0.,-6.12323399573677E-17));
#22790=DIRECTION('center_axis',(0.,1.,0.));
#22791=DIRECTION('ref_axis',(1.,0.,0.));
#22792=DIRECTION('center_axis',(0.,1.,0.));
#22793=DIRECTION('ref_axis',(1.,0.,0.));
#22794=DIRECTION('',(0.,1.,0.));
#22795=DIRECTION('',(0.,1.,0.));
#22796=DIRECTION('center_axis',(0.156434465040231,0.,-0.987688340595138));
#22797=DIRECTION('ref_axis',(-0.987688340595138,0.,-0.156434465040231));
#22798=DIRECTION('',(-0.987688340595138,0.,-0.156434465040231));
#22799=DIRECTION('center_axis',(0.,1.,0.));
#22800=DIRECTION('ref_axis',(1.,0.,0.));
#22801=DIRECTION('center_axis',(0.,1.,0.));
#22802=DIRECTION('ref_axis',(1.,0.,0.));
#22803=DIRECTION('',(0.,1.,0.));
#22804=DIRECTION('',(0.,1.,0.));
#22805=DIRECTION('center_axis',(0.309016994374948,0.,-0.951056516295154));
#22806=DIRECTION('ref_axis',(-0.951056516295154,0.,-0.309016994374948));
#22807=DIRECTION('',(-0.951056516295154,0.,-0.309016994374948));
#22808=DIRECTION('center_axis',(0.,1.,0.));
#22809=DIRECTION('ref_axis',(1.,0.,0.));
#22810=DIRECTION('center_axis',(0.,1.,0.));
#22811=DIRECTION('ref_axis',(1.,0.,0.));
#22812=DIRECTION('',(0.,1.,0.));
#22813=DIRECTION('',(0.,1.,0.));
#22814=DIRECTION('center_axis',(0.453990499739547,0.,-0.891006524188368));
#22815=DIRECTION('ref_axis',(-0.891006524188368,0.,-0.453990499739547));
#22816=DIRECTION('',(-0.891006524188368,0.,-0.453990499739547));
#22817=DIRECTION('center_axis',(0.,1.,0.));
#22818=DIRECTION('ref_axis',(1.,0.,0.));
#22819=DIRECTION('center_axis',(0.,1.,0.));
#22820=DIRECTION('ref_axis',(1.,0.,0.));
#22821=DIRECTION('',(0.,1.,0.));
#22822=DIRECTION('',(0.,1.,0.));
#22823=DIRECTION('center_axis',(0.587785252292473,0.,-0.809016994374947));
#22824=DIRECTION('ref_axis',(-0.809016994374947,0.,-0.587785252292473));
#22825=DIRECTION('',(-0.809016994374947,0.,-0.587785252292473));
#22826=DIRECTION('center_axis',(0.,1.,0.));
#22827=DIRECTION('ref_axis',(1.,0.,0.));
#22828=DIRECTION('center_axis',(0.,1.,0.));
#22829=DIRECTION('ref_axis',(1.,0.,0.));
#22830=DIRECTION('',(0.,1.,0.));
#22831=DIRECTION('',(0.,1.,0.));
#22832=DIRECTION('center_axis',(0.707106781186548,0.,-0.707106781186547));
#22833=DIRECTION('ref_axis',(-0.707106781186547,0.,-0.707106781186548));
#22834=DIRECTION('',(-0.707106781186547,0.,-0.707106781186548));
#22835=DIRECTION('center_axis',(0.,1.,0.));
#22836=DIRECTION('ref_axis',(1.,0.,0.));
#22837=DIRECTION('center_axis',(0.,1.,0.));
#22838=DIRECTION('ref_axis',(1.,0.,0.));
#22839=DIRECTION('',(0.,1.,0.));
#22840=DIRECTION('',(0.,1.,0.));
#22841=DIRECTION('center_axis',(0.809016994374947,0.,-0.587785252292473));
#22842=DIRECTION('ref_axis',(-0.587785252292473,0.,-0.809016994374947));
#22843=DIRECTION('',(-0.587785252292473,0.,-0.809016994374947));
#22844=DIRECTION('center_axis',(0.,1.,0.));
#22845=DIRECTION('ref_axis',(1.,0.,0.));
#22846=DIRECTION('center_axis',(0.,1.,0.));
#22847=DIRECTION('ref_axis',(1.,0.,0.));
#22848=DIRECTION('',(0.,1.,0.));
#22849=DIRECTION('',(0.,1.,0.));
#22850=DIRECTION('center_axis',(0.891006524188368,0.,-0.453990499739547));
#22851=DIRECTION('ref_axis',(-0.453990499739547,0.,-0.891006524188368));
#22852=DIRECTION('',(-0.453990499739547,0.,-0.891006524188368));
#22853=DIRECTION('center_axis',(0.,1.,0.));
#22854=DIRECTION('ref_axis',(1.,0.,0.));
#22855=DIRECTION('center_axis',(0.,1.,0.));
#22856=DIRECTION('ref_axis',(1.,0.,0.));
#22857=DIRECTION('',(0.,1.,0.));
#22858=DIRECTION('',(0.,1.,0.));
#22859=DIRECTION('center_axis',(0.951056516295154,0.,-0.309016994374947));
#22860=DIRECTION('ref_axis',(-0.309016994374947,0.,-0.951056516295154));
#22861=DIRECTION('',(-0.309016994374947,0.,-0.951056516295154));
#22862=DIRECTION('center_axis',(0.,1.,0.));
#22863=DIRECTION('ref_axis',(1.,0.,0.));
#22864=DIRECTION('center_axis',(0.,1.,0.));
#22865=DIRECTION('ref_axis',(1.,0.,0.));
#22866=DIRECTION('',(0.,1.,0.));
#22867=DIRECTION('center_axis',(0.987688340595138,0.,-0.156434465040231));
#22868=DIRECTION('ref_axis',(-0.156434465040231,0.,-0.987688340595138));
#22869=DIRECTION('',(-0.156434465040231,0.,-0.987688340595138));
#22870=DIRECTION('',(0.,1.,0.));
#22871=DIRECTION('center_axis',(0.,1.,0.));
#22872=DIRECTION('ref_axis',(1.,0.,0.));
#22873=DIRECTION('center_axis',(0.,1.,0.));
#22874=DIRECTION('ref_axis',(1.,0.,0.));
#22875=DIRECTION('',(0.,1.,0.));
#22876=DIRECTION('',(0.,1.,0.));
#22877=DIRECTION('center_axis',(1.,0.,0.));
#22878=DIRECTION('ref_axis',(0.,0.,-1.));
#22879=DIRECTION('',(0.,0.,-1.));
#22880=DIRECTION('center_axis',(0.,1.,0.));
#22881=DIRECTION('ref_axis',(1.,0.,0.));
#22882=DIRECTION('center_axis',(0.,1.,0.));
#22883=DIRECTION('ref_axis',(1.,0.,0.));
#22884=DIRECTION('center_axis',(0.,1.,0.));
#22885=DIRECTION('ref_axis',(1.,0.,0.));
#22886=DIRECTION('axis',(0.,0.,1.));
#22887=DIRECTION('refdir',(1.,0.,0.));
#22888=DIRECTION('center_axis',(1.,0.,0.));
#22889=DIRECTION('ref_axis',(0.,0.,-1.));
#22890=DIRECTION('',(0.,-0.707106781186547,-0.707106781186548));
#22891=DIRECTION('',(0.,-1.,0.));
#22892=DIRECTION('',(0.,-0.707106781186547,0.707106781186548));
#22893=DIRECTION('',(0.,0.,1.));
#22894=DIRECTION('',(0.,0.707106781186547,0.707106781186548));
#22895=DIRECTION('',(0.,1.,0.));
#22896=DIRECTION('',(0.,0.707106781186547,-0.707106781186548));
#22897=DIRECTION('',(0.,0.,-1.));
#22898=DIRECTION('center_axis',(0.,0.707106781186548,-0.707106781186547));
#22899=DIRECTION('ref_axis',(-1.,0.,0.));
#22900=DIRECTION('',(1.,0.,0.));
#22901=DIRECTION('',(0.,-0.707106781186547,-0.707106781186548));
#22902=DIRECTION('',(-1.,0.,0.));
#22903=DIRECTION('center_axis',(0.,1.,0.));
#22904=DIRECTION('ref_axis',(-1.,0.,0.));
#22905=DIRECTION('',(-1.,0.,0.));
#22906=DIRECTION('',(0.,0.,-1.));
#22907=DIRECTION('center_axis',(0.,0.707106781186548,0.707106781186547));
#22908=DIRECTION('ref_axis',(1.,0.,0.));
#22909=DIRECTION('',(1.,0.,0.));
#22910=DIRECTION('',(0.,0.707106781186547,-0.707106781186548));
#22911=DIRECTION('center_axis',(0.,0.,1.));
#22912=DIRECTION('ref_axis',(1.,0.,0.));
#22913=DIRECTION('',(-1.,0.,0.));
#22914=DIRECTION('',(0.,1.,0.));
#22915=DIRECTION('center_axis',(1.,0.,0.));
#22916=DIRECTION('ref_axis',(0.,0.,-1.));
#22917=DIRECTION('',(0.,-0.707106781186547,0.707106781186548));
#22918=DIRECTION('',(0.,-1.,0.));
#22919=DIRECTION('',(0.,0.707106781186547,0.707106781186548));
#22920=DIRECTION('',(0.,0.,1.));
#22921=DIRECTION('center_axis',(0.,0.,1.));
#22922=DIRECTION('ref_axis',(1.,0.,0.));
#22923=DIRECTION('',(1.,0.,0.));
#22924=DIRECTION('center_axis',(0.,-0.707106781186548,0.707106781186547));
#22925=DIRECTION('ref_axis',(1.,0.,0.));
#22926=DIRECTION('',(1.,0.,0.));
#22927=DIRECTION('center_axis',(0.,-0.707106781186548,-0.707106781186547));
#22928=DIRECTION('ref_axis',(-1.,0.,0.));
#22929=DIRECTION('',(-1.,0.,0.));
#22930=DIRECTION('center_axis',(0.,-1.,0.));
#22931=DIRECTION('ref_axis',(1.,0.,0.));
#22932=DIRECTION('axis',(0.,0.,1.));
#22933=DIRECTION('refdir',(1.,0.,0.));
#22934=DIRECTION('center_axis',(0.866025403784439,0.,-0.5));
#22935=DIRECTION('ref_axis',(0.5,0.,0.866025403784439));
#22936=DIRECTION('',(0.5,0.,0.866025403784439));
#22937=DIRECTION('',(0.,-1.,0.));
#22938=DIRECTION('',(0.5,0.,0.866025403784439));
#22939=DIRECTION('',(0.,-1.,0.));
#22940=DIRECTION('center_axis',(1.92296268638356E-16,0.,-1.));
#22941=DIRECTION('ref_axis',(1.,0.,1.92296268638356E-16));
#22942=DIRECTION('',(1.,0.,1.92296268638356E-16));
#22943=DIRECTION('',(0.,-1.,0.));
#22944=DIRECTION('',(1.,0.,1.92296268638356E-16));
#22945=DIRECTION('center_axis',(-0.866025403784439,0.,-0.5));
#22946=DIRECTION('ref_axis',(0.5,0.,-0.866025403784439));
#22947=DIRECTION('',(0.5,0.,-0.866025403784439));
#22948=DIRECTION('',(0.,-1.,0.));
#22949=DIRECTION('',(0.5,0.,-0.866025403784438));
#22950=DIRECTION('center_axis',(-0.866025403784439,0.,0.5));
#22951=DIRECTION('ref_axis',(-0.5,0.,-0.866025403784439));
#22952=DIRECTION('',(-0.5,0.,-0.866025403784439));
#22953=DIRECTION('',(0.,-1.,0.));
#22954=DIRECTION('',(-0.5,0.,-0.866025403784439));
#22955=DIRECTION('center_axis',(-1.92296268638356E-16,0.,1.));
#22956=DIRECTION('ref_axis',(-1.,0.,-1.92296268638356E-16));
#22957=DIRECTION('',(-1.,0.,-1.92296268638356E-16));
#22958=DIRECTION('',(0.,-1.,0.));
#22959=DIRECTION('',(-1.,0.,-1.92296268638356E-16));
#22960=DIRECTION('center_axis',(0.866025403784439,0.,0.5));
#22961=DIRECTION('ref_axis',(-0.5,0.,0.866025403784439));
#22962=DIRECTION('',(-0.5,0.,0.866025403784439));
#22963=DIRECTION('',(-0.5,0.,0.866025403784439));
#22964=DIRECTION('center_axis',(0.,-1.,0.));
#22965=DIRECTION('ref_axis',(0.,0.,-1.));
#22966=DIRECTION('center_axis',(0.,1.,0.));
#22967=DIRECTION('ref_axis',(0.,0.,1.));
#22968=DIRECTION('center_axis',(0.,-1.,0.));
#22969=DIRECTION('ref_axis',(1.,0.,0.));
#22970=DIRECTION('center_axis',(0.,-1.,0.));
#22971=DIRECTION('ref_axis',(1.,0.,0.));
#22972=DIRECTION('center_axis',(0.,-1.,0.));
#22973=DIRECTION('ref_axis',(1.,0.,0.));
#22974=DIRECTION('',(0.707106781186547,0.707106781186548,8.65956056235493E-17));
#22975=DIRECTION('center_axis',(0.,-1.,0.));
#22976=DIRECTION('ref_axis',(1.,0.,0.));
#22977=DIRECTION('center_axis',(0.,1.,0.));
#22978=DIRECTION('ref_axis',(1.,0.,0.));
#22979=DIRECTION('',(0.,1.,0.));
#22980=DIRECTION('center_axis',(0.,1.,0.));
#22981=DIRECTION('ref_axis',(1.,0.,0.));
#22982=DIRECTION('center_axis',(0.,-1.,0.));
#22983=DIRECTION('ref_axis',(1.,0.,0.));
#22984=DIRECTION('',(-0.707106781186547,0.707106781186548,-8.65956056235493E-17));
#22985=DIRECTION('center_axis',(0.,-1.,0.));
#22986=DIRECTION('ref_axis',(0.,0.,-1.));
#22987=DIRECTION('axis',(0.,0.,1.));
#22988=DIRECTION('refdir',(1.,0.,0.));
#22989=DIRECTION('center_axis',(0.,1.,0.));
#22990=DIRECTION('ref_axis',(0.,0.,1.));
#22991=DIRECTION('center_axis',(0.,-1.,0.));
#22992=DIRECTION('ref_axis',(1.,0.,0.));
#22993=DIRECTION('center_axis',(0.,-1.,0.));
#22994=DIRECTION('ref_axis',(1.,0.,0.));
#22995=DIRECTION('center_axis',(0.,-1.,0.));
#22996=DIRECTION('ref_axis',(1.,0.,0.));
#22997=DIRECTION('',(0.707106781186547,0.707106781186548,8.65956056235493E-17));
#22998=DIRECTION('center_axis',(0.,-1.,0.));
#22999=DIRECTION('ref_axis',(1.,0.,0.));
#23000=DIRECTION('center_axis',(0.,-1.,0.));
#23001=DIRECTION('ref_axis',(1.,0.,0.));
#23002=DIRECTION('',(0.,1.,0.));
#23003=DIRECTION('center_axis',(0.,1.,0.));
#23004=DIRECTION('ref_axis',(1.,0.,0.));
#23005=DIRECTION('center_axis',(0.,-1.,0.));
#23006=DIRECTION('ref_axis',(1.,0.,0.));
#23007=DIRECTION('',(-0.707106781186547,0.707106781186548,-8.65956056235493E-17));
#23008=DIRECTION('center_axis',(0.,-1.,0.));
#23009=DIRECTION('ref_axis',(0.,0.,-1.));
#23010=DIRECTION('center_axis',(0.,-1.,0.));
#23011=DIRECTION('ref_axis',(1.,0.,0.));
#23012=DIRECTION('center_axis',(0.,1.,0.));
#23013=DIRECTION('ref_axis',(1.,0.,0.));
#23014=DIRECTION('center_axis',(0.,1.,0.));
#23015=DIRECTION('ref_axis',(1.,0.,0.));
#23016=DIRECTION('',(-0.447213595499958,0.894427190999916,-5.47678698264203E-17));
#23017=DIRECTION('center_axis',(0.,-1.,0.));
#23018=DIRECTION('ref_axis',(1.,0.,0.));
#23019=DIRECTION('center_axis',(0.,1.,0.));
#23020=DIRECTION('ref_axis',(1.,0.,0.));
#23021=DIRECTION('',(0.,1.,0.));
#23022=DIRECTION('center_axis',(0.,1.,0.));
#23023=DIRECTION('ref_axis',(1.,0.,0.));
#23024=DIRECTION('center_axis',(0.,-1.,0.));
#23025=DIRECTION('ref_axis',(1.,0.,0.));
#23026=DIRECTION('',(-0.707106781186547,0.707106781186548,-8.65956056235493E-17));
#23027=DIRECTION('center_axis',(0.,-1.,0.));
#23028=DIRECTION('ref_axis',(0.,0.,-1.));
#23029=DIRECTION('center_axis',(0.866025403784439,0.,-0.5));
#23030=DIRECTION('ref_axis',(0.5,0.,0.866025403784439));
#23031=DIRECTION('',(-0.5,0.,-0.866025403784439));
#23032=DIRECTION('',(0.,-1.,0.));
#23033=DIRECTION('',(0.5,0.,0.866025403784439));
#23034=DIRECTION('',(0.,-1.,0.));
#23035=DIRECTION('center_axis',(1.60246890531964E-16,0.,-1.));
#23036=DIRECTION('ref_axis',(1.,0.,1.60246890531964E-16));
#23037=DIRECTION('',(-1.,0.,-1.60246890531964E-16));
#23038=DIRECTION('',(0.,-1.,0.));
#23039=DIRECTION('',(1.,0.,1.60246890531964E-16));
#23040=DIRECTION('center_axis',(-0.866025403784439,0.,-0.5));
#23041=DIRECTION('ref_axis',(0.5,0.,-0.866025403784439));
#23042=DIRECTION('',(-0.5,0.,0.866025403784439));
#23043=DIRECTION('',(0.,-1.,0.));
#23044=DIRECTION('',(0.5,0.,-0.866025403784439));
#23045=DIRECTION('center_axis',(-0.866025403784439,0.,0.5));
#23046=DIRECTION('ref_axis',(-0.5,0.,-0.866025403784439));
#23047=DIRECTION('',(0.5,0.,0.866025403784439));
#23048=DIRECTION('',(0.,-1.,0.));
#23049=DIRECTION('',(-0.5,0.,-0.866025403784439));
#23050=DIRECTION('center_axis',(-1.60246890531964E-16,0.,1.));
#23051=DIRECTION('ref_axis',(-1.,0.,-1.60246890531964E-16));
#23052=DIRECTION('',(1.,0.,1.60246890531964E-16));
#23053=DIRECTION('',(0.,-1.,0.));
#23054=DIRECTION('',(-1.,0.,-1.60246890531964E-16));
#23055=DIRECTION('center_axis',(0.866025403784439,0.,0.5));
#23056=DIRECTION('ref_axis',(-0.5,0.,0.866025403784439));
#23057=DIRECTION('',(0.5,0.,-0.866025403784439));
#23058=DIRECTION('',(-0.5,0.,0.866025403784439));
#23059=DIRECTION('center_axis',(0.,1.,0.));
#23060=DIRECTION('ref_axis',(1.,0.,0.));
#23061=DIRECTION('center_axis',(0.,-1.,0.));
#23062=DIRECTION('ref_axis',(0.,0.,-1.));
#23063=DIRECTION('',(0.,0.,1.));
#23064=DIRECTION('',(1.,0.,0.));
#23065=DIRECTION('',(0.,0.,1.));
#23066=DIRECTION('',(1.,0.,0.));
#23067=DIRECTION('',(0.,0.,1.));
#23068=DIRECTION('',(1.,0.,0.));
#23069=DIRECTION('',(0.,0.,1.));
#23070=DIRECTION('',(1.,0.,0.));
#23071=DIRECTION('',(0.,0.,1.));
#23072=DIRECTION('',(1.,0.,0.));
#23073=DIRECTION('',(0.,0.,1.));
#23074=DIRECTION('',(1.,0.,0.));
#23075=DIRECTION('',(0.,-1.,2.22044604925031E-16));
#23076=DIRECTION('',(1.,0.,0.));
#23077=DIRECTION('',(0.,-1.,2.22044604925031E-16));
#23078=DIRECTION('',(1.,0.,0.));
#23079=DIRECTION('',(0.,-1.,2.22044604925031E-16));
#23080=DIRECTION('',(1.,0.,0.));
#23081=DIRECTION('',(0.,0.,1.));
#23082=DIRECTION('',(1.,0.,0.));
#23083=DIRECTION('',(0.,0.,1.));
#23084=DIRECTION('',(-1.,1.22464679914735E-16,0.));
#23085=DIRECTION('',(0.,0.,1.));
#23086=DIRECTION('',(-1.,1.22464679914735E-16,0.));
#23087=DIRECTION('',(0.,0.,1.));
#23088=DIRECTION('',(-1.,1.22464679914735E-16,0.));
#23089=DIRECTION('',(0.,0.,1.));
#23090=DIRECTION('',(-1.,1.22464679914735E-16,0.));
#23091=DIRECTION('',(0.,0.,1.));
#23092=DIRECTION('',(1.,0.,0.));
#23093=DIRECTION('',(0.,0.,1.));
#23094=DIRECTION('',(1.,0.,0.));
#23095=DIRECTION('',(0.,0.,1.));
#23096=DIRECTION('',(1.,0.,0.));
#23097=DIRECTION('',(0.,0.,1.));
#23098=DIRECTION('',(1.,0.,0.));
#23099=DIRECTION('',(0.,0.,1.));
#23100=DIRECTION('',(1.,0.,0.));
#23101=DIRECTION('',(0.,0.,1.));
#23102=DIRECTION('',(-1.,1.22464679914735E-16,0.));
#23103=DIRECTION('',(0.,0.,1.));
#23104=DIRECTION('',(-1.,1.22464679914735E-16,0.));
#23105=DIRECTION('',(0.,0.,1.));
#23106=DIRECTION('',(-1.,1.22464679914735E-16,0.));
#23107=DIRECTION('',(0.,0.,1.));
#23108=DIRECTION('',(-1.,1.22464679914735E-16,0.));
#23109=DIRECTION('',(0.,0.,1.));
#23110=DIRECTION('',(1.,0.,0.));
#23111=DIRECTION('',(0.,0.,1.));
#23112=DIRECTION('',(1.,0.,0.));
#23113=DIRECTION('',(0.,0.,1.));
#23114=DIRECTION('',(1.,0.,0.));
#23115=DIRECTION('',(0.,0.,1.));
#23116=DIRECTION('',(1.,0.,0.));
#23117=DIRECTION('',(0.,0.,1.));
#23118=DIRECTION('',(1.,0.,0.));
#23119=DIRECTION('',(0.,0.,1.));
#23120=DIRECTION('',(1.,0.,0.));
#23121=DIRECTION('',(0.,0.,1.));
#23122=DIRECTION('',(1.,0.,0.));
#23123=DIRECTION('',(0.,0.,1.));
#23124=DIRECTION('',(1.,0.,0.));
#23125=DIRECTION('',(0.,0.,1.));
#23126=DIRECTION('',(1.,0.,0.));
#23127=DIRECTION('',(0.,0.,1.));
#23128=DIRECTION('',(-1.,1.22464679914735E-16,0.));
#23129=DIRECTION('',(0.,0.,1.));
#23130=DIRECTION('',(-1.,1.22464679914735E-16,0.));
#23131=DIRECTION('',(0.,0.,1.));
#23132=DIRECTION('',(-1.,1.22464679914735E-16,0.));
#23133=DIRECTION('',(0.,0.,1.));
#23134=DIRECTION('',(-1.,1.22464679914735E-16,0.));
#23135=DIRECTION('',(0.,0.,1.));
#23136=DIRECTION('',(1.,0.,0.));
#23137=DIRECTION('',(0.,0.,1.));
#23138=DIRECTION('',(1.,0.,0.));
#23139=DIRECTION('',(0.,0.,1.));
#23140=DIRECTION('',(1.,0.,0.));
#23141=DIRECTION('',(0.,0.,1.));
#23142=DIRECTION('',(1.,0.,0.));
#23143=DIRECTION('',(0.,0.,1.));
#23144=DIRECTION('',(1.,0.,0.));
#23145=DIRECTION('',(0.,0.,1.));
#23146=DIRECTION('',(-1.,1.22464679914735E-16,0.));
#23147=DIRECTION('',(0.,0.,1.));
#23148=DIRECTION('',(-1.,1.22464679914735E-16,0.));
#23149=DIRECTION('',(0.,0.,1.));
#23150=DIRECTION('',(-1.,1.22464679914735E-16,0.));
#23151=DIRECTION('',(0.,0.,1.));
#23152=DIRECTION('',(-1.,1.22464679914735E-16,0.));
#23153=DIRECTION('',(0.,0.,1.));
#23154=DIRECTION('',(1.,0.,0.));
#23155=DIRECTION('',(0.,0.,1.));
#23156=DIRECTION('',(1.,0.,0.));
#23157=DIRECTION('',(0.,0.,1.));
#23158=DIRECTION('',(1.,0.,0.));
#23159=DIRECTION('',(0.,0.,1.));
#23160=DIRECTION('',(1.,0.,0.));
#23161=DIRECTION('',(0.,0.,1.));
#23162=DIRECTION('',(1.,0.,0.));
#23163=DIRECTION('',(0.,0.,1.));
#23164=DIRECTION('',(1.,0.,0.));
#23165=DIRECTION('',(0.,0.,1.));
#23166=DIRECTION('',(1.,0.,0.));
#23167=DIRECTION('',(0.,0.,1.));
#23168=DIRECTION('',(1.,0.,0.));
#23169=DIRECTION('',(0.,0.,1.));
#23170=DIRECTION('',(1.,0.,0.));
#23171=DIRECTION('',(0.,0.,1.));
#23172=DIRECTION('',(1.,0.,0.));
#23173=DIRECTION('',(0.,0.,1.));
#23174=DIRECTION('',(-1.,1.22464679914735E-16,0.));
#23175=DIRECTION('',(0.,0.,1.));
#23176=DIRECTION('',(1.,0.,0.));
#23177=DIRECTION('',(0.,0.,1.));
#23178=DIRECTION('',(-1.,1.22464679914735E-16,0.));
#23179=DIRECTION('',(0.,0.,1.));
#23180=DIRECTION('',(1.,0.,0.));
#23181=DIRECTION('',(0.,0.,1.));
#23182=DIRECTION('',(1.,0.,0.));
#23183=DIRECTION('',(0.,0.,1.));
#23184=DIRECTION('',(1.,0.,0.));
#23185=DIRECTION('',(0.,0.,1.));
#23186=DIRECTION('',(1.,0.,0.));
#23187=DIRECTION('',(0.,0.,1.));
#23188=DIRECTION('',(1.,0.,0.));
#23189=DIRECTION('',(0.,0.,1.));
#23190=DIRECTION('',(1.,0.,0.));
#23191=DIRECTION('',(0.,0.,1.));
#23192=DIRECTION('',(1.,0.,0.));
#23193=DIRECTION('',(0.,0.,1.));
#23194=DIRECTION('',(1.,0.,0.));
#23195=DIRECTION('',(0.,0.,1.));
#23196=DIRECTION('',(1.,0.,0.));
#23197=DIRECTION('',(0.,-1.,2.22044604925031E-16));
#23198=DIRECTION('',(1.,0.,0.));
#23199=DIRECTION('',(0.,0.,1.));
#23200=DIRECTION('',(1.,0.,0.));
#23201=DIRECTION('',(8.65956056235493E-17,-8.65956056235493E-17,-1.));
#23202=DIRECTION('',(2.22044604925031E-16,1.,-8.65956056235494E-17));
#23203=DIRECTION('',(8.65956056235493E-17,-8.65956056235493E-17,-1.));
#23204=DIRECTION('',(2.22044604925031E-16,1.,-8.65956056235494E-17));
#23205=DIRECTION('',(0.,0.,1.));
#23206=DIRECTION('',(1.,0.,0.));
#23207=DIRECTION('',(0.,0.,1.));
#23208=DIRECTION('',(1.,0.,0.));
#23209=DIRECTION('',(0.,0.,1.));
#23210=DIRECTION('',(1.,0.,0.));
#23211=DIRECTION('',(0.,0.,1.));
#23212=DIRECTION('',(1.,0.,0.));
#23213=DIRECTION('',(0.,0.,1.));
#23214=DIRECTION('',(1.,0.,0.));
#23215=DIRECTION('',(0.,0.,1.));
#23216=DIRECTION('',(1.,0.,0.));
#23217=DIRECTION('',(0.,0.,1.));
#23218=DIRECTION('',(1.,0.,0.));
#23219=DIRECTION('',(0.,0.,1.));
#23220=DIRECTION('',(1.,0.,0.));
#23221=DIRECTION('',(0.,-1.,2.22044604925031E-16));
#23222=DIRECTION('',(1.,0.,0.));
#23223=DIRECTION('',(0.,0.,1.));
#23224=DIRECTION('',(1.,0.,0.));
#23225=DIRECTION('',(8.65956056235493E-17,-8.65956056235493E-17,-1.));
#23226=DIRECTION('',(2.22044604925031E-16,1.,-8.65956056235494E-17));
#23227=DIRECTION('',(0.,0.,1.));
#23228=DIRECTION('',(1.,0.,0.));
#23229=DIRECTION('',(0.,0.,1.));
#23230=DIRECTION('',(1.,0.,0.));
#23231=DIRECTION('',(0.,0.,1.));
#23232=DIRECTION('',(1.,0.,0.));
#23233=DIRECTION('',(0.,0.,1.));
#23234=DIRECTION('',(1.,0.,0.));
#23235=DIRECTION('',(0.,0.,1.));
#23236=DIRECTION('',(1.,0.,0.));
#23237=DIRECTION('',(0.,0.,1.));
#23238=DIRECTION('',(1.,0.,0.));
#23239=DIRECTION('',(0.,-1.,2.22044604925031E-16));
#23240=DIRECTION('',(1.,0.,0.));
#23241=DIRECTION('',(0.,0.,1.));
#23242=DIRECTION('',(1.,0.,0.));
#23243=DIRECTION('',(8.65956056235493E-17,-8.65956056235493E-17,-1.));
#23244=DIRECTION('',(2.22044604925031E-16,1.,-8.65956056235494E-17));
#23245=DIRECTION('',(0.,0.,1.));
#23246=DIRECTION('',(1.,0.,0.));
#23247=DIRECTION('',(0.,0.,1.));
#23248=DIRECTION('',(1.,0.,0.));
#23249=DIRECTION('',(0.,0.,1.));
#23250=DIRECTION('',(1.,0.,0.));
#23251=DIRECTION('',(0.,0.,1.));
#23252=DIRECTION('',(1.,0.,0.));
#23253=DIRECTION('',(0.,0.,1.));
#23254=DIRECTION('',(1.,0.,0.));
#23255=DIRECTION('',(0.,0.,1.));
#23256=DIRECTION('',(1.,0.,0.));
#23257=DIRECTION('',(0.,0.,1.));
#23258=DIRECTION('',(1.,0.,0.));
#23259=DIRECTION('',(0.,0.,1.));
#23260=DIRECTION('',(1.,0.,0.));
#23261=DIRECTION('',(0.,0.,1.));
#23262=DIRECTION('',(1.,0.,0.));
#23263=DIRECTION('',(0.,-1.,2.22044604925031E-16));
#23264=DIRECTION('',(1.,0.,0.));
#23265=DIRECTION('',(0.,0.,1.));
#23266=DIRECTION('',(1.,0.,0.));
#23267=DIRECTION('',(8.32667268468868E-17,-8.65956056235493E-17,-1.));
#23268=DIRECTION('',(2.22044604925031E-16,1.,-8.65956056235494E-17));
#23269=DIRECTION('',(0.,-1.,2.22044604925031E-16));
#23270=DIRECTION('',(1.,0.,0.));
#23271=DIRECTION('',(0.,0.,1.));
#23272=DIRECTION('',(1.,0.,0.));
#23273=DIRECTION('axis',(0.,0.,1.));
#23274=DIRECTION('refdir',(1.,0.,0.));
#23275=DIRECTION('axis',(0.,0.,1.));
#23276=DIRECTION('refdir',(1.,0.,0.));
#23277=DIRECTION('center_axis',(0.,1.,0.));
#23278=DIRECTION('ref_axis',(1.,0.,0.));
#23279=DIRECTION('center_axis',(0.,-1.,0.));
#23280=DIRECTION('ref_axis',(1.,0.,0.));
#23281=DIRECTION('',(0.,-1.,0.));
#23282=DIRECTION('center_axis',(0.,-1.,0.));
#23283=DIRECTION('ref_axis',(1.,0.,0.));
#23284=DIRECTION('center_axis',(0.,1.,0.));
#23285=DIRECTION('ref_axis',(1.,0.,0.));
#23286=DIRECTION('center_axis',(0.,1.,0.));
#23287=DIRECTION('ref_axis',(1.,0.,0.));
#23288=DIRECTION('',(0.,-1.,0.));
#23289=DIRECTION('center_axis',(0.,1.,0.));
#23290=DIRECTION('ref_axis',(1.,0.,0.));
#23291=DIRECTION('center_axis',(0.,1.,0.));
#23292=DIRECTION('ref_axis',(1.,0.,0.));
#23293=DIRECTION('center_axis',(0.,1.,0.));
#23294=DIRECTION('ref_axis',(1.,0.,0.));
#23295=DIRECTION('',(0.,0.,1.));
#23296=DIRECTION('',(1.,0.,0.));
#23297=DIRECTION('',(0.,0.,1.));
#23298=DIRECTION('',(1.,0.,0.));
#23299=DIRECTION('',(0.,0.,1.));
#23300=DIRECTION('',(1.,0.,0.));
#23301=DIRECTION('',(0.0784590957278449,0.,0.996917333733128));
#23302=DIRECTION('',(0.996917333733128,0.,-0.0784590957278449));
#23303=DIRECTION('',(0.,0.,1.));
#23304=DIRECTION('',(1.,0.,0.));
#23305=DIRECTION('',(0.0784590957278449,0.,0.996917333733128));
#23306=DIRECTION('',(0.996917333733128,0.,-0.0784590957278449));
#23307=DIRECTION('',(0.,0.,1.));
#23308=DIRECTION('',(1.,0.,0.));
#23309=CARTESIAN_POINT('',(0.,0.,0.));
#23310=CARTESIAN_POINT('',(0.,0.,0.));
#23311=CARTESIAN_POINT('',(0.,0.,0.));
#23312=CARTESIAN_POINT('Origin',(-2.,-5.,-0.1));
#23313=CARTESIAN_POINT('',(-2.25,-5.,0.));
#23314=CARTESIAN_POINT('Origin',(-2.,-5.,0.));
#23315=CARTESIAN_POINT('',(-2.25,-5.,1.));
#23316=CARTESIAN_POINT('',(-2.25,-5.,-0.1));
#23317=CARTESIAN_POINT('Origin',(-2.,-5.,1.));
#23318=CARTESIAN_POINT('Origin',(9.,-5.,-0.1));
#23319=CARTESIAN_POINT('',(8.75,-5.,0.));
#23320=CARTESIAN_POINT('Origin',(9.,-5.,0.));
#23321=CARTESIAN_POINT('',(8.75,-5.,1.));
#23322=CARTESIAN_POINT('',(8.75,-5.,-0.1));
#23323=CARTESIAN_POINT('Origin',(9.,-5.,1.));
#23324=CARTESIAN_POINT('Origin',(22.,-5.,-0.1));
#23325=CARTESIAN_POINT('',(21.75,-5.,0.));
#23326=CARTESIAN_POINT('Origin',(22.,-5.,0.));
#23327=CARTESIAN_POINT('',(21.75,-5.,1.));
#23328=CARTESIAN_POINT('',(21.75,-5.,-0.1));
#23329=CARTESIAN_POINT('Origin',(22.,-5.,1.));
#23330=CARTESIAN_POINT('Origin',(24.,6.5,0.));
#23331=CARTESIAN_POINT('',(24.,6.5,0.));
#23332=CARTESIAN_POINT('',(-4.,6.5,0.));
#23333=CARTESIAN_POINT('',(24.,6.5,0.));
#23334=CARTESIAN_POINT('',(-4.,6.5,1.));
#23335=CARTESIAN_POINT('',(-4.,6.5,0.));
#23336=CARTESIAN_POINT('',(24.,6.5,1.));
#23337=CARTESIAN_POINT('',(24.,6.5,1.));
#23338=CARTESIAN_POINT('',(24.,6.5,0.));
#23339=CARTESIAN_POINT('Origin',(24.,-6.5,0.));
#23340=CARTESIAN_POINT('',(24.,-6.5,0.));
#23341=CARTESIAN_POINT('',(24.,-6.5,0.));
#23342=CARTESIAN_POINT('',(24.,-6.5,1.));
#23343=CARTESIAN_POINT('',(24.,-6.5,1.));
#23344=CARTESIAN_POINT('',(24.,-6.5,0.));
#23345=CARTESIAN_POINT('Origin',(-4.,-6.5,0.));
#23346=CARTESIAN_POINT('',(-4.,-6.5,0.));
#23347=CARTESIAN_POINT('',(-4.,-6.5,0.));
#23348=CARTESIAN_POINT('',(-4.,-6.5,1.));
#23349=CARTESIAN_POINT('',(-4.,-6.5,1.));
#23350=CARTESIAN_POINT('',(-4.,-6.5,0.));
#23351=CARTESIAN_POINT('Origin',(-4.,6.5,0.));
#23352=CARTESIAN_POINT('',(-4.,6.5,0.));
#23353=CARTESIAN_POINT('',(-4.,6.5,1.));
#23354=CARTESIAN_POINT('Origin',(10.,0.,1.));
#23355=CARTESIAN_POINT('Origin',(10.,0.,0.));
#23356=CARTESIAN_POINT('',(0.,0.,0.));
#23357=CARTESIAN_POINT('Origin',(23.,-2.5,14.));
#23358=CARTESIAN_POINT('',(22.775,-2.4,14.));
#23359=CARTESIAN_POINT('Origin',(23.,-2.4,14.));
#23360=CARTESIAN_POINT('',(22.775,-0.6,14.));
#23361=CARTESIAN_POINT('',(22.775,-2.5,14.));
#23362=CARTESIAN_POINT('Origin',(23.,-0.6,14.));
#23363=CARTESIAN_POINT('Origin',(23.,-2.5,4.));
#23364=CARTESIAN_POINT('',(22.775,-2.4,4.));
#23365=CARTESIAN_POINT('Origin',(23.,-2.4,4.));
#23366=CARTESIAN_POINT('',(22.775,-0.6,4.));
#23367=CARTESIAN_POINT('',(22.775,-2.5,4.));
#23368=CARTESIAN_POINT('Origin',(23.,-0.6,4.));
#23369=CARTESIAN_POINT('Origin',(16.161522368915,-2.5,7.16152236891498));
#23370=CARTESIAN_POINT('',(15.996522368915,-2.4,7.16152236891498));
#23371=CARTESIAN_POINT('Origin',(16.161522368915,-2.4,7.16152236891498));
#23372=CARTESIAN_POINT('',(15.996522368915,-0.6,7.16152236891498));
#23373=CARTESIAN_POINT('',(15.996522368915,-2.5,7.16152236891498));
#23374=CARTESIAN_POINT('Origin',(16.161522368915,-0.6,7.16152236891498));
#23375=CARTESIAN_POINT('Origin',(16.161522368915,-2.5,10.838477631085));
#23376=CARTESIAN_POINT('',(15.996522368915,-2.4,10.838477631085));
#23377=CARTESIAN_POINT('Origin',(16.161522368915,-2.4,10.838477631085));
#23378=CARTESIAN_POINT('',(15.996522368915,-0.6,10.838477631085));
#23379=CARTESIAN_POINT('',(15.996522368915,-2.5,10.838477631085));
#23380=CARTESIAN_POINT('Origin',(16.161522368915,-0.6,10.838477631085));
#23381=CARTESIAN_POINT('Origin',(19.838477631085,-2.5,10.838477631085));
#23382=CARTESIAN_POINT('',(19.673477631085,-2.4,10.838477631085));
#23383=CARTESIAN_POINT('Origin',(19.838477631085,-2.4,10.838477631085));
#23384=CARTESIAN_POINT('',(19.673477631085,-0.6,10.838477631085));
#23385=CARTESIAN_POINT('',(19.673477631085,-2.5,10.838477631085));
#23386=CARTESIAN_POINT('Origin',(19.838477631085,-0.6,10.838477631085));
#23387=CARTESIAN_POINT('Origin',(19.838477631085,-2.5,7.16152236891498));
#23388=CARTESIAN_POINT('',(19.673477631085,-2.4,7.16152236891498));
#23389=CARTESIAN_POINT('Origin',(19.838477631085,-2.4,7.16152236891498));
#23390=CARTESIAN_POINT('',(19.673477631085,-0.6,7.16152236891498));
#23391=CARTESIAN_POINT('',(19.673477631085,-2.5,7.16152236891498));
#23392=CARTESIAN_POINT('Origin',(19.838477631085,-0.6,7.16152236891498));
#23393=CARTESIAN_POINT('Origin',(18.,-2.5,9.));
#23394=CARTESIAN_POINT('',(15.65,-2.4,9.));
#23395=CARTESIAN_POINT('Origin',(18.,-2.4,9.));
#23396=CARTESIAN_POINT('',(15.65,-0.6,9.));
#23397=CARTESIAN_POINT('',(15.65,-2.5,9.));
#23398=CARTESIAN_POINT('Origin',(18.,-0.6,9.));
#23399=CARTESIAN_POINT('Origin',(10.5150757595082,-2.5,7.51507575950825));
#23400=CARTESIAN_POINT('',(10.3500757595083,-2.4,7.51507575950825));
#23401=CARTESIAN_POINT('Origin',(10.5150757595082,-2.4,7.51507575950825));
#23402=CARTESIAN_POINT('',(10.3500757595083,-0.6,7.51507575950825));
#23403=CARTESIAN_POINT('',(10.3500757595083,-2.5,7.51507575950825));
#23404=CARTESIAN_POINT('Origin',(10.5150757595082,-0.6,7.51507575950825));
#23405=CARTESIAN_POINT('Origin',(10.5150757595082,-2.5,10.4849242404918));
#23406=CARTESIAN_POINT('',(10.3500757595083,-2.4,10.4849242404918));
#23407=CARTESIAN_POINT('Origin',(10.5150757595082,-2.4,10.4849242404918));
#23408=CARTESIAN_POINT('',(10.3500757595083,-0.6,10.4849242404918));
#23409=CARTESIAN_POINT('',(10.3500757595083,-2.5,10.4849242404918));
#23410=CARTESIAN_POINT('Origin',(10.5150757595082,-0.6,10.4849242404918));
#23411=CARTESIAN_POINT('Origin',(13.4849242404918,-2.5,10.4849242404918));
#23412=CARTESIAN_POINT('',(13.3199242404918,-2.4,10.4849242404918));
#23413=CARTESIAN_POINT('Origin',(13.4849242404918,-2.4,10.4849242404918));
#23414=CARTESIAN_POINT('',(13.3199242404918,-0.6,10.4849242404918));
#23415=CARTESIAN_POINT('',(13.3199242404918,-2.5,10.4849242404918));
#23416=CARTESIAN_POINT('Origin',(13.4849242404918,-0.6,10.4849242404918));
#23417=CARTESIAN_POINT('Origin',(13.4849242404918,-2.5,7.51507575950825));
#23418=CARTESIAN_POINT('',(13.3199242404918,-2.4,7.51507575950825));
#23419=CARTESIAN_POINT('Origin',(13.4849242404918,-2.4,7.51507575950825));
#23420=CARTESIAN_POINT('',(13.3199242404918,-0.6,7.51507575950825));
#23421=CARTESIAN_POINT('',(13.3199242404918,-2.5,7.51507575950825));
#23422=CARTESIAN_POINT('Origin',(13.4849242404918,-0.6,7.51507575950825));
#23423=CARTESIAN_POINT('Origin',(12.,-2.5,9.));
#23424=CARTESIAN_POINT('',(10.4,-2.4,9.));
#23425=CARTESIAN_POINT('Origin',(12.,-2.4,9.));
#23426=CARTESIAN_POINT('',(10.4,-0.6,9.));
#23427=CARTESIAN_POINT('',(10.4,-2.5,9.));
#23428=CARTESIAN_POINT('Origin',(12.,-0.6,9.));
#23429=CARTESIAN_POINT('Origin',(4.16152236891498,-2.5,7.16152236891498));
#23430=CARTESIAN_POINT('',(3.99652236891498,-2.4,7.16152236891498));
#23431=CARTESIAN_POINT('Origin',(4.16152236891498,-2.4,7.16152236891498));
#23432=CARTESIAN_POINT('',(3.99652236891498,-0.6,7.16152236891498));
#23433=CARTESIAN_POINT('',(3.99652236891498,-2.5,7.16152236891498));
#23434=CARTESIAN_POINT('Origin',(4.16152236891498,-0.6,7.16152236891498));
#23435=CARTESIAN_POINT('Origin',(4.16152236891498,-2.5,10.838477631085));
#23436=CARTESIAN_POINT('',(3.99652236891498,-2.4,10.838477631085));
#23437=CARTESIAN_POINT('Origin',(4.16152236891498,-2.4,10.838477631085));
#23438=CARTESIAN_POINT('',(3.99652236891498,-0.6,10.838477631085));
#23439=CARTESIAN_POINT('',(3.99652236891498,-2.5,10.838477631085));
#23440=CARTESIAN_POINT('Origin',(4.16152236891498,-0.6,10.838477631085));
#23441=CARTESIAN_POINT('Origin',(7.83847763108502,-2.5,10.838477631085));
#23442=CARTESIAN_POINT('',(7.67347763108502,-2.4,10.838477631085));
#23443=CARTESIAN_POINT('Origin',(7.83847763108502,-2.4,10.838477631085));
#23444=CARTESIAN_POINT('',(7.67347763108502,-0.6,10.838477631085));
#23445=CARTESIAN_POINT('',(7.67347763108502,-2.5,10.838477631085));
#23446=CARTESIAN_POINT('Origin',(7.83847763108502,-0.6,10.838477631085));
#23447=CARTESIAN_POINT('Origin',(7.83847763108502,-2.5,7.16152236891498));
#23448=CARTESIAN_POINT('',(7.67347763108502,-2.4,7.16152236891498));
#23449=CARTESIAN_POINT('Origin',(7.83847763108502,-2.4,7.16152236891498));
#23450=CARTESIAN_POINT('',(7.67347763108502,-0.6,7.16152236891498));
#23451=CARTESIAN_POINT('',(7.67347763108502,-2.5,7.16152236891498));
#23452=CARTESIAN_POINT('Origin',(7.83847763108502,-0.6,7.16152236891498));
#23453=CARTESIAN_POINT('Origin',(6.,-2.5,9.));
#23454=CARTESIAN_POINT('',(3.65,-2.4,9.));
#23455=CARTESIAN_POINT('Origin',(6.,-2.4,9.));
#23456=CARTESIAN_POINT('',(3.65,-0.6,9.));
#23457=CARTESIAN_POINT('',(3.65,-2.5,9.));
#23458=CARTESIAN_POINT('Origin',(6.,-0.6,9.));
#23459=CARTESIAN_POINT('Origin',(-1.48492424049175,-2.5,7.51507575950825));
#23460=CARTESIAN_POINT('',(-1.64992424049175,-2.4,7.51507575950825));
#23461=CARTESIAN_POINT('Origin',(-1.48492424049175,-2.4,7.51507575950825));
#23462=CARTESIAN_POINT('',(-1.64992424049175,-0.6,7.51507575950825));
#23463=CARTESIAN_POINT('',(-1.64992424049175,-2.5,7.51507575950825));
#23464=CARTESIAN_POINT('Origin',(-1.48492424049175,-0.6,7.51507575950825));
#23465=CARTESIAN_POINT('Origin',(-1.48492424049175,-2.5,10.4849242404918));
#23466=CARTESIAN_POINT('',(-1.64992424049175,-2.4,10.4849242404918));
#23467=CARTESIAN_POINT('Origin',(-1.48492424049175,-2.4,10.4849242404918));
#23468=CARTESIAN_POINT('',(-1.64992424049175,-0.6,10.4849242404918));
#23469=CARTESIAN_POINT('',(-1.64992424049175,-2.5,10.4849242404918));
#23470=CARTESIAN_POINT('Origin',(-1.48492424049175,-0.6,10.4849242404918));
#23471=CARTESIAN_POINT('Origin',(1.48492424049175,-2.5,10.4849242404918));
#23472=CARTESIAN_POINT('',(1.31992424049175,-2.4,10.4849242404918));
#23473=CARTESIAN_POINT('Origin',(1.48492424049175,-2.4,10.4849242404918));
#23474=CARTESIAN_POINT('',(1.31992424049175,-0.6,10.4849242404918));
#23475=CARTESIAN_POINT('',(1.31992424049175,-2.5,10.4849242404918));
#23476=CARTESIAN_POINT('Origin',(1.48492424049175,-0.6,10.4849242404918));
#23477=CARTESIAN_POINT('Origin',(1.48492424049175,-2.5,7.51507575950825));
#23478=CARTESIAN_POINT('',(1.31992424049175,-2.4,7.51507575950825));
#23479=CARTESIAN_POINT('Origin',(1.48492424049175,-2.4,7.51507575950825));
#23480=CARTESIAN_POINT('',(1.31992424049175,-0.6,7.51507575950825));
#23481=CARTESIAN_POINT('',(1.31992424049175,-2.5,7.51507575950825));
#23482=CARTESIAN_POINT('Origin',(1.48492424049175,-0.6,7.51507575950825));
#23483=CARTESIAN_POINT('Origin',(0.,-2.5,9.));
#23484=CARTESIAN_POINT('',(-1.6,-2.4,9.));
#23485=CARTESIAN_POINT('Origin',(0.,-2.4,9.));
#23486=CARTESIAN_POINT('',(-1.6,-0.6,9.));
#23487=CARTESIAN_POINT('',(-1.6,-2.5,9.));
#23488=CARTESIAN_POINT('Origin',(0.,-0.6,9.));
#23489=CARTESIAN_POINT('Origin',(-2.,-5.,0.9));
#23490=CARTESIAN_POINT('',(-2.33,-5.,1.));
#23491=CARTESIAN_POINT('Origin',(-2.,-5.,1.));
#23492=CARTESIAN_POINT('',(-2.33,-5.,2.));
#23493=CARTESIAN_POINT('',(-2.33,-5.,0.9));
#23494=CARTESIAN_POINT('Origin',(-2.,-5.,2.));
#23495=CARTESIAN_POINT('Origin',(9.,-5.,0.9));
#23496=CARTESIAN_POINT('',(8.67,-5.,1.));
#23497=CARTESIAN_POINT('Origin',(9.,-5.,1.));
#23498=CARTESIAN_POINT('',(8.67,-5.,2.));
#23499=CARTESIAN_POINT('',(8.67,-5.,0.9));
#23500=CARTESIAN_POINT('Origin',(9.,-5.,2.));
#23501=CARTESIAN_POINT('Origin',(22.,-5.,0.9));
#23502=CARTESIAN_POINT('',(21.67,-5.,1.));
#23503=CARTESIAN_POINT('Origin',(22.,-5.,1.));
#23504=CARTESIAN_POINT('',(21.67,-5.,2.));
#23505=CARTESIAN_POINT('',(21.67,-5.,0.9));
#23506=CARTESIAN_POINT('Origin',(22.,-5.,2.));
#23507=CARTESIAN_POINT('Origin',(-3.5,-6.,2.));
#23508=CARTESIAN_POINT('',(23.5,-6.,2.));
#23509=CARTESIAN_POINT('',(-3.5,-6.,2.));
#23510=CARTESIAN_POINT('',(23.5,-6.,2.));
#23511=CARTESIAN_POINT('',(23.5,-2.4,2.));
#23512=CARTESIAN_POINT('',(23.5,-6.,2.));
#23513=CARTESIAN_POINT('',(-3.5,-2.4,2.));
#23514=CARTESIAN_POINT('',(-3.5,-2.4,2.));
#23515=CARTESIAN_POINT('',(-3.5,-6.,2.));
#23516=CARTESIAN_POINT('Origin',(10.,-6.,1.5));
#23517=CARTESIAN_POINT('',(-3.5,-6.,1.));
#23518=CARTESIAN_POINT('',(-3.5,-6.,2.));
#23519=CARTESIAN_POINT('',(23.5,-6.,1.));
#23520=CARTESIAN_POINT('',(-3.5,-6.,1.));
#23521=CARTESIAN_POINT('',(23.5,-6.,1.));
#23522=CARTESIAN_POINT('Origin',(23.5,-0.6,1.));
#23523=CARTESIAN_POINT('',(23.5,-0.6,1.));
#23524=CARTESIAN_POINT('',(-3.5,-0.6,1.));
#23525=CARTESIAN_POINT('',(23.5,-0.6,1.));
#23526=CARTESIAN_POINT('',(-3.5,-0.6,16.));
#23527=CARTESIAN_POINT('',(-3.5,-0.6,1.));
#23528=CARTESIAN_POINT('',(23.5,-0.6,16.));
#23529=CARTESIAN_POINT('',(23.5,-0.6,16.));
#23530=CARTESIAN_POINT('',(23.5,-0.6,1.));
#23531=CARTESIAN_POINT('Origin',(23.5,-2.4,1.));
#23532=CARTESIAN_POINT('',(23.5,-6.,1.));
#23533=CARTESIAN_POINT('',(23.5,-2.4,16.));
#23534=CARTESIAN_POINT('',(23.5,-2.4,16.));
#23535=CARTESIAN_POINT('',(23.5,-2.4,1.));
#23536=CARTESIAN_POINT('Origin',(-3.5,-2.4,1.));
#23537=CARTESIAN_POINT('',(-3.5,-2.4,16.));
#23538=CARTESIAN_POINT('',(-3.5,-2.4,16.));
#23539=CARTESIAN_POINT('',(-3.5,-2.4,1.));
#23540=CARTESIAN_POINT('Origin',(-3.5,-0.6,1.));
#23541=CARTESIAN_POINT('',(-3.5,-0.6,1.));
#23542=CARTESIAN_POINT('',(-3.5,-0.6,16.));
#23543=CARTESIAN_POINT('Origin',(10.,-1.5,16.));
#23544=CARTESIAN_POINT('Origin',(10.,-1.5,1.));
#23545=CARTESIAN_POINT('',(0.,0.,0.));
#23546=CARTESIAN_POINT('Origin',(-1.48492424049175,-2.7,7.51507575950825));
#23547=CARTESIAN_POINT('',(-1.70992424049175,-2.6,7.51507575950825));
#23548=CARTESIAN_POINT('Origin',(-1.48492424049175,-2.6,7.51507575950825));
#23549=CARTESIAN_POINT('',(-1.70992424049175,-2.4,7.51507575950825));
#23550=CARTESIAN_POINT('',(-1.70992424049175,-2.7,7.51507575950825));
#23551=CARTESIAN_POINT('Origin',(-1.48492424049175,-2.4,7.51507575950825));
#23552=CARTESIAN_POINT('Origin',(-1.48492424049175,-2.7,10.4849242404918));
#23553=CARTESIAN_POINT('',(-1.70992424049175,-2.6,10.4849242404918));
#23554=CARTESIAN_POINT('Origin',(-1.48492424049175,-2.6,10.4849242404918));
#23555=CARTESIAN_POINT('',(-1.70992424049175,-2.4,10.4849242404918));
#23556=CARTESIAN_POINT('',(-1.70992424049175,-2.7,10.4849242404918));
#23557=CARTESIAN_POINT('Origin',(-1.48492424049175,-2.4,10.4849242404918));
#23558=CARTESIAN_POINT('Origin',(1.48492424049175,-2.7,10.4849242404918));
#23559=CARTESIAN_POINT('',(1.25992424049175,-2.6,10.4849242404918));
#23560=CARTESIAN_POINT('Origin',(1.48492424049175,-2.6,10.4849242404918));
#23561=CARTESIAN_POINT('',(1.25992424049175,-2.4,10.4849242404918));
#23562=CARTESIAN_POINT('',(1.25992424049175,-2.7,10.4849242404918));
#23563=CARTESIAN_POINT('Origin',(1.48492424049175,-2.4,10.4849242404918));
#23564=CARTESIAN_POINT('Origin',(1.48492424049175,-2.7,7.51507575950825));
#23565=CARTESIAN_POINT('',(1.25992424049175,-2.6,7.51507575950825));
#23566=CARTESIAN_POINT('Origin',(1.48492424049175,-2.6,7.51507575950825));
#23567=CARTESIAN_POINT('',(1.25992424049175,-2.4,7.51507575950825));
#23568=CARTESIAN_POINT('',(1.25992424049175,-2.7,7.51507575950825));
#23569=CARTESIAN_POINT('Origin',(1.48492424049175,-2.4,7.51507575950825));
#23570=CARTESIAN_POINT('Origin',(0.,-2.4,9.));
#23571=CARTESIAN_POINT('',(-1.59,-2.,9.));
#23572=CARTESIAN_POINT('Origin',(0.,-2.,9.));
#23573=CARTESIAN_POINT('',(-1.59,-2.4,9.));
#23574=CARTESIAN_POINT('',(-1.59,-2.4,9.));
#23575=CARTESIAN_POINT('Origin',(0.,-2.4,9.));
#23576=CARTESIAN_POINT('Origin',(0.,-2.,9.));
#23577=CARTESIAN_POINT('',(-1.2,-2.,9.));
#23578=CARTESIAN_POINT('Origin',(0.,-2.,9.));
#23579=CARTESIAN_POINT('Origin',(0.,-2.6,9.));
#23580=CARTESIAN_POINT('',(-1.2,-2.6,9.));
#23581=CARTESIAN_POINT('',(-1.2,-2.6,9.));
#23582=CARTESIAN_POINT('Origin',(0.,-2.6,9.));
#23583=CARTESIAN_POINT('Origin',(0.,-2.6,9.));
#23584=CARTESIAN_POINT('',(-2.5,-2.4,9.));
#23585=CARTESIAN_POINT('Origin',(0.,-2.4,9.));
#23586=CARTESIAN_POINT('',(-2.5,-2.6,9.));
#23587=CARTESIAN_POINT('',(-2.5,-2.6,9.));
#23588=CARTESIAN_POINT('Origin',(0.,-2.6,9.));
#23589=CARTESIAN_POINT('Origin',(0.,-2.4,9.));
#23590=CARTESIAN_POINT('Origin',(0.,-2.6,9.));
#23591=CARTESIAN_POINT('',(0.,0.,0.));
#23592=CARTESIAN_POINT('Origin',(-1.48492424049175,-0.7,7.51507575950825));
#23593=CARTESIAN_POINT('',(-1.70992424049175,-0.6,7.51507575950825));
#23594=CARTESIAN_POINT('Origin',(-1.48492424049175,-0.6,7.51507575950825));
#23595=CARTESIAN_POINT('',(-1.70992424049175,-0.4,7.51507575950825));
#23596=CARTESIAN_POINT('',(-1.70992424049175,-0.7,7.51507575950825));
#23597=CARTESIAN_POINT('Origin',(-1.48492424049175,-0.4,7.51507575950825));
#23598=CARTESIAN_POINT('Origin',(-1.48492424049175,-0.7,10.4849242404918));
#23599=CARTESIAN_POINT('',(-1.70992424049175,-0.6,10.4849242404918));
#23600=CARTESIAN_POINT('Origin',(-1.48492424049175,-0.6,10.4849242404918));
#23601=CARTESIAN_POINT('',(-1.70992424049175,-0.4,10.4849242404918));
#23602=CARTESIAN_POINT('',(-1.70992424049175,-0.7,10.4849242404918));
#23603=CARTESIAN_POINT('Origin',(-1.48492424049175,-0.4,10.4849242404918));
#23604=CARTESIAN_POINT('Origin',(1.48492424049175,-0.7,10.4849242404918));
#23605=CARTESIAN_POINT('',(1.25992424049175,-0.6,10.4849242404918));
#23606=CARTESIAN_POINT('Origin',(1.48492424049175,-0.6,10.4849242404918));
#23607=CARTESIAN_POINT('',(1.25992424049175,-0.4,10.4849242404918));
#23608=CARTESIAN_POINT('',(1.25992424049175,-0.7,10.4849242404918));
#23609=CARTESIAN_POINT('Origin',(1.48492424049175,-0.4,10.4849242404918));
#23610=CARTESIAN_POINT('Origin',(1.48492424049175,-0.7,7.51507575950825));
#23611=CARTESIAN_POINT('',(1.25992424049175,-0.6,7.51507575950825));
#23612=CARTESIAN_POINT('Origin',(1.48492424049175,-0.6,7.51507575950825));
#23613=CARTESIAN_POINT('',(1.25992424049175,-0.4,7.51507575950825));
#23614=CARTESIAN_POINT('',(1.25992424049175,-0.7,7.51507575950825));
#23615=CARTESIAN_POINT('Origin',(1.48492424049175,-0.4,7.51507575950825));
#23616=CARTESIAN_POINT('Origin',(0.,-1.,9.));
#23617=CARTESIAN_POINT('',(-1.59,-0.6,9.));
#23618=CARTESIAN_POINT('Origin',(0.,-0.6,9.));
#23619=CARTESIAN_POINT('',(-1.59,-1.,9.));
#23620=CARTESIAN_POINT('',(-1.59,-1.,9.));
#23621=CARTESIAN_POINT('Origin',(0.,-1.,9.));
#23622=CARTESIAN_POINT('Origin',(0.,-1.,9.));
#23623=CARTESIAN_POINT('',(-1.2,-1.,9.));
#23624=CARTESIAN_POINT('Origin',(0.,-1.,9.));
#23625=CARTESIAN_POINT('Origin',(0.,-0.6,9.));
#23626=CARTESIAN_POINT('',(-1.2,-0.4,9.));
#23627=CARTESIAN_POINT('Origin',(0.,-0.4,9.));
#23628=CARTESIAN_POINT('',(-1.2,-0.6,9.));
#23629=CARTESIAN_POINT('Origin',(0.,-0.6,9.));
#23630=CARTESIAN_POINT('',(-2.5,-0.4,9.));
#23631=CARTESIAN_POINT('Origin',(0.,-0.4,9.));
#23632=CARTESIAN_POINT('',(-2.5,-0.6,9.));
#23633=CARTESIAN_POINT('',(-2.5,-0.6,9.));
#23634=CARTESIAN_POINT('Origin',(0.,-0.6,9.));
#23635=CARTESIAN_POINT('Origin',(0.,-0.4,9.));
#23636=CARTESIAN_POINT('Origin',(0.,-0.6,9.));
#23637=CARTESIAN_POINT('',(0.,0.,0.));
#23638=CARTESIAN_POINT('Origin',(4.16152236891498,-2.7,7.16152236891498));
#23639=CARTESIAN_POINT('',(3.93652236891498,-2.6,7.16152236891498));
#23640=CARTESIAN_POINT('Origin',(4.16152236891498,-2.6,7.16152236891498));
#23641=CARTESIAN_POINT('',(3.93652236891498,-2.4,7.16152236891498));
#23642=CARTESIAN_POINT('',(3.93652236891498,-2.7,7.16152236891498));
#23643=CARTESIAN_POINT('Origin',(4.16152236891498,-2.4,7.16152236891498));
#23644=CARTESIAN_POINT('Origin',(4.16152236891498,-2.7,10.838477631085));
#23645=CARTESIAN_POINT('',(3.93652236891498,-2.6,10.838477631085));
#23646=CARTESIAN_POINT('Origin',(4.16152236891498,-2.6,10.838477631085));
#23647=CARTESIAN_POINT('',(3.93652236891498,-2.4,10.838477631085));
#23648=CARTESIAN_POINT('',(3.93652236891498,-2.7,10.838477631085));
#23649=CARTESIAN_POINT('Origin',(4.16152236891498,-2.4,10.838477631085));
#23650=CARTESIAN_POINT('Origin',(7.83847763108502,-2.7,10.838477631085));
#23651=CARTESIAN_POINT('',(7.61347763108502,-2.6,10.838477631085));
#23652=CARTESIAN_POINT('Origin',(7.83847763108502,-2.6,10.838477631085));
#23653=CARTESIAN_POINT('',(7.61347763108502,-2.4,10.838477631085));
#23654=CARTESIAN_POINT('',(7.61347763108502,-2.7,10.838477631085));
#23655=CARTESIAN_POINT('Origin',(7.83847763108502,-2.4,10.838477631085));
#23656=CARTESIAN_POINT('Origin',(7.83847763108502,-2.7,7.16152236891498));
#23657=CARTESIAN_POINT('',(7.61347763108502,-2.6,7.16152236891498));
#23658=CARTESIAN_POINT('Origin',(7.83847763108502,-2.6,7.16152236891498));
#23659=CARTESIAN_POINT('',(7.61347763108502,-2.4,7.16152236891498));
#23660=CARTESIAN_POINT('',(7.61347763108502,-2.7,7.16152236891498));
#23661=CARTESIAN_POINT('Origin',(7.83847763108502,-2.4,7.16152236891498));
#23662=CARTESIAN_POINT('Origin',(6.,-2.4,9.));
#23663=CARTESIAN_POINT('',(3.66,-2.2,9.));
#23664=CARTESIAN_POINT('Origin',(6.,-2.2,9.));
#23665=CARTESIAN_POINT('',(3.66,-2.4,9.));
#23666=CARTESIAN_POINT('',(3.66,-2.4,9.));
#23667=CARTESIAN_POINT('Origin',(6.,-2.4,9.));
#23668=CARTESIAN_POINT('Origin',(6.,-2.2,9.));
#23669=CARTESIAN_POINT('',(4.1,-2.2,9.));
#23670=CARTESIAN_POINT('Origin',(6.,-2.2,9.));
#23671=CARTESIAN_POINT('Origin',(6.,-2.6,9.));
#23672=CARTESIAN_POINT('',(4.1,-2.6,9.));
#23673=CARTESIAN_POINT('',(4.1,-2.6,9.));
#23674=CARTESIAN_POINT('Origin',(6.,-2.6,9.));
#23675=CARTESIAN_POINT('Origin',(6.,-2.6,9.));
#23676=CARTESIAN_POINT('',(3.,-2.4,9.));
#23677=CARTESIAN_POINT('Origin',(6.,-2.4,9.));
#23678=CARTESIAN_POINT('',(3.,-2.6,9.));
#23679=CARTESIAN_POINT('',(3.,-2.6,9.));
#23680=CARTESIAN_POINT('Origin',(6.,-2.6,9.));
#23681=CARTESIAN_POINT('Origin',(6.,-2.4,9.));
#23682=CARTESIAN_POINT('Origin',(6.,-2.6,9.));
#23683=CARTESIAN_POINT('',(0.,0.,0.));
#23684=CARTESIAN_POINT('Origin',(4.16152236891498,-0.7,7.16152236891498));
#23685=CARTESIAN_POINT('',(3.93652236891498,-0.6,7.16152236891498));
#23686=CARTESIAN_POINT('Origin',(4.16152236891498,-0.6,7.16152236891498));
#23687=CARTESIAN_POINT('',(3.93652236891498,-0.4,7.16152236891498));
#23688=CARTESIAN_POINT('',(3.93652236891498,-0.7,7.16152236891498));
#23689=CARTESIAN_POINT('Origin',(4.16152236891498,-0.4,7.16152236891498));
#23690=CARTESIAN_POINT('Origin',(4.16152236891498,-0.7,10.838477631085));
#23691=CARTESIAN_POINT('',(3.93652236891498,-0.6,10.838477631085));
#23692=CARTESIAN_POINT('Origin',(4.16152236891498,-0.6,10.838477631085));
#23693=CARTESIAN_POINT('',(3.93652236891498,-0.4,10.838477631085));
#23694=CARTESIAN_POINT('',(3.93652236891498,-0.7,10.838477631085));
#23695=CARTESIAN_POINT('Origin',(4.16152236891498,-0.4,10.838477631085));
#23696=CARTESIAN_POINT('Origin',(7.83847763108502,-0.7,10.838477631085));
#23697=CARTESIAN_POINT('',(7.61347763108502,-0.6,10.838477631085));
#23698=CARTESIAN_POINT('Origin',(7.83847763108502,-0.6,10.838477631085));
#23699=CARTESIAN_POINT('',(7.61347763108502,-0.4,10.838477631085));
#23700=CARTESIAN_POINT('',(7.61347763108502,-0.7,10.838477631085));
#23701=CARTESIAN_POINT('Origin',(7.83847763108502,-0.4,10.838477631085));
#23702=CARTESIAN_POINT('Origin',(7.83847763108502,-0.7,7.16152236891498));
#23703=CARTESIAN_POINT('',(7.61347763108502,-0.6,7.16152236891498));
#23704=CARTESIAN_POINT('Origin',(7.83847763108502,-0.6,7.16152236891498));
#23705=CARTESIAN_POINT('',(7.61347763108502,-0.4,7.16152236891498));
#23706=CARTESIAN_POINT('',(7.61347763108502,-0.7,7.16152236891498));
#23707=CARTESIAN_POINT('Origin',(7.83847763108502,-0.4,7.16152236891498));
#23708=CARTESIAN_POINT('Origin',(6.,-0.8,9.));
#23709=CARTESIAN_POINT('',(3.66,-0.6,9.));
#23710=CARTESIAN_POINT('Origin',(6.,-0.6,9.));
#23711=CARTESIAN_POINT('',(3.66,-0.8,9.));
#23712=CARTESIAN_POINT('',(3.66,-0.8,9.));
#23713=CARTESIAN_POINT('Origin',(6.,-0.8,9.));
#23714=CARTESIAN_POINT('Origin',(6.,-0.8,9.));
#23715=CARTESIAN_POINT('',(4.1,-0.8,9.));
#23716=CARTESIAN_POINT('Origin',(6.,-0.8,9.));
#23717=CARTESIAN_POINT('Origin',(6.,-0.6,9.));
#23718=CARTESIAN_POINT('',(4.1,-0.4,9.));
#23719=CARTESIAN_POINT('Origin',(6.,-0.4,9.));
#23720=CARTESIAN_POINT('',(4.1,-0.6,9.));
#23721=CARTESIAN_POINT('Origin',(6.,-0.6,9.));
#23722=CARTESIAN_POINT('',(3.,-0.4,9.));
#23723=CARTESIAN_POINT('Origin',(6.,-0.4,9.));
#23724=CARTESIAN_POINT('',(3.,-0.6,9.));
#23725=CARTESIAN_POINT('',(3.,-0.6,9.));
#23726=CARTESIAN_POINT('Origin',(6.,-0.6,9.));
#23727=CARTESIAN_POINT('Origin',(6.,-0.4,9.));
#23728=CARTESIAN_POINT('Origin',(6.,-0.6,9.));
#23729=CARTESIAN_POINT('',(0.,0.,0.));
#23730=CARTESIAN_POINT('Origin',(0.144337567297406,-0.6,-0.25));
#23731=CARTESIAN_POINT('',(0.288675134594813,-0.6,0.));
#23732=CARTESIAN_POINT('',(0.144337567297406,-0.6,-0.25));
#23733=CARTESIAN_POINT('',(0.288675134594813,-0.6,0.));
#23734=CARTESIAN_POINT('',(0.144337567297406,-0.96,-0.25));
#23735=CARTESIAN_POINT('',(0.144337567297406,-0.6,-0.25));
#23736=CARTESIAN_POINT('',(0.288675134594813,-0.96,0.));
#23737=CARTESIAN_POINT('',(0.288675134594813,-0.96,0.));
#23738=CARTESIAN_POINT('',(0.288675134594813,-0.6,0.));
#23739=CARTESIAN_POINT('Origin',(-0.144337567297406,-0.6,-0.25));
#23740=CARTESIAN_POINT('',(-0.144337567297406,-0.6,-0.25));
#23741=CARTESIAN_POINT('',(0.144337567297406,-0.6,-0.25));
#23742=CARTESIAN_POINT('',(-0.144337567297406,-0.96,-0.25));
#23743=CARTESIAN_POINT('',(-0.144337567297406,-0.6,-0.25));
#23744=CARTESIAN_POINT('',(0.144337567297406,-0.96,-0.25));
#23745=CARTESIAN_POINT('Origin',(-0.288675134594813,-0.6,-8.32667268468867E-17));
#23746=CARTESIAN_POINT('',(-0.288675134594813,-0.6,-3.53525079574969E-17));
#23747=CARTESIAN_POINT('',(-0.144337567297406,-0.6,-0.25));
#23748=CARTESIAN_POINT('',(-0.288675134594813,-0.96,-5.55111512312578E-17));
#23749=CARTESIAN_POINT('',(-0.288675134594813,-0.6,-3.53525079574969E-17));
#23750=CARTESIAN_POINT('',(-0.144337567297406,-0.96,-0.25));
#23751=CARTESIAN_POINT('Origin',(-0.144337567297407,-0.6,0.25));
#23752=CARTESIAN_POINT('',(-0.144337567297407,-0.6,0.25));
#23753=CARTESIAN_POINT('',(-0.288675134594813,-0.6,-3.53525079574969E-17));
#23754=CARTESIAN_POINT('',(-0.144337567297407,-0.96,0.25));
#23755=CARTESIAN_POINT('',(-0.144337567297407,-0.6,0.25));
#23756=CARTESIAN_POINT('',(-0.288675134594813,-0.96,-3.53525079574969E-17));
#23757=CARTESIAN_POINT('Origin',(0.144337567297406,-0.6,0.25));
#23758=CARTESIAN_POINT('',(0.144337567297406,-0.6,0.25));
#23759=CARTESIAN_POINT('',(-0.144337567297407,-0.6,0.25));
#23760=CARTESIAN_POINT('',(0.144337567297406,-0.96,0.25));
#23761=CARTESIAN_POINT('',(0.144337567297406,-0.6,0.25));
#23762=CARTESIAN_POINT('',(-0.144337567297407,-0.96,0.25));
#23763=CARTESIAN_POINT('Origin',(0.288675134594813,-0.6,0.));
#23764=CARTESIAN_POINT('',(0.144337567297406,-0.6,0.25));
#23765=CARTESIAN_POINT('',(0.144337567297406,-0.96,0.25));
#23766=CARTESIAN_POINT('Origin',(0.,-0.6,0.));
#23767=CARTESIAN_POINT('Origin',(0.,-0.96,0.));
#23768=CARTESIAN_POINT('Origin',(0.,-1.8,0.));
#23769=CARTESIAN_POINT('',(-0.2942,-1.8,3.60291088309151E-17));
#23770=CARTESIAN_POINT('Origin',(0.,-1.8,0.));
#23771=CARTESIAN_POINT('Origin',(0.45,0.6,0.));
#23772=CARTESIAN_POINT('',(-0.45,0.6,-5.51091059616309E-17));
#23773=CARTESIAN_POINT('Origin',(0.,0.6,0.));
#23774=CARTESIAN_POINT('Origin',(0.,0.575,0.));
#23775=CARTESIAN_POINT('',(-0.5,0.55,-6.12323399573677E-17));
#23776=CARTESIAN_POINT('Origin',(0.,0.55,0.));
#23777=CARTESIAN_POINT('',(-0.475,0.575,-5.81707229594993E-17));
#23778=CARTESIAN_POINT('Origin',(0.,0.29,0.));
#23779=CARTESIAN_POINT('',(-0.5,0.0299999999999998,-6.12323399573677E-17));
#23780=CARTESIAN_POINT('Origin',(0.,0.0299999999999998,0.));
#23781=CARTESIAN_POINT('',(-0.5,0.29,-6.12323399573677E-17));
#23782=CARTESIAN_POINT('Origin',(0.,0.0150000000000001,0.));
#23783=CARTESIAN_POINT('',(-0.47,7.11236625150491E-17,-5.75583995599256E-17));
#23784=CARTESIAN_POINT('Origin',(0.,0.,0.));
#23785=CARTESIAN_POINT('',(-0.485,0.0150000000000001,-5.93953697586466E-17));
#23786=CARTESIAN_POINT('Origin',(0.32,0.,0.));
#23787=CARTESIAN_POINT('',(-0.32,-6.93889390390723E-18,-3.91886975727153E-17));
#23788=CARTESIAN_POINT('Origin',(0.,0.,0.));
#23789=CARTESIAN_POINT('Origin',(0.,-0.02,0.));
#23790=CARTESIAN_POINT('',(-0.2942,-0.0515999999999999,3.60291088309151E-17));
#23791=CARTESIAN_POINT('Origin',(0.,-0.0515999999999999,0.));
#23792=CARTESIAN_POINT('',(-0.31,-0.02,-3.7964050773568E-17));
#23793=CARTESIAN_POINT('Origin',(0.,-1.24,0.));
#23794=CARTESIAN_POINT('',(-0.2942,-1.24,-3.60291088309151E-17));
#23795=CARTESIAN_POINT('',(0.,0.,0.));
#23796=CARTESIAN_POINT('Origin',(10.5150757595082,-2.7,7.51507575950825));
#23797=CARTESIAN_POINT('',(10.2900757595082,-2.6,7.51507575950825));
#23798=CARTESIAN_POINT('Origin',(10.5150757595082,-2.6,7.51507575950825));
#23799=CARTESIAN_POINT('',(10.2900757595082,-2.4,7.51507575950825));
#23800=CARTESIAN_POINT('',(10.2900757595082,-2.7,7.51507575950825));
#23801=CARTESIAN_POINT('Origin',(10.5150757595082,-2.4,7.51507575950825));
#23802=CARTESIAN_POINT('Origin',(10.5150757595082,-2.7,10.4849242404918));
#23803=CARTESIAN_POINT('',(10.2900757595082,-2.6,10.4849242404918));
#23804=CARTESIAN_POINT('Origin',(10.5150757595082,-2.6,10.4849242404918));
#23805=CARTESIAN_POINT('',(10.2900757595082,-2.4,10.4849242404918));
#23806=CARTESIAN_POINT('',(10.2900757595082,-2.7,10.4849242404918));
#23807=CARTESIAN_POINT('Origin',(10.5150757595082,-2.4,10.4849242404918));
#23808=CARTESIAN_POINT('Origin',(13.4849242404918,-2.7,10.4849242404918));
#23809=CARTESIAN_POINT('',(13.2599242404918,-2.6,10.4849242404918));
#23810=CARTESIAN_POINT('Origin',(13.4849242404918,-2.6,10.4849242404918));
#23811=CARTESIAN_POINT('',(13.2599242404918,-2.4,10.4849242404918));
#23812=CARTESIAN_POINT('',(13.2599242404918,-2.7,10.4849242404918));
#23813=CARTESIAN_POINT('Origin',(13.4849242404918,-2.4,10.4849242404918));
#23814=CARTESIAN_POINT('Origin',(13.4849242404918,-2.7,7.51507575950825));
#23815=CARTESIAN_POINT('',(13.2599242404918,-2.6,7.51507575950825));
#23816=CARTESIAN_POINT('Origin',(13.4849242404918,-2.6,7.51507575950825));
#23817=CARTESIAN_POINT('',(13.2599242404918,-2.4,7.51507575950825));
#23818=CARTESIAN_POINT('',(13.2599242404918,-2.7,7.51507575950825));
#23819=CARTESIAN_POINT('Origin',(13.4849242404918,-2.4,7.51507575950825));
#23820=CARTESIAN_POINT('Origin',(12.,-2.4,9.));
#23821=CARTESIAN_POINT('',(10.41,-2.,9.));
#23822=CARTESIAN_POINT('Origin',(12.,-2.,9.));
#23823=CARTESIAN_POINT('',(10.41,-2.4,9.));
#23824=CARTESIAN_POINT('',(10.41,-2.4,9.));
#23825=CARTESIAN_POINT('Origin',(12.,-2.4,9.));
#23826=CARTESIAN_POINT('Origin',(12.,-2.,9.));
#23827=CARTESIAN_POINT('',(10.8,-2.,9.));
#23828=CARTESIAN_POINT('Origin',(12.,-2.,9.));
#23829=CARTESIAN_POINT('Origin',(12.,-2.6,9.));
#23830=CARTESIAN_POINT('',(10.8,-2.6,9.));
#23831=CARTESIAN_POINT('',(10.8,-2.6,9.));
#23832=CARTESIAN_POINT('Origin',(12.,-2.6,9.));
#23833=CARTESIAN_POINT('Origin',(12.,-2.6,9.));
#23834=CARTESIAN_POINT('',(9.5,-2.4,9.));
#23835=CARTESIAN_POINT('Origin',(12.,-2.4,9.));
#23836=CARTESIAN_POINT('',(9.5,-2.6,9.));
#23837=CARTESIAN_POINT('',(9.5,-2.6,9.));
#23838=CARTESIAN_POINT('Origin',(12.,-2.6,9.));
#23839=CARTESIAN_POINT('Origin',(12.,-2.4,9.));
#23840=CARTESIAN_POINT('Origin',(12.,-2.6,9.));
#23841=CARTESIAN_POINT('',(0.,0.,0.));
#23842=CARTESIAN_POINT('Origin',(10.5150757595082,-0.7,7.51507575950825));
#23843=CARTESIAN_POINT('',(10.2900757595082,-0.6,7.51507575950825));
#23844=CARTESIAN_POINT('Origin',(10.5150757595082,-0.6,7.51507575950825));
#23845=CARTESIAN_POINT('',(10.2900757595082,-0.4,7.51507575950825));
#23846=CARTESIAN_POINT('',(10.2900757595082,-0.7,7.51507575950825));
#23847=CARTESIAN_POINT('Origin',(10.5150757595082,-0.4,7.51507575950825));
#23848=CARTESIAN_POINT('Origin',(10.5150757595082,-0.7,10.4849242404918));
#23849=CARTESIAN_POINT('',(10.2900757595082,-0.6,10.4849242404918));
#23850=CARTESIAN_POINT('Origin',(10.5150757595082,-0.6,10.4849242404918));
#23851=CARTESIAN_POINT('',(10.2900757595082,-0.4,10.4849242404918));
#23852=CARTESIAN_POINT('',(10.2900757595082,-0.7,10.4849242404918));
#23853=CARTESIAN_POINT('Origin',(10.5150757595082,-0.4,10.4849242404918));
#23854=CARTESIAN_POINT('Origin',(13.4849242404918,-0.7,10.4849242404918));
#23855=CARTESIAN_POINT('',(13.2599242404918,-0.6,10.4849242404918));
#23856=CARTESIAN_POINT('Origin',(13.4849242404918,-0.6,10.4849242404918));
#23857=CARTESIAN_POINT('',(13.2599242404918,-0.4,10.4849242404918));
#23858=CARTESIAN_POINT('',(13.2599242404918,-0.7,10.4849242404918));
#23859=CARTESIAN_POINT('Origin',(13.4849242404918,-0.4,10.4849242404918));
#23860=CARTESIAN_POINT('Origin',(13.4849242404918,-0.7,7.51507575950825));
#23861=CARTESIAN_POINT('',(13.2599242404918,-0.6,7.51507575950825));
#23862=CARTESIAN_POINT('Origin',(13.4849242404918,-0.6,7.51507575950825));
#23863=CARTESIAN_POINT('',(13.2599242404918,-0.4,7.51507575950825));
#23864=CARTESIAN_POINT('',(13.2599242404918,-0.7,7.51507575950825));
#23865=CARTESIAN_POINT('Origin',(13.4849242404918,-0.4,7.51507575950825));
#23866=CARTESIAN_POINT('Origin',(12.,-1.,9.));
#23867=CARTESIAN_POINT('',(10.41,-0.6,9.));
#23868=CARTESIAN_POINT('Origin',(12.,-0.6,9.));
#23869=CARTESIAN_POINT('',(10.41,-1.,9.));
#23870=CARTESIAN_POINT('',(10.41,-1.,9.));
#23871=CARTESIAN_POINT('Origin',(12.,-1.,9.));
#23872=CARTESIAN_POINT('Origin',(12.,-1.,9.));
#23873=CARTESIAN_POINT('',(10.8,-1.,9.));
#23874=CARTESIAN_POINT('Origin',(12.,-1.,9.));
#23875=CARTESIAN_POINT('Origin',(12.,-0.6,9.));
#23876=CARTESIAN_POINT('',(10.8,-0.4,9.));
#23877=CARTESIAN_POINT('Origin',(12.,-0.4,9.));
#23878=CARTESIAN_POINT('',(10.8,-0.6,9.));
#23879=CARTESIAN_POINT('Origin',(12.,-0.6,9.));
#23880=CARTESIAN_POINT('',(9.5,-0.4,9.));
#23881=CARTESIAN_POINT('Origin',(12.,-0.4,9.));
#23882=CARTESIAN_POINT('',(9.5,-0.6,9.));
#23883=CARTESIAN_POINT('',(9.5,-0.6,9.));
#23884=CARTESIAN_POINT('Origin',(12.,-0.6,9.));
#23885=CARTESIAN_POINT('Origin',(12.,-0.4,9.));
#23886=CARTESIAN_POINT('Origin',(12.,-0.6,9.));
#23887=CARTESIAN_POINT('',(0.,0.,0.));
#23888=CARTESIAN_POINT('Origin',(16.161522368915,-2.7,7.16152236891498));
#23889=CARTESIAN_POINT('',(15.936522368915,-2.6,7.16152236891498));
#23890=CARTESIAN_POINT('Origin',(16.161522368915,-2.6,7.16152236891498));
#23891=CARTESIAN_POINT('',(15.936522368915,-2.4,7.16152236891498));
#23892=CARTESIAN_POINT('',(15.936522368915,-2.7,7.16152236891498));
#23893=CARTESIAN_POINT('Origin',(16.161522368915,-2.4,7.16152236891498));
#23894=CARTESIAN_POINT('Origin',(16.161522368915,-2.7,10.838477631085));
#23895=CARTESIAN_POINT('',(15.936522368915,-2.6,10.838477631085));
#23896=CARTESIAN_POINT('Origin',(16.161522368915,-2.6,10.838477631085));
#23897=CARTESIAN_POINT('',(15.936522368915,-2.4,10.838477631085));
#23898=CARTESIAN_POINT('',(15.936522368915,-2.7,10.838477631085));
#23899=CARTESIAN_POINT('Origin',(16.161522368915,-2.4,10.838477631085));
#23900=CARTESIAN_POINT('Origin',(19.838477631085,-2.7,10.838477631085));
#23901=CARTESIAN_POINT('',(19.613477631085,-2.6,10.838477631085));
#23902=CARTESIAN_POINT('Origin',(19.838477631085,-2.6,10.838477631085));
#23903=CARTESIAN_POINT('',(19.613477631085,-2.4,10.838477631085));
#23904=CARTESIAN_POINT('',(19.613477631085,-2.7,10.838477631085));
#23905=CARTESIAN_POINT('Origin',(19.838477631085,-2.4,10.838477631085));
#23906=CARTESIAN_POINT('Origin',(19.838477631085,-2.7,7.16152236891498));
#23907=CARTESIAN_POINT('',(19.613477631085,-2.6,7.16152236891498));
#23908=CARTESIAN_POINT('Origin',(19.838477631085,-2.6,7.16152236891498));
#23909=CARTESIAN_POINT('',(19.613477631085,-2.4,7.16152236891498));
#23910=CARTESIAN_POINT('',(19.613477631085,-2.7,7.16152236891498));
#23911=CARTESIAN_POINT('Origin',(19.838477631085,-2.4,7.16152236891498));
#23912=CARTESIAN_POINT('Origin',(18.,-2.4,9.));
#23913=CARTESIAN_POINT('',(15.66,-2.2,9.));
#23914=CARTESIAN_POINT('Origin',(18.,-2.2,9.));
#23915=CARTESIAN_POINT('',(15.66,-2.4,9.));
#23916=CARTESIAN_POINT('',(15.66,-2.4,9.));
#23917=CARTESIAN_POINT('Origin',(18.,-2.4,9.));
#23918=CARTESIAN_POINT('Origin',(18.,-2.2,9.));
#23919=CARTESIAN_POINT('',(16.1,-2.2,9.));
#23920=CARTESIAN_POINT('Origin',(18.,-2.2,9.));
#23921=CARTESIAN_POINT('Origin',(18.,-2.6,9.));
#23922=CARTESIAN_POINT('',(16.1,-2.6,9.));
#23923=CARTESIAN_POINT('',(16.1,-2.6,9.));
#23924=CARTESIAN_POINT('Origin',(18.,-2.6,9.));
#23925=CARTESIAN_POINT('Origin',(18.,-2.6,9.));
#23926=CARTESIAN_POINT('',(15.,-2.4,9.));
#23927=CARTESIAN_POINT('Origin',(18.,-2.4,9.));
#23928=CARTESIAN_POINT('',(15.,-2.6,9.));
#23929=CARTESIAN_POINT('',(15.,-2.6,9.));
#23930=CARTESIAN_POINT('Origin',(18.,-2.6,9.));
#23931=CARTESIAN_POINT('Origin',(18.,-2.4,9.));
#23932=CARTESIAN_POINT('Origin',(18.,-2.6,9.));
#23933=CARTESIAN_POINT('',(0.,0.,0.));
#23934=CARTESIAN_POINT('Origin',(16.161522368915,-0.7,7.16152236891498));
#23935=CARTESIAN_POINT('',(15.936522368915,-0.6,7.16152236891498));
#23936=CARTESIAN_POINT('Origin',(16.161522368915,-0.6,7.16152236891498));
#23937=CARTESIAN_POINT('',(15.936522368915,-0.4,7.16152236891498));
#23938=CARTESIAN_POINT('',(15.936522368915,-0.7,7.16152236891498));
#23939=CARTESIAN_POINT('Origin',(16.161522368915,-0.4,7.16152236891498));
#23940=CARTESIAN_POINT('Origin',(16.161522368915,-0.7,10.838477631085));
#23941=CARTESIAN_POINT('',(15.936522368915,-0.6,10.838477631085));
#23942=CARTESIAN_POINT('Origin',(16.161522368915,-0.6,10.838477631085));
#23943=CARTESIAN_POINT('',(15.936522368915,-0.4,10.838477631085));
#23944=CARTESIAN_POINT('',(15.936522368915,-0.7,10.838477631085));
#23945=CARTESIAN_POINT('Origin',(16.161522368915,-0.4,10.838477631085));
#23946=CARTESIAN_POINT('Origin',(19.838477631085,-0.7,10.838477631085));
#23947=CARTESIAN_POINT('',(19.613477631085,-0.6,10.838477631085));
#23948=CARTESIAN_POINT('Origin',(19.838477631085,-0.6,10.838477631085));
#23949=CARTESIAN_POINT('',(19.613477631085,-0.4,10.838477631085));
#23950=CARTESIAN_POINT('',(19.613477631085,-0.7,10.838477631085));
#23951=CARTESIAN_POINT('Origin',(19.838477631085,-0.4,10.838477631085));
#23952=CARTESIAN_POINT('Origin',(19.838477631085,-0.7,7.16152236891498));
#23953=CARTESIAN_POINT('',(19.613477631085,-0.6,7.16152236891498));
#23954=CARTESIAN_POINT('Origin',(19.838477631085,-0.6,7.16152236891498));
#23955=CARTESIAN_POINT('',(19.613477631085,-0.4,7.16152236891498));
#23956=CARTESIAN_POINT('',(19.613477631085,-0.7,7.16152236891498));
#23957=CARTESIAN_POINT('Origin',(19.838477631085,-0.4,7.16152236891498));
#23958=CARTESIAN_POINT('Origin',(18.,-0.8,9.));
#23959=CARTESIAN_POINT('',(15.66,-0.6,9.));
#23960=CARTESIAN_POINT('Origin',(18.,-0.6,9.));
#23961=CARTESIAN_POINT('',(15.66,-0.8,9.));
#23962=CARTESIAN_POINT('',(15.66,-0.8,9.));
#23963=CARTESIAN_POINT('Origin',(18.,-0.8,9.));
#23964=CARTESIAN_POINT('Origin',(18.,-0.8,9.));
#23965=CARTESIAN_POINT('',(16.1,-0.8,9.));
#23966=CARTESIAN_POINT('Origin',(18.,-0.8,9.));
#23967=CARTESIAN_POINT('Origin',(18.,-0.6,9.));
#23968=CARTESIAN_POINT('',(16.1,-0.4,9.));
#23969=CARTESIAN_POINT('Origin',(18.,-0.4,9.));
#23970=CARTESIAN_POINT('',(16.1,-0.6,9.));
#23971=CARTESIAN_POINT('Origin',(18.,-0.6,9.));
#23972=CARTESIAN_POINT('',(15.,-0.4,9.));
#23973=CARTESIAN_POINT('Origin',(18.,-0.4,9.));
#23974=CARTESIAN_POINT('',(15.,-0.6,9.));
#23975=CARTESIAN_POINT('',(15.,-0.6,9.));
#23976=CARTESIAN_POINT('Origin',(18.,-0.6,9.));
#23977=CARTESIAN_POINT('Origin',(18.,-0.4,9.));
#23978=CARTESIAN_POINT('Origin',(18.,-0.6,9.));
#23979=CARTESIAN_POINT('',(0.,0.,0.));
#23980=CARTESIAN_POINT('',(0.,0.,0.));
#23981=CARTESIAN_POINT('Origin',(0.,0.,0.));
#23982=CARTESIAN_POINT('',(-1.070235,-0.308121667383195,-1.31065986708547E-16));
#23983=CARTESIAN_POINT('',(-1.31065986708547E-16,-0.308121667383195,1.070235));
#23984=CARTESIAN_POINT('Origin',(0.,-0.308121667383195,0.));
#23985=CARTESIAN_POINT('Origin',(0.,-0.308121667383195,0.));
#23986=CARTESIAN_POINT('',(-1.31065986708547E-16,0.308121667383195,1.070235));
#23987=CARTESIAN_POINT('Origin',(-1.34711147906209E-16,0.,1.1));
#23988=CARTESIAN_POINT('',(-1.070235,0.308121667383195,1.31065986708547E-16));
#23989=CARTESIAN_POINT('Origin',(0.,0.308121667383195,0.));
#23990=CARTESIAN_POINT('Origin',(0.,0.308121667383195,0.));
#23991=CARTESIAN_POINT('Origin',(0.,0.,0.));
#23992=CARTESIAN_POINT('',(-1.070235,0.5,-1.31065986708547E-16));
#23993=CARTESIAN_POINT('',(-1.070235,0.,-1.31065986708547E-16));
#23994=CARTESIAN_POINT('Origin',(0.,0.5,0.));
#23995=CARTESIAN_POINT('Origin',(0.,0.,0.));
#23996=CARTESIAN_POINT('',(-0.6,-0.44,-7.34788079488412E-17));
#23997=CARTESIAN_POINT('Origin',(0.,-0.44,0.));
#23998=CARTESIAN_POINT('',(-0.6,0.44,-7.34788079488412E-17));
#23999=CARTESIAN_POINT('',(-0.6,0.,-7.34788079488412E-17));
#24000=CARTESIAN_POINT('Origin',(0.,0.44,0.));
#24001=CARTESIAN_POINT('Origin',(0.,0.47,0.));
#24002=CARTESIAN_POINT('',(-0.66,0.5,-8.08266887437253E-17));
#24003=CARTESIAN_POINT('',(-0.63,0.47,-7.71527483462832E-17));
#24004=CARTESIAN_POINT('Origin',(0.,0.5,0.));
#24005=CARTESIAN_POINT('Origin',(1.070235,0.5,0.));
#24006=CARTESIAN_POINT('Origin',(0.,0.,0.));
#24007=CARTESIAN_POINT('',(-1.070235,-0.5,-1.31065986708547E-16));
#24008=CARTESIAN_POINT('Origin',(0.,-0.5,0.));
#24009=CARTESIAN_POINT('',(-1.070235,0.,-1.31065986708547E-16));
#24010=CARTESIAN_POINT('Origin',(0.66,-0.5,0.));
#24011=CARTESIAN_POINT('',(-0.66,-0.5,-8.08266887437253E-17));
#24012=CARTESIAN_POINT('Origin',(0.,-0.5,0.));
#24013=CARTESIAN_POINT('Origin',(0.,-0.47,0.));
#24014=CARTESIAN_POINT('',(-0.63,-0.47,-7.71527483462832E-17));
#24015=CARTESIAN_POINT('',(0.,0.,0.));
#24016=CARTESIAN_POINT('Origin',(0.,0.,0.));
#24017=CARTESIAN_POINT('',(-1.129765,0.308121667383195,-1.38356309103871E-16));
#24018=CARTESIAN_POINT('',(-1.38356309103871E-16,0.308121667383195,1.129765));
#24019=CARTESIAN_POINT('Origin',(0.,0.308121667383195,0.));
#24020=CARTESIAN_POINT('Origin',(0.,0.308121667383195,0.));
#24021=CARTESIAN_POINT('',(-1.38356309103871E-16,-0.308121667383195,1.129765));
#24022=CARTESIAN_POINT('Origin',(-1.34711147906209E-16,0.,1.1));
#24023=CARTESIAN_POINT('',(-1.129765,-0.308121667383195,1.38356309103871E-16));
#24024=CARTESIAN_POINT('Origin',(0.,-0.308121667383195,0.));
#24025=CARTESIAN_POINT('Origin',(0.,-0.308121667383195,0.));
#24026=CARTESIAN_POINT('Origin',(0.,0.,0.));
#24027=CARTESIAN_POINT('',(-1.129765,-0.5,-1.38356309103871E-16));
#24028=CARTESIAN_POINT('Origin',(0.,-0.5,0.));
#24029=CARTESIAN_POINT('',(-1.129765,0.,-1.38356309103871E-16));
#24030=CARTESIAN_POINT('Origin',(1.54,0.5,0.));
#24031=CARTESIAN_POINT('',(-1.54,0.5,-1.88595607068692E-16));
#24032=CARTESIAN_POINT('Origin',(0.,0.5,0.));
#24033=CARTESIAN_POINT('',(-1.129765,0.5,-1.38356309103871E-16));
#24034=CARTESIAN_POINT('Origin',(0.,0.5,0.));
#24035=CARTESIAN_POINT('Origin',(0.,0.47,0.));
#24036=CARTESIAN_POINT('',(-1.6,0.44,-1.95943487863577E-16));
#24037=CARTESIAN_POINT('Origin',(0.,0.44,0.));
#24038=CARTESIAN_POINT('',(-1.57,0.47,-1.92269547466134E-16));
#24039=CARTESIAN_POINT('Origin',(0.,0.,0.));
#24040=CARTESIAN_POINT('',(-1.6,-0.44,-1.95943487863577E-16));
#24041=CARTESIAN_POINT('Origin',(0.,-0.44,0.));
#24042=CARTESIAN_POINT('',(-1.6,0.,-1.95943487863577E-16));
#24043=CARTESIAN_POINT('Origin',(0.,-0.47,0.));
#24044=CARTESIAN_POINT('',(-1.54,-0.5,-1.88595607068692E-16));
#24045=CARTESIAN_POINT('Origin',(0.,-0.5,0.));
#24046=CARTESIAN_POINT('',(-1.57,-0.47,-1.92269547466134E-16));
#24047=CARTESIAN_POINT('Origin',(1.129765,-0.5,0.));
#24048=CARTESIAN_POINT('Origin',(0.,0.,0.));
#24049=CARTESIAN_POINT('',(-1.129765,0.,-1.38356309103871E-16));
#24050=CARTESIAN_POINT('',(0.,0.,0.));
#24051=CARTESIAN_POINT('Origin',(1.1,0.,0.));
#24052=CARTESIAN_POINT('',(1.1,-2.23201749654651E-33,0.29765));
#24053=CARTESIAN_POINT('',(1.1,-2.23201749654651E-33,-0.29765));
#24054=CARTESIAN_POINT('Origin',(1.1,0.,0.));
#24055=CARTESIAN_POINT('Origin',(0.685838782044607,0.,-0.860014630714833));
#24056=CARTESIAN_POINT('',(0.918550922801216,-5.31350540756609E-33,-0.674432891191581));
#24057=CARTESIAN_POINT('',(0.453126641287998,8.49470414473068E-34,-1.04559637023808));
#24058=CARTESIAN_POINT('Origin',(0.685838782044607,0.,-0.860014630714833));
#24059=CARTESIAN_POINT('Origin',(-0.244773027351946,0.,-1.07242070340001));
#24060=CARTESIAN_POINT('',(0.0454142657089739,-2.23201749654651E-33,-1.1386540593921));
#24061=CARTESIAN_POINT('',(-0.534960320412865,-2.23201749654651E-33,-1.00618734740791));
#24062=CARTESIAN_POINT('Origin',(-0.244773027351946,0.,-1.07242070340001));
#24063=CARTESIAN_POINT('Origin',(-0.991065754692661,0.,-0.477272113029314));
#24064=CARTESIAN_POINT('',(-0.86192025974432,8.49470414473067E-34,-0.745445496560469));
#24065=CARTESIAN_POINT('',(-1.120211249641,-5.31350540756609E-33,-0.209098729498159));
#24066=CARTESIAN_POINT('Origin',(-0.991065754692661,0.,-0.477272113029314));
#24067=CARTESIAN_POINT('Origin',(-0.991065754692661,0.,0.477272113029314));
#24068=CARTESIAN_POINT('',(-1.120211249641,-2.23201749654651E-33,0.209098729498159));
#24069=CARTESIAN_POINT('',(-0.86192025974432,-2.23201749654651E-33,0.745445496560469));
#24070=CARTESIAN_POINT('Origin',(-0.991065754692661,0.,0.477272113029314));
#24071=CARTESIAN_POINT('Origin',(-0.244773027351946,0.,1.07242070340001));
#24072=CARTESIAN_POINT('',(-0.534960320412866,-2.23201749654651E-33,1.00618734740791));
#24073=CARTESIAN_POINT('',(0.0454142657089737,-2.23201749654651E-33,1.1386540593921));
#24074=CARTESIAN_POINT('Origin',(-0.244773027351946,0.,1.07242070340001));
#24075=CARTESIAN_POINT('Origin',(0.685838782044607,0.,0.860014630714833));
#24076=CARTESIAN_POINT('',(0.453126641287998,-2.23201749654651E-33,1.04559637023808));
#24077=CARTESIAN_POINT('',(0.918550922801216,-2.23201749654651E-33,0.674432891191581));
#24078=CARTESIAN_POINT('Origin',(0.685838782044607,0.,0.860014630714833));
#24079=CARTESIAN_POINT('',(0.,0.,0.));
#24080=CARTESIAN_POINT('Origin',(0.685838782044607,0.,0.860014630714833));
#24081=CARTESIAN_POINT('',(0.413083465285518,-0.05953,0.993751811093549));
#24082=CARTESIAN_POINT('',(0.876916659919095,-0.05953,0.623857181492959));
#24083=CARTESIAN_POINT('Ctrl Pts',(0.413083465285518,-0.05953,0.993751811093549));
#24084=CARTESIAN_POINT('Ctrl Pts',(0.419070565453383,-0.0925528133349865,
0.991263089003441));
#24085=CARTESIAN_POINT('Ctrl Pts',(0.430199341854858,-0.124911173756694,
0.986608710139579));
#24086=CARTESIAN_POINT('Ctrl Pts',(0.457978755888596,-0.177924977804098,
0.973971221090534));
#24087=CARTESIAN_POINT('Ctrl Pts',(0.473077587363685,-0.199697230012983,
0.966820759530997));
#24088=CARTESIAN_POINT('Ctrl Pts',(0.507057380724533,-0.237895043532788,
0.949440676105255));
#24089=CARTESIAN_POINT('Ctrl Pts',(0.525933334162555,-0.254319232363049,
0.939198248544428));
#24090=CARTESIAN_POINT('Ctrl Pts',(0.564362943424238,-0.28018331644634,
0.916597376014514));
#24091=CARTESIAN_POINT('Ctrl Pts',(0.585840553788742,-0.29104845371857,
0.903141581680914));
#24092=CARTESIAN_POINT('Ctrl Pts',(0.629305439856167,-0.30527573347708,
0.873412008702649));
#24093=CARTESIAN_POINT('Ctrl Pts',(0.651278921914856,-0.308638795020976,
0.857118508332695));
#24094=CARTESIAN_POINT('Ctrl Pts',(0.690705563850638,-0.308638795020976,
0.825676810575914));
#24095=CARTESIAN_POINT('Ctrl Pts',(0.711480111898423,-0.30527573347708,
0.807879894508811));
#24096=CARTESIAN_POINT('Ctrl Pts',(0.750136149454208,-0.29104845371857,
0.772120216227122));
#24097=CARTESIAN_POINT('Ctrl Pts',(0.768033796848072,-0.28018331644634,
0.754175290318038));
#24098=CARTESIAN_POINT('Ctrl Pts',(0.798619410861634,-0.254319232363049,
0.721738358858166));
#24099=CARTESIAN_POINT('Ctrl Pts',(0.812805334167529,-0.237895043532788,
0.705614819529209));
#24100=CARTESIAN_POINT('Ctrl Pts',(0.837310877969633,-0.199697230012983,
0.676354402927683));
#24101=CARTESIAN_POINT('Ctrl Pts',(0.847641868610495,-0.177924977804098,
0.663225258065736));
#24102=CARTESIAN_POINT('Ctrl Pts',(0.866144010579847,-0.124911173756694,
0.638954437806245));
#24103=CARTESIAN_POINT('Ctrl Pts',(0.873158080166742,-0.0925528133349865,
0.62914037979579));
#24104=CARTESIAN_POINT('Ctrl Pts',(0.876916659919095,-0.05953,0.623857181492959));
#24105=CARTESIAN_POINT('',(0.437601487681057,-0.05953,1.03511272300331));
#24106=CARTESIAN_POINT('Origin',(0.685838782044607,-0.05953,0.860014630714833));
#24107=CARTESIAN_POINT('',(0.911784794170997,-0.05953,0.656964154625313));
#24108=CARTESIAN_POINT('Ctrl Pts',(0.911784794170998,-0.0595300000000001,
0.656964154625312));
#24109=CARTESIAN_POINT('Ctrl Pts',(0.909827729890942,-0.0762225747374255,
0.659680317203144));
#24110=CARTESIAN_POINT('Ctrl Pts',(0.907004864562642,-0.0928409665394228,
0.663576540841106));
#24111=CARTESIAN_POINT('Ctrl Pts',(0.895234408667242,-0.144299303100741,
0.679480524217551));
#24112=CARTESIAN_POINT('Ctrl Pts',(0.882797231409153,-0.177024326825049,
0.695831250979106));
#24113=CARTESIAN_POINT('Ctrl Pts',(0.854332839576145,-0.227269801620064,
0.73042219438957));
#24114=CARTESIAN_POINT('Ctrl Pts',(0.834863020612702,-0.251265615809407,
0.752807465209441));
#24115=CARTESIAN_POINT('Ctrl Pts',(0.800439809856111,-0.279889827963178,
0.789147407129766));
#24116=CARTESIAN_POINT('Ctrl Pts',(0.781998747691871,-0.290879136862659,
0.80756613568454));
#24117=CARTESIAN_POINT('Ctrl Pts',(0.742239891936898,-0.305251990234487,
0.844254137480382));
#24118=CARTESIAN_POINT('Ctrl Pts',(0.720906778729541,-0.308638795020976,
0.862505527716294));
#24119=CARTESIAN_POINT('Ctrl Pts',(0.680463863683392,-0.308638795020976,
0.894757676234429));
#24120=CARTESIAN_POINT('Ctrl Pts',(0.657923009631182,-0.305251990234488,
0.91149460735272));
#24121=CARTESIAN_POINT('Ctrl Pts',(0.613307674922609,-0.290879136862659,
0.942092777160053));
#24122=CARTESIAN_POINT('Ctrl Pts',(0.591247219971725,-0.279889827963178,
0.955972930713954));
#24123=CARTESIAN_POINT('Ctrl Pts',(0.548158511259202,-0.251265615809407,
0.981446681891443));
#24124=CARTESIAN_POINT('Ctrl Pts',(0.522002043615455,-0.227269801620063,
0.995447160474328));
#24125=CARTESIAN_POINT('Ctrl Pts',(0.481944444320713,-0.177024326825049,
1.01550068154148));
#24126=CARTESIAN_POINT('Ctrl Pts',(0.463236132117164,-0.14429930310074,
1.0239876538093));
#24127=CARTESIAN_POINT('Ctrl Pts',(0.445111721969657,-0.0928409665394226,
1.03192403056628));
#24128=CARTESIAN_POINT('Ctrl Pts',(0.440685038163619,-0.0762225747374254,
1.03380912944435));
#24129=CARTESIAN_POINT('Ctrl Pts',(0.437601487681056,-0.05953,1.03511272300331));
#24130=CARTESIAN_POINT('Origin',(0.685838782044607,-0.05953,0.860014630714833));
#24131=CARTESIAN_POINT('Origin',(0.,-0.208355,0.));
#24132=CARTESIAN_POINT('',(0.0548532617164168,-0.05953,1.12247250791415));
#24133=CARTESIAN_POINT('Origin',(0.,-0.05953,0.));
#24134=CARTESIAN_POINT('',(-0.536443649899848,-0.05953,0.987512846410683));
#24135=CARTESIAN_POINT('Ctrl Pts',(0.0548532617164173,-0.0595300000000001,
1.12247250791414));
#24136=CARTESIAN_POINT('Ctrl Pts',(0.05150947068137,-0.0762225747374254,
1.12263591311425));
#24137=CARTESIAN_POINT('Ctrl Pts',(0.0467032526342597,-0.0928409665394227,
1.12285816383385));
#24138=CARTESIAN_POINT('Ctrl Pts',(0.0269302585198975,-0.144299303100741,
1.12357162229597));
#24139=CARTESIAN_POINT('Ctrl Pts',(0.006392292392153,-0.177024326825049,
1.12404235695137));
#24140=CARTESIAN_POINT('Ctrl Pts',(-0.0383992541984087,-0.227269801620063,
1.12335509974011));
#24141=CARTESIAN_POINT('Ctrl Pts',(-0.0680399972366993,-0.251265615809407,
1.12208997038458));
#24142=CARTESIAN_POINT('Ctrl Pts',(-0.117914228755037,-0.279889827963178,
1.1178344036749));
#24143=CARTESIAN_POINT('Ctrl Pts',(-0.14381238480104,-0.290879136862659,
1.11490049012186));
#24144=CARTESIAN_POINT('Ctrl Pts',(-0.19728546073067,-0.305251990234488,
1.10669035995599));
#24145=CARTESIAN_POINT('Ctrl Pts',(-0.224855950742601,-0.308638795020976,
1.10139101611326));
#24146=CARTESIAN_POINT('Ctrl Pts',(-0.275287440920027,-0.308638795020976,
1.0898803575765));
#24147=CARTESIAN_POINT('Ctrl Pts',(-0.302426893214945,-0.305251990234488,
1.08269251410343));
#24148=CARTESIAN_POINT('Ctrl Pts',(-0.35416671187353,-0.290879136862659,
1.06688848765783));
#24149=CARTESIAN_POINT('Ctrl Pts',(-0.3787731215897,-0.279889827963178,
1.05829506364875));
#24150=CARTESIAN_POINT('Ctrl Pts',(-0.425554672694338,-0.251265615809407,
1.04048957871266));
#24151=CARTESIAN_POINT('Ctrl Pts',(-0.452808978448581,-0.227269801620063,
1.02876878445619));
#24152=CARTESIAN_POINT('Ctrl Pts',(-0.493462957200432,-0.177024326825049,
1.0099536580922));
#24153=CARTESIAN_POINT('Ctrl Pts',(-0.511762781179148,-0.14429930310074,
1.00061845128527));
#24154=CARTESIAN_POINT('Ctrl Pts',(-0.529268075276157,-0.0928409665394226,
0.991396466802468));
#24155=CARTESIAN_POINT('Ctrl Pts',(-0.533501897135713,-0.0762225747374254,
0.989110885965947));
#24156=CARTESIAN_POINT('Ctrl Pts',(-0.536443649899848,-0.0595300000000001,
0.987512846410683));
#24157=CARTESIAN_POINT('',(-0.843383895613249,-0.05953,0.742736168477219));
#24158=CARTESIAN_POINT('Origin',(0.,-0.05953,0.));
#24159=CARTESIAN_POINT('',(-1.10653577764992,-0.05953,0.196295654879792));
#24160=CARTESIAN_POINT('Ctrl Pts',(-0.843383895613249,-0.0595300000000001,
0.742736168477219));
#24161=CARTESIAN_POINT('Ctrl Pts',(-0.84559647055299,-0.0762225747374255,
0.740223768851062));
#24162=CARTESIAN_POINT('Ctrl Pts',(-0.848766861100456,-0.0928409665394227,
0.736604687327351));
#24163=CARTESIAN_POINT('Ctrl Pts',(-0.861652925570091,-0.144299303100741,
0.721590372101268));
#24164=CARTESIAN_POINT('Ctrl Pts',(-0.87482617317514,-0.177024326825049,
0.705826641853758));
#24165=CARTESIAN_POINT('Ctrl Pts',(-0.902215926359523,-0.227269801620063,
0.670378702718353));
#24166=CARTESIAN_POINT('Ctrl Pts',(-0.919707509403859,-0.251265615809407,
0.646415841396062));
#24167=CARTESIAN_POINT('Ctrl Pts',(-0.947476448101718,-0.279889827963178,
0.604769294586516));
#24168=CARTESIAN_POINT('Ctrl Pts',(-0.961329858300736,-0.290879136862659,
0.582692035672022));
#24169=CARTESIAN_POINT('Ctrl Pts',(-0.988250837578047,-0.305251990234488,
0.535766169015486));
#24170=CARTESIAN_POINT('Ctrl Pts',(-1.00129756308006,-0.308638795020976,
0.510906605094603));
#24171=CARTESIAN_POINT('Ctrl Pts',(-1.02374168767024,-0.308638795020976,
0.46430090015576));
#24172=CARTESIAN_POINT('Ctrl Pts',(-1.03504317708586,-0.305251990234488,
0.438600874831839));
#24173=CARTESIAN_POINT('Ctrl Pts',(-1.05494634094458,-0.290879136862659,
0.388295406390235));
#24174=CARTESIAN_POINT('Ctrl Pts',(-1.06356957703048,-0.279889827963178,
0.363699428370917));
#24175=CARTESIAN_POINT('Ctrl Pts',(-1.0788165083757,-0.251265615809407,
0.316022600643821));
#24176=CARTESIAN_POINT('Ctrl Pts',(-1.08664560412098,-0.227269801620063,
0.287406530683752));
#24177=CARTESIAN_POINT('Ctrl Pts',(-1.09728268713976,-0.177024326825049,
0.243890930799337));
#24178=CARTESIAN_POINT('Ctrl Pts',(-1.10139388218929,-0.144299303100741,
0.22376314604679));
#24179=CARTESIAN_POINT('Ctrl Pts',(-1.10509821673782,-0.0928409665394227,
0.204327142733961));
#24180=CARTESIAN_POINT('Ctrl Pts',(-1.10595102243643,-0.0762225747374254,
0.199591971170104));
#24181=CARTESIAN_POINT('Ctrl Pts',(-1.10653577764992,-0.0595300000000001,
0.196295654879792));
#24182=CARTESIAN_POINT('',(-1.123812,-0.05953,1.37627276864339E-16));
#24183=CARTESIAN_POINT('Origin',(0.,-0.05953,0.));
#24184=CARTESIAN_POINT('',(-1.123812,-0.35718,1.37627276864339E-16));
#24185=CARTESIAN_POINT('',(-1.123812,-0.208355,1.37627276864339E-16));
#24186=CARTESIAN_POINT('Origin',(0.,-0.35718,0.));
#24187=CARTESIAN_POINT('',(-1.10653577764992,-0.05953,-0.196295654879793));
#24188=CARTESIAN_POINT('Origin',(0.,-0.05953,0.));
#24189=CARTESIAN_POINT('',(-0.843383895613249,-0.05953,-0.742736168477219));
#24190=CARTESIAN_POINT('Ctrl Pts',(-1.10653577764992,-0.0595300000000001,
-0.196295654879792));
#24191=CARTESIAN_POINT('Ctrl Pts',(-1.10595102243643,-0.0762225747374255,
-0.199591971170104));
#24192=CARTESIAN_POINT('Ctrl Pts',(-1.10509821673782,-0.0928409665394228,
-0.204327142733962));
#24193=CARTESIAN_POINT('Ctrl Pts',(-1.10139388218929,-0.144299303100741,
-0.22376314604679));
#24194=CARTESIAN_POINT('Ctrl Pts',(-1.09728268713976,-0.177024326825049,
-0.243890930799338));
#24195=CARTESIAN_POINT('Ctrl Pts',(-1.08664560412098,-0.227269801620063,
-0.287406530683753));
#24196=CARTESIAN_POINT('Ctrl Pts',(-1.0788165083757,-0.251265615809407,
-0.316022600643821));
#24197=CARTESIAN_POINT('Ctrl Pts',(-1.06356957703048,-0.279889827963178,
-0.363699428370918));
#24198=CARTESIAN_POINT('Ctrl Pts',(-1.05494634094458,-0.290879136862659,
-0.388295406390235));
#24199=CARTESIAN_POINT('Ctrl Pts',(-1.03504317708586,-0.305251990234488,
-0.438600874831839));
#24200=CARTESIAN_POINT('Ctrl Pts',(-1.02374168767024,-0.308638795020976,
-0.46430090015576));
#24201=CARTESIAN_POINT('Ctrl Pts',(-1.00129756308006,-0.308638795020976,
-0.510906605094603));
#24202=CARTESIAN_POINT('Ctrl Pts',(-0.988250837578047,-0.305251990234488,
-0.535766169015486));
#24203=CARTESIAN_POINT('Ctrl Pts',(-0.961329858300736,-0.290879136862659,
-0.582692035672022));
#24204=CARTESIAN_POINT('Ctrl Pts',(-0.947476448101718,-0.279889827963178,
-0.604769294586516));
#24205=CARTESIAN_POINT('Ctrl Pts',(-0.919707509403859,-0.251265615809407,
-0.646415841396062));
#24206=CARTESIAN_POINT('Ctrl Pts',(-0.902215926359523,-0.227269801620064,
-0.670378702718353));
#24207=CARTESIAN_POINT('Ctrl Pts',(-0.87482617317514,-0.177024326825049,
-0.705826641853758));
#24208=CARTESIAN_POINT('Ctrl Pts',(-0.861652925570091,-0.144299303100741,
-0.721590372101268));
#24209=CARTESIAN_POINT('Ctrl Pts',(-0.848766861100456,-0.0928409665394229,
-0.736604687327351));
#24210=CARTESIAN_POINT('Ctrl Pts',(-0.84559647055299,-0.0762225747374255,
-0.740223768851063));
#24211=CARTESIAN_POINT('Ctrl Pts',(-0.843383895613249,-0.0595300000000001,
-0.742736168477219));
#24212=CARTESIAN_POINT('',(-0.536443649899847,-0.05953,-0.987512846410683));
#24213=CARTESIAN_POINT('Origin',(0.,-0.05953,0.));
#24214=CARTESIAN_POINT('',(0.0548532617164172,-0.05953,-1.12247250791415));
#24215=CARTESIAN_POINT('Ctrl Pts',(-0.536443649899848,-0.0595300000000001,
-0.987512846410683));
#24216=CARTESIAN_POINT('Ctrl Pts',(-0.533501897135712,-0.0762225747374254,
-0.989110885965947));
#24217=CARTESIAN_POINT('Ctrl Pts',(-0.529268075276156,-0.0928409665394227,
-0.991396466802469));
#24218=CARTESIAN_POINT('Ctrl Pts',(-0.511762781179147,-0.144299303100741,
-1.00061845128527));
#24219=CARTESIAN_POINT('Ctrl Pts',(-0.493462957200432,-0.177024326825049,
-1.0099536580922));
#24220=CARTESIAN_POINT('Ctrl Pts',(-0.45280897844858,-0.227269801620063,
-1.02876878445619));
#24221=CARTESIAN_POINT('Ctrl Pts',(-0.425554672694337,-0.251265615809407,
-1.04048957871266));
#24222=CARTESIAN_POINT('Ctrl Pts',(-0.3787731215897,-0.279889827963178,
-1.05829506364875));
#24223=CARTESIAN_POINT('Ctrl Pts',(-0.354166711873529,-0.290879136862659,
-1.06688848765783));
#24224=CARTESIAN_POINT('Ctrl Pts',(-0.302426893214944,-0.305251990234488,
-1.08269251410343));
#24225=CARTESIAN_POINT('Ctrl Pts',(-0.275287440920027,-0.308638795020976,
-1.0898803575765));
#24226=CARTESIAN_POINT('Ctrl Pts',(-0.224855950742601,-0.308638795020976,
-1.10139101611326));
#24227=CARTESIAN_POINT('Ctrl Pts',(-0.19728546073067,-0.305251990234488,
-1.10669035995599));
#24228=CARTESIAN_POINT('Ctrl Pts',(-0.143812384801039,-0.290879136862659,
-1.11490049012186));
#24229=CARTESIAN_POINT('Ctrl Pts',(-0.117914228755037,-0.279889827963178,
-1.1178344036749));
#24230=CARTESIAN_POINT('Ctrl Pts',(-0.0680399972366989,-0.251265615809407,
-1.12208997038458));
#24231=CARTESIAN_POINT('Ctrl Pts',(-0.0383992541984084,-0.227269801620063,
-1.12335509974011));
#24232=CARTESIAN_POINT('Ctrl Pts',(0.00639229239215326,-0.177024326825049,
-1.12404235695137));
#24233=CARTESIAN_POINT('Ctrl Pts',(0.0269302585198977,-0.144299303100741,
-1.12357162229597));
#24234=CARTESIAN_POINT('Ctrl Pts',(0.04670325263426,-0.0928409665394228,
-1.12285816383385));
#24235=CARTESIAN_POINT('Ctrl Pts',(0.0515094706813703,-0.0762225747374255,
-1.12263591311425));
#24236=CARTESIAN_POINT('Ctrl Pts',(0.0548532617164176,-0.0595300000000001,
-1.12247250791414));
#24237=CARTESIAN_POINT('',(0.437601487681057,-0.05953,-1.03511272300331));
#24238=CARTESIAN_POINT('Origin',(0.,-0.05953,0.));
#24239=CARTESIAN_POINT('',(0.911784794170997,-0.05953,-0.656964154625313));
#24240=CARTESIAN_POINT('Ctrl Pts',(0.437601487681056,-0.0595300000000001,
-1.03511272300331));
#24241=CARTESIAN_POINT('Ctrl Pts',(0.440685038163619,-0.0762225747374255,
-1.03380912944435));
#24242=CARTESIAN_POINT('Ctrl Pts',(0.445111721969657,-0.0928409665394228,
-1.03192403056628));
#24243=CARTESIAN_POINT('Ctrl Pts',(0.463236132117164,-0.144299303100741,
-1.0239876538093));
#24244=CARTESIAN_POINT('Ctrl Pts',(0.481944444320713,-0.177024326825049,
-1.01550068154148));
#24245=CARTESIAN_POINT('Ctrl Pts',(0.522002043615455,-0.227269801620064,
-0.995447160474328));
#24246=CARTESIAN_POINT('Ctrl Pts',(0.548158511259203,-0.251265615809407,
-0.981446681891443));
#24247=CARTESIAN_POINT('Ctrl Pts',(0.591247219971725,-0.279889827963178,
-0.955972930713954));
#24248=CARTESIAN_POINT('Ctrl Pts',(0.613307674922609,-0.290879136862659,
-0.942092777160053));
#24249=CARTESIAN_POINT('Ctrl Pts',(0.657923009631182,-0.305251990234487,
-0.91149460735272));
#24250=CARTESIAN_POINT('Ctrl Pts',(0.680463863683393,-0.308638795020976,
-0.894757676234429));
#24251=CARTESIAN_POINT('Ctrl Pts',(0.720906778729542,-0.308638795020976,
-0.862505527716294));
#24252=CARTESIAN_POINT('Ctrl Pts',(0.742239891936899,-0.305251990234488,
-0.844254137480381));
#24253=CARTESIAN_POINT('Ctrl Pts',(0.781998747691872,-0.290879136862659,
-0.80756613568454));
#24254=CARTESIAN_POINT('Ctrl Pts',(0.800439809856112,-0.279889827963178,
-0.789147407129765));
#24255=CARTESIAN_POINT('Ctrl Pts',(0.834863020612702,-0.251265615809407,
-0.752807465209441));
#24256=CARTESIAN_POINT('Ctrl Pts',(0.854332839576145,-0.227269801620064,
-0.73042219438957));
#24257=CARTESIAN_POINT('Ctrl Pts',(0.882797231409153,-0.177024326825049,
-0.695831250979106));
#24258=CARTESIAN_POINT('Ctrl Pts',(0.895234408667242,-0.144299303100741,
-0.679480524217551));
#24259=CARTESIAN_POINT('Ctrl Pts',(0.907004864562642,-0.0928409665394228,
-0.663576540841106));
#24260=CARTESIAN_POINT('Ctrl Pts',(0.909827729890942,-0.0762225747374256,
-0.659680317203144));
#24261=CARTESIAN_POINT('Ctrl Pts',(0.911784794170998,-0.0595300000000001,
-0.656964154625312));
#24262=CARTESIAN_POINT('',(1.08212377959455,-0.05953,-0.303251606722892));
#24263=CARTESIAN_POINT('Origin',(0.,-0.05953,0.));
#24264=CARTESIAN_POINT('',(1.08212377959455,-0.05953,0.303251606722892));
#24265=CARTESIAN_POINT('Ctrl Pts',(1.08212377959455,-0.0595300000000001,
-0.303251606722892));
#24266=CARTESIAN_POINT('Ctrl Pts',(1.0830271513892,-0.0762225747374255,
-0.300028012588062));
#24267=CARTESIAN_POINT('Ctrl Pts',(1.08431331394788,-0.0928409665394228,
-0.2953917518996));
#24268=CARTESIAN_POINT('Ctrl Pts',(1.08940878963422,-0.144299303100741,
-0.276273267473431));
#24269=CARTESIAN_POINT('Ctrl Pts',(1.09443784939331,-0.177024326825049,
-0.256354979351213));
#24270=CARTESIAN_POINT('Ctrl Pts',(1.10373487993589,-0.227269801620064,
-0.212533521233765));
#24271=CARTESIAN_POINT('Ctrl Pts',(1.10909715583869,-0.251265615809407,
-0.183354415742157));
#24272=CARTESIAN_POINT('Ctrl Pts',(1.1160463456491,-0.279889827963178,-0.133783682657561));
#24273=CARTESIAN_POINT('Ctrl Pts',(1.11894887330541,-0.290879136862659,
-0.107881990270302));
#24274=CARTESIAN_POINT('Ctrl Pts',(1.12284346704144,-0.305251990234488,
-0.0539226701638766));
#24275=CARTESIAN_POINT('Ctrl Pts',(1.123812,-0.308638795020976,-0.025864214957475));
#24276=CARTESIAN_POINT('Ctrl Pts',(1.123812,-0.308638795020976,0.025864214957475));
#24277=CARTESIAN_POINT('Ctrl Pts',(1.12284346704144,-0.305251990234488,
0.0539226701638766));
#24278=CARTESIAN_POINT('Ctrl Pts',(1.11894887330541,-0.290879136862659,
0.107881990270302));
#24279=CARTESIAN_POINT('Ctrl Pts',(1.1160463456491,-0.279889827963178,0.133783682657561));
#24280=CARTESIAN_POINT('Ctrl Pts',(1.10909715583869,-0.251265615809407,
0.183354415742157));
#24281=CARTESIAN_POINT('Ctrl Pts',(1.10373487993589,-0.227269801620064,
0.212533521233765));
#24282=CARTESIAN_POINT('Ctrl Pts',(1.09443784939331,-0.177024326825049,
0.256354979351213));
#24283=CARTESIAN_POINT('Ctrl Pts',(1.08940878963422,-0.144299303100741,
0.276273267473431));
#24284=CARTESIAN_POINT('Ctrl Pts',(1.08431331394788,-0.0928409665394228,
0.2953917518996));
#24285=CARTESIAN_POINT('Ctrl Pts',(1.0830271513892,-0.0762225747374255,
0.300028012588062));
#24286=CARTESIAN_POINT('Ctrl Pts',(1.08212377959455,-0.0595300000000001,
0.303251606722892));
#24287=CARTESIAN_POINT('Origin',(0.,-0.05953,0.));
#24288=CARTESIAN_POINT('Origin',(0.,-0.05953,0.));
#24289=CARTESIAN_POINT('',(0.0589974094846122,-0.05953,1.07456964270265));
#24290=CARTESIAN_POINT('Origin',(0.,-0.05953,0.));
#24291=CARTESIAN_POINT('Origin',(-0.244773027351946,-0.05953,1.07242070340001));
#24292=CARTESIAN_POINT('Origin',(-0.244773027351946,0.,1.07242070340001));
#24293=CARTESIAN_POINT('',(-0.519393123750572,-0.05953,0.942555777842682));
#24294=CARTESIAN_POINT('Ctrl Pts',(-0.519393123750572,-0.05953,0.942555777842682));
#24295=CARTESIAN_POINT('Ctrl Pts',(-0.513714466572041,-0.0925528133349865,
0.945684988399766));
#24296=CARTESIAN_POINT('Ctrl Pts',(-0.503136848051455,-0.124911173756694,
0.951483858396181));
#24297=CARTESIAN_POINT('Ctrl Pts',(-0.47593627990192,-0.177924977804098,
0.965323333309091));
#24298=CARTESIAN_POINT('Ctrl Pts',(-0.460931856495794,-0.199697230012983,
0.972669835243841));
#24299=CARTESIAN_POINT('Ctrl Pts',(-0.426157505475872,-0.237895043532788,
0.988400002689705));
#24300=CARTESIAN_POINT('Ctrl Pts',(-0.406380688682952,-0.254319232363049,
0.996771768218699));
#24301=CARTESIAN_POINT('Ctrl Pts',(-0.364750145543744,-0.28018331644634,
1.01272583306292));
#24302=CARTESIAN_POINT('Ctrl Pts',(-0.340838910881557,-0.29104845371857,
1.02112815447116));
#24303=CARTESIAN_POINT('Ctrl Pts',(-0.290495481564827,-0.30527573347708,
1.036574285215));
#24304=CARTESIAN_POINT('Ctrl Pts',(-0.264056468041074,-0.308638795020976,
1.04359501395068));
#24305=CARTESIAN_POINT('Ctrl Pts',(-0.214892249704082,-0.308638795020976,
1.05481642595959));
#24306=CARTESIAN_POINT('Ctrl Pts',(-0.188025341585962,-0.30527573347708,
1.05996242598502));
#24307=CARTESIAN_POINT('Ctrl Pts',(-0.135965654106109,-0.29104845371857,
1.06788913840721));
#24308=CARTESIAN_POINT('Ctrl Pts',(-0.110776745452494,-0.28018331644634,
1.07069360430242));
#24309=CARTESIAN_POINT('Ctrl Pts',(-0.0663467128214646,-0.254319232363049,
1.07438230428002));
#24310=CARTESIAN_POINT('Ctrl Pts',(-0.0448960436540983,-0.237895043532788,
1.07542044338697));
#24311=CARTESIAN_POINT('Ctrl Pts',(-0.00674037211528124,-0.199697230012983,
1.07633607767727));
#24312=CARTESIAN_POINT('Ctrl Pts',(0.00996567398334777,-0.177924977804098,
1.07622728347683));
#24313=CARTESIAN_POINT('Ctrl Pts',(0.0404772621979741,-0.124911173756694,
1.07556023164702));
#24314=CARTESIAN_POINT('Ctrl Pts',(0.0525234025782719,-0.0925528133349865,
1.07492508698591));
#24315=CARTESIAN_POINT('Ctrl Pts',(0.0589974094846124,-0.05953,1.07456964270265));
#24316=CARTESIAN_POINT('Origin',(-0.244773027351946,-0.05953,1.07242070340001));
#24317=CARTESIAN_POINT('Origin',(0.,-0.05953,0.));
#24318=CARTESIAN_POINT('',(-0.803348093619616,-0.05953,0.716109245731214));
#24319=CARTESIAN_POINT('Origin',(0.,-0.05953,0.));
#24320=CARTESIAN_POINT('Origin',(-0.991065754692661,-0.05953,0.477272113029314));
#24321=CARTESIAN_POINT('Origin',(-0.991065754692661,0.,0.477272113029314));
#24322=CARTESIAN_POINT('',(-1.06075609691358,-0.05953,0.181596019242328));
#24323=CARTESIAN_POINT('Ctrl Pts',(-1.06075609691358,-0.05953,0.181596019242328));
#24324=CARTESIAN_POINT('Ctrl Pts',(-1.05966202740332,-0.0925528133349865,
0.187986803072856));
#24325=CARTESIAN_POINT('Ctrl Pts',(-1.05760072925372,-0.124911173756694,
0.199872254546857));
#24326=CARTESIAN_POINT('Ctrl Pts',(-1.05146158959546,-0.177924977804098,
0.22976728653846));
#24327=CARTESIAN_POINT('Ctrl Pts',(-1.04785021111757,-0.199697230012983,
0.246078686169301));
#24328=CARTESIAN_POINT('Ctrl Pts',(-1.03846709802406,-0.237895043532788,
0.283073967563097));
#24329=CARTESIAN_POINT('Ctrl Pts',(-1.03268176429485,-0.254319232363049,
0.303755815985685));
#24330=CARTESIAN_POINT('Ctrl Pts',(-1.01919893537026,-0.28018331644634,
0.346251081972725));
#24331=CARTESIAN_POINT('Ctrl Pts',(-1.01085972381132,-0.29104845371857,
0.370184399726282));
#24332=CARTESIAN_POINT('Ctrl Pts',(-0.99154738033959,-0.30527573347708,
0.419174982698463));
#24333=CARTESIAN_POINT('Ctrl Pts',(-0.980551951791748,-0.308638795020976,
0.444223188605045));
#24334=CARTESIAN_POINT('Ctrl Pts',(-0.958671816228589,-0.308638795020976,
0.489657758261848));
#24335=CARTESIAN_POINT('Ctrl Pts',(-0.945943877838127,-0.30527573347708,
0.51387163140139));
#24336=CARTESIAN_POINT('Ctrl Pts',(-0.91968254693063,-0.29104845371857,
0.559515758398093));
#24337=CARTESIAN_POINT('Ctrl Pts',(-0.906170138993533,-0.28018331644634,
0.580957796077825));
#24338=CARTESIAN_POINT('Ctrl Pts',(-0.8813524085237,-0.254319232363049,
0.617994461173994));
#24339=CARTESIAN_POINT('Ctrl Pts',(-0.868789784891799,-0.237895043532788,
0.635412538795143));
#24340=CARTESIAN_POINT('Ctrl Pts',(-0.845715984518854,-0.199697230012983,
0.66581473268113));
#24341=CARTESIAN_POINT('Ctrl Pts',(-0.835214876415962,-0.177924977804098,
0.678808213394124));
#24342=CARTESIAN_POINT('Ctrl Pts',(-0.815669690204649,-0.124911173756694,
0.702247233627224));
#24343=CARTESIAN_POINT('Ctrl Pts',(-0.807662468433796,-0.0925528133349865,
0.711269279199861));
#24344=CARTESIAN_POINT('Ctrl Pts',(-0.803348093619616,-0.05953,0.716109245731214));
#24345=CARTESIAN_POINT('Origin',(-0.991065754692661,-0.05953,0.477272113029314));
#24346=CARTESIAN_POINT('Origin',(0.,-0.05953,0.));
#24347=CARTESIAN_POINT('',(-1.076188,-0.05953,1.31795018948079E-16));
#24348=CARTESIAN_POINT('Origin',(0.,-0.05953,0.));
#24349=CARTESIAN_POINT('',(-1.06075609691358,-0.05953,-0.181596019242328));
#24350=CARTESIAN_POINT('Origin',(0.,-0.05953,0.));
#24351=CARTESIAN_POINT('Origin',(-0.991065754692661,-0.05953,-0.477272113029314));
#24352=CARTESIAN_POINT('Origin',(-0.991065754692661,0.,-0.477272113029314));
#24353=CARTESIAN_POINT('',(-0.803348093619616,-0.05953,-0.716109245731215));
#24354=CARTESIAN_POINT('Ctrl Pts',(-0.803348093619616,-0.05953,-0.716109245731215));
#24355=CARTESIAN_POINT('Ctrl Pts',(-0.807662468433795,-0.0925528133349865,
-0.711269279199862));
#24356=CARTESIAN_POINT('Ctrl Pts',(-0.815669690204649,-0.124911173756694,
-0.702247233627224));
#24357=CARTESIAN_POINT('Ctrl Pts',(-0.835214876415962,-0.177924977804098,
-0.678808213394124));
#24358=CARTESIAN_POINT('Ctrl Pts',(-0.845715984518854,-0.199697230012983,
-0.66581473268113));
#24359=CARTESIAN_POINT('Ctrl Pts',(-0.868789784891799,-0.237895043532788,
-0.635412538795143));
#24360=CARTESIAN_POINT('Ctrl Pts',(-0.8813524085237,-0.254319232363049,
-0.617994461173994));
#24361=CARTESIAN_POINT('Ctrl Pts',(-0.906170138993533,-0.28018331644634,
-0.580957796077826));
#24362=CARTESIAN_POINT('Ctrl Pts',(-0.91968254693063,-0.29104845371857,
-0.559515758398093));
#24363=CARTESIAN_POINT('Ctrl Pts',(-0.945943877838127,-0.30527573347708,
-0.51387163140139));
#24364=CARTESIAN_POINT('Ctrl Pts',(-0.958671816228589,-0.308638795020976,
-0.489657758261848));
#24365=CARTESIAN_POINT('Ctrl Pts',(-0.980551951791748,-0.308638795020976,
-0.444223188605045));
#24366=CARTESIAN_POINT('Ctrl Pts',(-0.99154738033959,-0.30527573347708,
-0.419174982698463));
#24367=CARTESIAN_POINT('Ctrl Pts',(-1.01085972381132,-0.29104845371857,
-0.370184399726282));
#24368=CARTESIAN_POINT('Ctrl Pts',(-1.01919893537026,-0.28018331644634,
-0.346251081972725));
#24369=CARTESIAN_POINT('Ctrl Pts',(-1.03268176429485,-0.254319232363049,
-0.303755815985685));
#24370=CARTESIAN_POINT('Ctrl Pts',(-1.03846709802406,-0.237895043532788,
-0.283073967563097));
#24371=CARTESIAN_POINT('Ctrl Pts',(-1.04785021111757,-0.199697230012983,
-0.246078686169302));
#24372=CARTESIAN_POINT('Ctrl Pts',(-1.05146158959546,-0.177924977804098,
-0.229767286538461));
#24373=CARTESIAN_POINT('Ctrl Pts',(-1.05760072925372,-0.124911173756694,
-0.199872254546858));
#24374=CARTESIAN_POINT('Ctrl Pts',(-1.05966202740332,-0.0925528133349864,
-0.187986803072857));
#24375=CARTESIAN_POINT('Ctrl Pts',(-1.06075609691358,-0.05953,-0.181596019242328));
#24376=CARTESIAN_POINT('Origin',(-0.991065754692661,-0.05953,-0.477272113029314));
#24377=CARTESIAN_POINT('Origin',(0.,-0.05953,0.));
#24378=CARTESIAN_POINT('',(-0.519393123750572,-0.05953,-0.942555777842682));
#24379=CARTESIAN_POINT('Origin',(0.,-0.05953,0.));
#24380=CARTESIAN_POINT('Origin',(-0.244773027351946,-0.05953,-1.07242070340001));
#24381=CARTESIAN_POINT('Origin',(-0.244773027351946,0.,-1.07242070340001));
#24382=CARTESIAN_POINT('',(0.0589974094846125,-0.05953,-1.07456964270265));
#24383=CARTESIAN_POINT('Ctrl Pts',(0.0589974094846127,-0.05953,-1.07456964270265));
#24384=CARTESIAN_POINT('Ctrl Pts',(0.0525234025782722,-0.0925528133349865,
-1.07492508698591));
#24385=CARTESIAN_POINT('Ctrl Pts',(0.0404772621979744,-0.124911173756694,
-1.07556023164702));
#24386=CARTESIAN_POINT('Ctrl Pts',(0.0099656739833481,-0.177924977804098,
-1.07622728347683));
#24387=CARTESIAN_POINT('Ctrl Pts',(-0.00674037211528096,-0.199697230012983,
-1.07633607767727));
#24388=CARTESIAN_POINT('Ctrl Pts',(-0.044896043654098,-0.237895043532788,
-1.07542044338697));
#24389=CARTESIAN_POINT('Ctrl Pts',(-0.0663467128214644,-0.254319232363049,
-1.07438230428002));
#24390=CARTESIAN_POINT('Ctrl Pts',(-0.110776745452493,-0.28018331644634,
-1.07069360430242));
#24391=CARTESIAN_POINT('Ctrl Pts',(-0.135965654106109,-0.29104845371857,
-1.06788913840721));
#24392=CARTESIAN_POINT('Ctrl Pts',(-0.188025341585962,-0.30527573347708,
-1.05996242598502));
#24393=CARTESIAN_POINT('Ctrl Pts',(-0.214892249704082,-0.308638795020976,
-1.05481642595959));
#24394=CARTESIAN_POINT('Ctrl Pts',(-0.264056468041074,-0.308638795020976,
-1.04359501395068));
#24395=CARTESIAN_POINT('Ctrl Pts',(-0.290495481564827,-0.30527573347708,
-1.036574285215));
#24396=CARTESIAN_POINT('Ctrl Pts',(-0.340838910881557,-0.291048453718569,
-1.02112815447116));
#24397=CARTESIAN_POINT('Ctrl Pts',(-0.364750145543744,-0.28018331644634,
-1.01272583306292));
#24398=CARTESIAN_POINT('Ctrl Pts',(-0.406380688682952,-0.254319232363049,
-0.996771768218699));
#24399=CARTESIAN_POINT('Ctrl Pts',(-0.426157505475872,-0.237895043532788,
-0.988400002689705));
#24400=CARTESIAN_POINT('Ctrl Pts',(-0.460931856495794,-0.199697230012983,
-0.972669835243841));
#24401=CARTESIAN_POINT('Ctrl Pts',(-0.475936279901919,-0.177924977804098,
-0.965323333309091));
#24402=CARTESIAN_POINT('Ctrl Pts',(-0.503136848051454,-0.124911173756694,
-0.951483858396181));
#24403=CARTESIAN_POINT('Ctrl Pts',(-0.513714466572041,-0.0925528133349865,
-0.945684988399766));
#24404=CARTESIAN_POINT('Ctrl Pts',(-0.519393123750572,-0.05953,-0.942555777842682));
#24405=CARTESIAN_POINT('Origin',(-0.244773027351946,-0.05953,-1.07242070340001));
#24406=CARTESIAN_POINT('Origin',(0.,-0.05953,0.));
#24407=CARTESIAN_POINT('',(0.413083465285518,-0.05953,-0.993751811093549));
#24408=CARTESIAN_POINT('Origin',(0.,-0.05953,0.));
#24409=CARTESIAN_POINT('Origin',(0.685838782044607,-0.05953,-0.860014630714833));
#24410=CARTESIAN_POINT('Origin',(0.685838782044607,0.,-0.860014630714833));
#24411=CARTESIAN_POINT('',(0.876916659919095,-0.05953,-0.623857181492959));
#24412=CARTESIAN_POINT('Ctrl Pts',(0.876916659919095,-0.05953,-0.623857181492958));
#24413=CARTESIAN_POINT('Ctrl Pts',(0.873158080166742,-0.0925528133349865,
-0.62914037979579));
#24414=CARTESIAN_POINT('Ctrl Pts',(0.866144010579847,-0.124911173756694,
-0.638954437806245));
#24415=CARTESIAN_POINT('Ctrl Pts',(0.847641868610495,-0.177924977804098,
-0.663225258065736));
#24416=CARTESIAN_POINT('Ctrl Pts',(0.837310877969633,-0.199697230012983,
-0.676354402927683));
#24417=CARTESIAN_POINT('Ctrl Pts',(0.81280533416753,-0.237895043532788,
-0.705614819529209));
#24418=CARTESIAN_POINT('Ctrl Pts',(0.798619410861634,-0.254319232363049,
-0.721738358858166));
#24419=CARTESIAN_POINT('Ctrl Pts',(0.768033796848072,-0.28018331644634,
-0.754175290318038));
#24420=CARTESIAN_POINT('Ctrl Pts',(0.750136149454208,-0.29104845371857,
-0.772120216227122));
#24421=CARTESIAN_POINT('Ctrl Pts',(0.711480111898423,-0.30527573347708,
-0.807879894508811));
#24422=CARTESIAN_POINT('Ctrl Pts',(0.690705563850638,-0.308638795020976,
-0.825676810575913));
#24423=CARTESIAN_POINT('Ctrl Pts',(0.651278921914856,-0.308638795020976,
-0.857118508332695));
#24424=CARTESIAN_POINT('Ctrl Pts',(0.629305439856167,-0.30527573347708,
-0.873412008702649));
#24425=CARTESIAN_POINT('Ctrl Pts',(0.585840553788742,-0.29104845371857,
-0.903141581680914));
#24426=CARTESIAN_POINT('Ctrl Pts',(0.564362943424239,-0.28018331644634,
-0.916597376014514));
#24427=CARTESIAN_POINT('Ctrl Pts',(0.525933334162556,-0.254319232363049,
-0.939198248544427));
#24428=CARTESIAN_POINT('Ctrl Pts',(0.507057380724533,-0.237895043532788,
-0.949440676105255));
#24429=CARTESIAN_POINT('Ctrl Pts',(0.473077587363686,-0.199697230012983,
-0.966820759530997));
#24430=CARTESIAN_POINT('Ctrl Pts',(0.457978755888596,-0.177924977804098,
-0.973971221090534));
#24431=CARTESIAN_POINT('Ctrl Pts',(0.430199341854858,-0.124911173756694,
-0.986608710139579));
#24432=CARTESIAN_POINT('Ctrl Pts',(0.419070565453384,-0.0925528133349865,
-0.991263089003441));
#24433=CARTESIAN_POINT('Ctrl Pts',(0.413083465285518,-0.05953,-0.993751811093549));
#24434=CARTESIAN_POINT('Origin',(0.685838782044607,-0.05953,-0.860014630714833));
#24435=CARTESIAN_POINT('Origin',(0.,-0.208355,0.));
#24436=CARTESIAN_POINT('',(-1.076188,-0.35718,1.31795018948079E-16));
#24437=CARTESIAN_POINT('Origin',(0.,-0.35718,0.));
#24438=CARTESIAN_POINT('',(-1.076188,-0.208355,1.31795018948079E-16));
#24439=CARTESIAN_POINT('',(1.03449977959455,-0.05953,0.296632461748266));
#24440=CARTESIAN_POINT('Origin',(0.,-0.05953,0.));
#24441=CARTESIAN_POINT('',(1.03449977959455,-0.05953,-0.296632461748266));
#24442=CARTESIAN_POINT('Ctrl Pts',(1.03449977959455,-0.05953,0.296632461748267));
#24443=CARTESIAN_POINT('Ctrl Pts',(1.03628691421076,-0.0925528133349865,
0.290399865505497));
#24444=CARTESIAN_POINT('Ctrl Pts',(1.03958665287714,-0.124911173756694,
0.278797079997872));
#24445=CARTESIAN_POINT('Ctrl Pts',(1.0470264474309,-0.177924977804098,0.249198913998601));
#24446=CARTESIAN_POINT('Ctrl Pts',(1.05084995891418,-0.199697230012983,
0.232935932341942));
#24447=CARTESIAN_POINT('Ctrl Pts',(1.05844771715377,-0.237895043532788,
0.195533155353269));
#24448=CARTESIAN_POINT('Ctrl Pts',(1.06220882929878,-0.254319232363049,
0.17438929156337));
#24449=CARTESIAN_POINT('Ctrl Pts',(1.06849922508772,-0.28018331644634,0.130252399648131));
#24450=CARTESIAN_POINT('Ctrl Pts',(1.07137013248666,-0.29104845371857,0.105070977154072));
#24451=CARTESIAN_POINT('Ctrl Pts',(1.07522652957392,-0.30527573347708,0.0525526752791107));
#24452=CARTESIAN_POINT('Ctrl Pts',(1.076188,-0.308638795020976,0.025214283908933));
#24453=CARTESIAN_POINT('Ctrl Pts',(1.076188,-0.308638795020976,-0.025214283908933));
#24454=CARTESIAN_POINT('Ctrl Pts',(1.07522652957392,-0.30527573347708,-0.0525526752791107));
#24455=CARTESIAN_POINT('Ctrl Pts',(1.07137013248666,-0.29104845371857,-0.105070977154072));
#24456=CARTESIAN_POINT('Ctrl Pts',(1.06849922508772,-0.28018331644634,-0.130252399648131));
#24457=CARTESIAN_POINT('Ctrl Pts',(1.06220882929878,-0.254319232363049,
-0.17438929156337));
#24458=CARTESIAN_POINT('Ctrl Pts',(1.05844771715377,-0.237895043532788,
-0.195533155353269));
#24459=CARTESIAN_POINT('Ctrl Pts',(1.05084995891418,-0.199697230012983,
-0.232935932341942));
#24460=CARTESIAN_POINT('Ctrl Pts',(1.0470264474309,-0.177924977804098,-0.249198913998601));
#24461=CARTESIAN_POINT('Ctrl Pts',(1.03958665287714,-0.124911173756694,
-0.278797079997872));
#24462=CARTESIAN_POINT('Ctrl Pts',(1.03628691421076,-0.0925528133349865,
-0.290399865505497));
#24463=CARTESIAN_POINT('Ctrl Pts',(1.03449977959455,-0.05953,-0.296632461748267));
#24464=CARTESIAN_POINT('Origin',(0.,-0.05953,0.));
#24465=CARTESIAN_POINT('Origin',(0.,-0.05953,0.));
#24466=CARTESIAN_POINT('Origin',(1.1,-0.05953,0.));
#24467=CARTESIAN_POINT('Origin',(1.1,0.,0.));
#24468=CARTESIAN_POINT('Origin',(1.1,-0.05953,0.));
#24469=CARTESIAN_POINT('Origin',(0.,-0.35718,0.));
#24470=CARTESIAN_POINT('Origin',(0.,-0.05953,0.));
#24471=CARTESIAN_POINT('',(0.,0.,0.));
#24472=CARTESIAN_POINT('Origin',(1.119765,0.495,0.));
#24473=CARTESIAN_POINT('',(-1.119765,0.495,-1.37131662304724E-16));
#24474=CARTESIAN_POINT('Origin',(0.,0.495,0.));
#24475=CARTESIAN_POINT('',(-1.085235,0.495,-1.32902956907268E-16));
#24476=CARTESIAN_POINT('Origin',(0.,0.495,0.));
#24477=CARTESIAN_POINT('Origin',(0.,0.4575,0.));
#24478=CARTESIAN_POINT('',(-1.119765,0.42,-1.37131662304724E-16));
#24479=CARTESIAN_POINT('Origin',(0.,0.42,0.));
#24480=CARTESIAN_POINT('',(-1.119765,0.4575,-1.37131662304724E-16));
#24481=CARTESIAN_POINT('Origin',(1.085235,0.42,0.));
#24482=CARTESIAN_POINT('',(-1.085235,0.42,-1.32902956907268E-16));
#24483=CARTESIAN_POINT('Origin',(0.,0.42,0.));
#24484=CARTESIAN_POINT('Origin',(0.,0.4575,0.));
#24485=CARTESIAN_POINT('',(-1.085235,0.4575,-1.32902956907268E-16));
#24486=CARTESIAN_POINT('Origin',(1.119765,-0.42,0.));
#24487=CARTESIAN_POINT('',(-1.119765,-0.42,-1.37131662304724E-16));
#24488=CARTESIAN_POINT('Origin',(0.,-0.42,0.));
#24489=CARTESIAN_POINT('',(-1.085235,-0.42,-1.32902956907268E-16));
#24490=CARTESIAN_POINT('Origin',(0.,-0.42,0.));
#24491=CARTESIAN_POINT('Origin',(0.,-0.4575,0.));
#24492=CARTESIAN_POINT('',(-1.119765,-0.495,-1.37131662304724E-16));
#24493=CARTESIAN_POINT('Origin',(0.,-0.495,0.));
#24494=CARTESIAN_POINT('',(-1.119765,-0.4575,-1.37131662304724E-16));
#24495=CARTESIAN_POINT('Origin',(1.085235,-0.495,0.));
#24496=CARTESIAN_POINT('',(-1.085235,-0.495,-1.32902956907268E-16));
#24497=CARTESIAN_POINT('Origin',(0.,-0.495,0.));
#24498=CARTESIAN_POINT('Origin',(0.,-0.4575,0.));
#24499=CARTESIAN_POINT('',(-1.085235,-0.4575,-1.32902956907268E-16));
#24500=CARTESIAN_POINT('',(0.,0.,0.));
#24501=CARTESIAN_POINT('',(0.,0.,0.));
#24502=CARTESIAN_POINT('',(0.,0.,0.));
#24503=CARTESIAN_POINT('',(0.,0.,0.));
#24504=CARTESIAN_POINT('',(0.,0.,0.));
#24505=CARTESIAN_POINT('',(0.,0.,0.));
#24506=CARTESIAN_POINT('',(0.,0.,0.));
#24507=CARTESIAN_POINT('Origin',(0.,0.,0.));
#24508=CARTESIAN_POINT('',(-1.63531,-0.410863395882378,-2.00267715711366E-16));
#24509=CARTESIAN_POINT('',(-2.00267715711366E-16,-0.410863395882378,1.63531));
#24510=CARTESIAN_POINT('Origin',(0.,-0.410863395882378,0.));
#24511=CARTESIAN_POINT('Origin',(0.,-0.410863395882378,0.));
#24512=CARTESIAN_POINT('',(-2.00267715711366E-16,0.410863395882378,1.63531));
#24513=CARTESIAN_POINT('Origin',(-2.05128338857182E-16,0.,1.675));
#24514=CARTESIAN_POINT('',(-1.63531,0.410863395882378,2.00267715711366E-16));
#24515=CARTESIAN_POINT('Origin',(0.,0.410863395882378,0.));
#24516=CARTESIAN_POINT('Origin',(0.,0.410863395882378,0.));
#24517=CARTESIAN_POINT('Origin',(0.,0.,0.));
#24518=CARTESIAN_POINT('',(-1.63531,0.7,-2.00267715711366E-16));
#24519=CARTESIAN_POINT('',(-1.63531,0.,-2.00267715711366E-16));
#24520=CARTESIAN_POINT('Origin',(0.,0.7,0.));
#24521=CARTESIAN_POINT('Origin',(0.,0.,0.));
#24522=CARTESIAN_POINT('',(-1.,-0.6,-1.22464679914735E-16));
#24523=CARTESIAN_POINT('Origin',(0.,-0.6,0.));
#24524=CARTESIAN_POINT('',(-1.,0.6,-1.22464679914735E-16));
#24525=CARTESIAN_POINT('',(-1.,0.,-1.22464679914735E-16));
#24526=CARTESIAN_POINT('Origin',(0.,0.6,0.));
#24527=CARTESIAN_POINT('Origin',(0.,0.65,0.));
#24528=CARTESIAN_POINT('',(-1.1,0.7,-1.34711147906209E-16));
#24529=CARTESIAN_POINT('',(-1.05,0.65,-1.28587913910472E-16));
#24530=CARTESIAN_POINT('Origin',(0.,0.7,0.));
#24531=CARTESIAN_POINT('Origin',(1.63531,0.7,0.));
#24532=CARTESIAN_POINT('Origin',(0.,0.,0.));
#24533=CARTESIAN_POINT('',(-1.63531,-0.7,-2.00267715711366E-16));
#24534=CARTESIAN_POINT('Origin',(0.,-0.7,0.));
#24535=CARTESIAN_POINT('',(-1.63531,0.,-2.00267715711366E-16));
#24536=CARTESIAN_POINT('Origin',(1.1,-0.7,0.));
#24537=CARTESIAN_POINT('',(-1.1,-0.7,-1.34711147906209E-16));
#24538=CARTESIAN_POINT('Origin',(0.,-0.7,0.));
#24539=CARTESIAN_POINT('Origin',(0.,-0.65,0.));
#24540=CARTESIAN_POINT('',(-1.05,-0.65,-1.28587913910472E-16));
#24541=CARTESIAN_POINT('',(0.,0.,0.));
#24542=CARTESIAN_POINT('Origin',(0.,0.,0.));
#24543=CARTESIAN_POINT('',(-1.71469,0.410863395882378,-2.09988962002998E-16));
#24544=CARTESIAN_POINT('',(-2.09988962002998E-16,0.410863395882378,1.71469));
#24545=CARTESIAN_POINT('Origin',(0.,0.410863395882378,0.));
#24546=CARTESIAN_POINT('Origin',(0.,0.410863395882378,0.));
#24547=CARTESIAN_POINT('',(-2.09988962002998E-16,-0.410863395882378,1.71469));
#24548=CARTESIAN_POINT('Origin',(-2.05128338857182E-16,0.,1.675));
#24549=CARTESIAN_POINT('',(-1.71469,-0.410863395882378,2.09988962002998E-16));
#24550=CARTESIAN_POINT('Origin',(0.,-0.410863395882378,0.));
#24551=CARTESIAN_POINT('Origin',(0.,-0.410863395882378,0.));
#24552=CARTESIAN_POINT('Origin',(0.,0.,0.));
#24553=CARTESIAN_POINT('',(-1.71469,-0.7,-2.09988962002998E-16));
#24554=CARTESIAN_POINT('Origin',(0.,-0.7,0.));
#24555=CARTESIAN_POINT('',(-1.71469,0.,-2.09988962002998E-16));
#24556=CARTESIAN_POINT('Origin',(2.25,0.7,0.));
#24557=CARTESIAN_POINT('',(-2.25,0.7,-2.75545529808154E-16));
#24558=CARTESIAN_POINT('Origin',(0.,0.7,0.));
#24559=CARTESIAN_POINT('',(-1.71469,0.7,-2.09988962002998E-16));
#24560=CARTESIAN_POINT('Origin',(0.,0.7,0.));
#24561=CARTESIAN_POINT('Origin',(0.,0.65,0.));
#24562=CARTESIAN_POINT('',(-2.35,0.6,-2.87791997799628E-16));
#24563=CARTESIAN_POINT('Origin',(0.,0.6,0.));
#24564=CARTESIAN_POINT('',(-2.3,0.65,-2.81668763803891E-16));
#24565=CARTESIAN_POINT('Origin',(0.,0.,0.));
#24566=CARTESIAN_POINT('',(-2.35,-0.6,-2.87791997799628E-16));
#24567=CARTESIAN_POINT('Origin',(0.,-0.6,0.));
#24568=CARTESIAN_POINT('',(-2.35,0.,-2.87791997799628E-16));
#24569=CARTESIAN_POINT('Origin',(0.,-0.65,0.));
#24570=CARTESIAN_POINT('',(-2.25,-0.7,-2.75545529808154E-16));
#24571=CARTESIAN_POINT('Origin',(0.,-0.7,0.));
#24572=CARTESIAN_POINT('',(-2.3,-0.65,-2.81668763803891E-16));
#24573=CARTESIAN_POINT('Origin',(1.71469,-0.7,0.));
#24574=CARTESIAN_POINT('Origin',(0.,0.,0.));
#24575=CARTESIAN_POINT('',(-1.71469,0.,-2.09988962002998E-16));
#24576=CARTESIAN_POINT('',(0.,0.,0.));
#24577=CARTESIAN_POINT('Origin',(1.675,0.,0.));
#24578=CARTESIAN_POINT('',(1.675,-2.97627328869245E-33,0.3969));
#24579=CARTESIAN_POINT('',(1.675,-2.97627328869245E-33,-0.3969));
#24580=CARTESIAN_POINT('Origin',(1.675,0.,0.));
#24581=CARTESIAN_POINT('Origin',(1.18440385848747,0.,-1.18440385848747));
#24582=CARTESIAN_POINT('',(1.46505453994041,3.1867025333467E-33,-0.903753177034526));
#24583=CARTESIAN_POINT('',(0.903753177034527,-9.13924911073161E-33,-1.46505453994041));
#24584=CARTESIAN_POINT('Origin',(1.18440385848747,0.,-1.18440385848747));
#24585=CARTESIAN_POINT('Origin',(1.02564169428591E-16,0.,-1.675));
#24586=CARTESIAN_POINT('',(0.3969,-2.97627328869246E-33,-1.675));
#24587=CARTESIAN_POINT('',(-0.3969,-2.97627328869245E-33,-1.675));
#24588=CARTESIAN_POINT('Origin',(1.02564169428591E-16,0.,-1.675));
#24589=CARTESIAN_POINT('Origin',(-1.18440385848747,0.,-1.18440385848747));
#24590=CARTESIAN_POINT('',(-0.903753177034526,3.1867025333467E-33,-1.46505453994041));
#24591=CARTESIAN_POINT('',(-1.46505453994041,-9.13924911073161E-33,-0.903753177034527));
#24592=CARTESIAN_POINT('Origin',(-1.18440385848747,0.,-1.18440385848747));
#24593=CARTESIAN_POINT('Origin',(-1.675,0.,-2.05128338857182E-16));
#24594=CARTESIAN_POINT('',(-1.675,-2.97627328869246E-33,-0.3969));
#24595=CARTESIAN_POINT('',(-1.675,-2.97627328869245E-33,0.3969));
#24596=CARTESIAN_POINT('Origin',(-1.675,0.,-2.05128338857182E-16));
#24597=CARTESIAN_POINT('Origin',(-1.18440385848747,0.,1.18440385848747));
#24598=CARTESIAN_POINT('',(-1.46505453994041,6.26819044436628E-33,0.903753177034526));
#24599=CARTESIAN_POINT('',(-0.903753177034527,-1.22207370217512E-32,1.46505453994041));
#24600=CARTESIAN_POINT('Origin',(-1.18440385848747,0.,1.18440385848747));
#24601=CARTESIAN_POINT('Origin',(-3.07692508285772E-16,0.,1.675));
#24602=CARTESIAN_POINT('',(-0.3969,-2.97627328869246E-33,1.675));
#24603=CARTESIAN_POINT('',(0.396899999999999,-2.97627328869245E-33,1.675));
#24604=CARTESIAN_POINT('Origin',(-3.07692508285772E-16,0.,1.675));
#24605=CARTESIAN_POINT('Origin',(1.18440385848747,0.,1.18440385848747));
#24606=CARTESIAN_POINT('',(0.903753177034526,9.34967835538585E-33,1.46505453994041));
#24607=CARTESIAN_POINT('',(1.46505453994041,-1.53022249327708E-32,0.903753177034527));
#24608=CARTESIAN_POINT('Origin',(1.18440385848747,0.,1.18440385848747));
#24609=CARTESIAN_POINT('',(0.,0.,0.));
#24610=CARTESIAN_POINT('Origin',(1.18440385848747,0.,1.18440385848747));
#24611=CARTESIAN_POINT('',(0.846804978391753,-0.07938,1.40825612658882));
#24612=CARTESIAN_POINT('',(1.40825612658882,-0.07938,0.846804978391754));
#24613=CARTESIAN_POINT('Ctrl Pts',(0.846804978391752,-0.0793800000000001,
1.40825612658882));
#24614=CARTESIAN_POINT('Ctrl Pts',(0.854205272175554,-0.123401821157026,
1.40380622184538));
#24615=CARTESIAN_POINT('Ctrl Pts',(0.867957148219441,-0.166543350814306,
1.39550172959303));
#24616=CARTESIAN_POINT('Ctrl Pts',(0.902193646979982,-0.237231147975234,
1.3735491215176));
#24617=CARTESIAN_POINT('Ctrl Pts',(0.920778333482564,-0.266264900654909,
1.36127834356734));
#24618=CARTESIAN_POINT('Ctrl Pts',(0.962485392528369,-0.317195968905306,
1.33211611256184));
#24619=CARTESIAN_POINT('Ctrl Pts',(0.985600426557816,-0.33909093068465,
1.31521005565926));
#24620=CARTESIAN_POINT('Ctrl Pts',(1.03253285680459,-0.373586846396559,
1.27866649102984));
#24621=CARTESIAN_POINT('Ctrl Pts',(1.05871835910697,-0.388086240756494,
1.25722555095714));
#24622=CARTESIAN_POINT('Ctrl Pts',(1.11153475808518,-0.407068917407805,
1.2107812086231));
#24623=CARTESIAN_POINT('Ctrl Pts',(1.13814686046673,-0.411552957311693,
1.18575674747573));
#24624=CARTESIAN_POINT('Ctrl Pts',(1.18575674747573,-0.411552957311693,
1.13814686046673));
#24625=CARTESIAN_POINT('Ctrl Pts',(1.2107812086231,-0.407068917407805,1.11153475808518));
#24626=CARTESIAN_POINT('Ctrl Pts',(1.25722555095713,-0.388086240756494,
1.05871835910697));
#24627=CARTESIAN_POINT('Ctrl Pts',(1.27866649102984,-0.373586846396559,
1.03253285680459));
#24628=CARTESIAN_POINT('Ctrl Pts',(1.31521005565926,-0.33909093068465,0.985600426557816));
#24629=CARTESIAN_POINT('Ctrl Pts',(1.33211611256184,-0.317195968905306,
0.962485392528369));
#24630=CARTESIAN_POINT('Ctrl Pts',(1.36127834356734,-0.266264900654909,
0.920778333482565));
#24631=CARTESIAN_POINT('Ctrl Pts',(1.3735491215176,-0.237231147975234,0.902193646979983));
#24632=CARTESIAN_POINT('Ctrl Pts',(1.39550172959303,-0.166543350814306,
0.867957148219442));
#24633=CARTESIAN_POINT('Ctrl Pts',(1.40380622184538,-0.123401821157026,
0.854205272175555));
#24634=CARTESIAN_POINT('Ctrl Pts',(1.40825612658882,-0.0793800000000001,
0.846804978391753));
#24635=CARTESIAN_POINT('',(0.886256117232623,-0.07938,1.45861320581289));
#24636=CARTESIAN_POINT('Origin',(1.18440385848747,-0.07938,1.18440385848747));
#24637=CARTESIAN_POINT('',(1.45861320581289,-0.07938,0.886256117232624));
#24638=CARTESIAN_POINT('Ctrl Pts',(1.45861320581289,-0.0793800000000001,
0.886256117232623));
#24639=CARTESIAN_POINT('Ctrl Pts',(1.45630208793976,-0.101649918886749,
0.890059788636852));
#24640=CARTESIAN_POINT('Ctrl Pts',(1.45296717977858,-0.123823518623746,
0.895520212222107));
#24641=CARTESIAN_POINT('Ctrl Pts',(1.43904931717599,-0.192480977588836,
0.917859913453975));
#24642=CARTESIAN_POINT('Ctrl Pts',(1.4243271592157,-0.236152929235938,0.940896403863072));
#24643=CARTESIAN_POINT('Ctrl Pts',(1.39055359345152,-0.303141259068212,
0.990027513266106));
#24644=CARTESIAN_POINT('Ctrl Pts',(1.36743459453896,-0.335108247315849,
1.02199477007745));
#24645=CARTESIAN_POINT('Ctrl Pts',(1.32643091652006,-0.373243761060364,
1.07446535104584));
#24646=CARTESIAN_POINT('Ctrl Pts',(1.30441816675528,-0.387888272594439,
1.10126842659597));
#24647=CARTESIAN_POINT('Ctrl Pts',(1.25681160160691,-0.407041111792943,
1.15530234155453));
#24648=CARTESIAN_POINT('Ctrl Pts',(1.23119764287622,-0.411552957311693,
1.18251418313119));
#24649=CARTESIAN_POINT('Ctrl Pts',(1.18251418313119,-0.411552957311693,
1.23119764287622));
#24650=CARTESIAN_POINT('Ctrl Pts',(1.15530234155453,-0.407041111792943,
1.25681160160691));
#24651=CARTESIAN_POINT('Ctrl Pts',(1.10126842659597,-0.387888272594439,
1.30441816675528));
#24652=CARTESIAN_POINT('Ctrl Pts',(1.07446535104584,-0.373243761060364,
1.32643091652006));
#24653=CARTESIAN_POINT('Ctrl Pts',(1.02199477007745,-0.335108247315848,
1.36743459453896));
#24654=CARTESIAN_POINT('Ctrl Pts',(0.990027513266105,-0.303141259068211,
1.39055359345152));
#24655=CARTESIAN_POINT('Ctrl Pts',(0.940896403863071,-0.236152929235937,
1.42432715921571));
#24656=CARTESIAN_POINT('Ctrl Pts',(0.917859913453974,-0.192480977588835,
1.43904931717599));
#24657=CARTESIAN_POINT('Ctrl Pts',(0.895520212222106,-0.123823518623745,
1.45296717977858));
#24658=CARTESIAN_POINT('Ctrl Pts',(0.890059788636851,-0.101649918886749,
1.45630208793976));
#24659=CARTESIAN_POINT('Ctrl Pts',(0.886256117232622,-0.0793800000000001,
1.45861320581289));
#24660=CARTESIAN_POINT('Origin',(1.18440385848747,-0.07938,1.18440385848747));
#24661=CARTESIAN_POINT('Origin',(0.,-0.27783,0.));
#24662=CARTESIAN_POINT('',(0.404717578595295,-0.07938,1.65807299932179));
#24663=CARTESIAN_POINT('Origin',(0.,-0.07938,0.));
#24664=CARTESIAN_POINT('',(-0.404717578595296,-0.07938,1.65807299932179));
#24665=CARTESIAN_POINT('Ctrl Pts',(0.404717578595296,-0.0793800000000001,
1.65807299932179));
#24666=CARTESIAN_POINT('Ctrl Pts',(0.400393769631747,-0.101649918886749,
1.65912839404491));
#24667=CARTESIAN_POINT('Ctrl Pts',(0.394174530911058,-0.123823518623745,
1.66063136041479));
#24668=CARTESIAN_POINT('Ctrl Pts',(0.368536561654407,-0.192480977588835,
1.66658649961961));
#24669=CARTESIAN_POINT('Ctrl Pts',(0.341837165343982,-0.236152929235937,
1.67246562047521));
#24670=CARTESIAN_POINT('Ctrl Pts',(0.283214707341173,-0.303141259068211,
1.68332504372461));
#24671=CARTESIAN_POINT('Ctrl Pts',(0.244262842368623,-0.335108247315849,
1.68958170688653));
#24672=CARTESIAN_POINT('Ctrl Pts',(0.178166559972324,-0.373243761060364,
1.69769003172132));
#24673=CARTESIAN_POINT('Ctrl Pts',(0.143648558862931,-0.387888272594439,
1.70107730356824));
#24674=CARTESIAN_POINT('Ctrl Pts',(0.0717778861362652,-0.407041111792943,
1.70562212620408));
#24675=CARTESIAN_POINT('Ctrl Pts',(0.0344244045173309,-0.411552957311693,
1.706752));
#24676=CARTESIAN_POINT('Ctrl Pts',(-0.0344244045173315,-0.411552957311693,
1.706752));
#24677=CARTESIAN_POINT('Ctrl Pts',(-0.0717778861362658,-0.407041111792943,
1.70562212620408));
#24678=CARTESIAN_POINT('Ctrl Pts',(-0.143648558862932,-0.387888272594439,
1.70107730356824));
#24679=CARTESIAN_POINT('Ctrl Pts',(-0.178166559972325,-0.373243761060364,
1.69769003172132));
#24680=CARTESIAN_POINT('Ctrl Pts',(-0.244262842368624,-0.335108247315849,
1.68958170688653));
#24681=CARTESIAN_POINT('Ctrl Pts',(-0.283214707341173,-0.303141259068212,
1.68332504372461));
#24682=CARTESIAN_POINT('Ctrl Pts',(-0.341837165343982,-0.236152929235937,
1.67246562047521));
#24683=CARTESIAN_POINT('Ctrl Pts',(-0.368536561654408,-0.192480977588835,
1.66658649961961));
#24684=CARTESIAN_POINT('Ctrl Pts',(-0.394174530911059,-0.123823518623745,
1.66063136041479));
#24685=CARTESIAN_POINT('Ctrl Pts',(-0.400393769631748,-0.101649918886749,
1.65912839404491));
#24686=CARTESIAN_POINT('Ctrl Pts',(-0.404717578595297,-0.0793800000000001,
1.65807299932179));
#24687=CARTESIAN_POINT('',(-0.886256117232624,-0.07938,1.45861320581289));
#24688=CARTESIAN_POINT('Origin',(0.,-0.07938,0.));
#24689=CARTESIAN_POINT('',(-1.45861320581289,-0.07938,0.886256117232623));
#24690=CARTESIAN_POINT('Ctrl Pts',(-0.886256117232623,-0.0793800000000001,
1.45861320581289));
#24691=CARTESIAN_POINT('Ctrl Pts',(-0.890059788636852,-0.101649918886749,
1.45630208793976));
#24692=CARTESIAN_POINT('Ctrl Pts',(-0.895520212222106,-0.123823518623745,
1.45296717977858));
#24693=CARTESIAN_POINT('Ctrl Pts',(-0.917859913453974,-0.192480977588835,
1.43904931717599));
#24694=CARTESIAN_POINT('Ctrl Pts',(-0.940896403863071,-0.236152929235937,
1.4243271592157));
#24695=CARTESIAN_POINT('Ctrl Pts',(-0.990027513266105,-0.303141259068211,
1.39055359345152));
#24696=CARTESIAN_POINT('Ctrl Pts',(-1.02199477007745,-0.335108247315848,
1.36743459453896));
#24697=CARTESIAN_POINT('Ctrl Pts',(-1.07446535104584,-0.373243761060364,
1.32643091652006));
#24698=CARTESIAN_POINT('Ctrl Pts',(-1.10126842659597,-0.387888272594439,
1.30441816675528));
#24699=CARTESIAN_POINT('Ctrl Pts',(-1.15530234155453,-0.407041111792943,
1.25681160160691));
#24700=CARTESIAN_POINT('Ctrl Pts',(-1.18251418313119,-0.411552957311693,
1.23119764287622));
#24701=CARTESIAN_POINT('Ctrl Pts',(-1.23119764287622,-0.411552957311693,
1.18251418313119));
#24702=CARTESIAN_POINT('Ctrl Pts',(-1.25681160160691,-0.407041111792943,
1.15530234155453));
#24703=CARTESIAN_POINT('Ctrl Pts',(-1.30441816675528,-0.387888272594439,
1.10126842659597));
#24704=CARTESIAN_POINT('Ctrl Pts',(-1.32643091652006,-0.373243761060365,
1.07446535104584));
#24705=CARTESIAN_POINT('Ctrl Pts',(-1.36743459453896,-0.335108247315849,
1.02199477007745));
#24706=CARTESIAN_POINT('Ctrl Pts',(-1.39055359345152,-0.303141259068212,
0.990027513266106));
#24707=CARTESIAN_POINT('Ctrl Pts',(-1.4243271592157,-0.236152929235938,
0.940896403863071));
#24708=CARTESIAN_POINT('Ctrl Pts',(-1.43904931717599,-0.192480977588836,
0.917859913453974));
#24709=CARTESIAN_POINT('Ctrl Pts',(-1.45296717977858,-0.123823518623746,
0.895520212222106));
#24710=CARTESIAN_POINT('Ctrl Pts',(-1.45630208793976,-0.101649918886749,
0.890059788636852));
#24711=CARTESIAN_POINT('Ctrl Pts',(-1.45861320581289,-0.0793800000000001,
0.886256117232623));
#24712=CARTESIAN_POINT('',(-1.65807299932179,-0.07938,0.404717578595295));
#24713=CARTESIAN_POINT('Origin',(0.,-0.07938,0.));
#24714=CARTESIAN_POINT('',(-1.706752,-0.411552957311693,2.08591827245526E-16));
#24715=CARTESIAN_POINT('Ctrl Pts',(-1.65807299932179,-0.0793800000000001,
0.404717578595296));
#24716=CARTESIAN_POINT('Ctrl Pts',(-1.65912839404491,-0.101649918886749,
0.400393769631747));
#24717=CARTESIAN_POINT('Ctrl Pts',(-1.66063136041479,-0.123823518623745,
0.394174530911058));
#24718=CARTESIAN_POINT('Ctrl Pts',(-1.66658649961961,-0.192480977588835,
0.368536561654407));
#24719=CARTESIAN_POINT('Ctrl Pts',(-1.67246562047521,-0.236152929235937,
0.341837165343982));
#24720=CARTESIAN_POINT('Ctrl Pts',(-1.68332504372461,-0.303141259068211,
0.283214707341173));
#24721=CARTESIAN_POINT('Ctrl Pts',(-1.68958170688653,-0.335108247315848,
0.244262842368623));
#24722=CARTESIAN_POINT('Ctrl Pts',(-1.69769003172132,-0.373243761060364,
0.178166559972324));
#24723=CARTESIAN_POINT('Ctrl Pts',(-1.70107730356824,-0.387888272594439,
0.143648558862931));
#24724=CARTESIAN_POINT('Ctrl Pts',(-1.70562212620408,-0.407041111792943,
0.0717778861362656));
#24725=CARTESIAN_POINT('Ctrl Pts',(-1.706752,-0.411552957311693,0.0344244045173313));
#24726=CARTESIAN_POINT('Ctrl Pts',(-1.706752,-0.411552957311693,2.08166817117217E-16));
#24727=CARTESIAN_POINT('',(-1.706752,-0.47628,2.09016837373834E-16));
#24728=CARTESIAN_POINT('',(-1.706752,-0.27783,2.09016837373834E-16));
#24729=CARTESIAN_POINT('Origin',(0.,-0.47628,0.));
#24730=CARTESIAN_POINT('',(-1.65807299932179,-0.07938,-0.404717578595296));
#24731=CARTESIAN_POINT('Ctrl Pts',(-1.706752,-0.411552957311693,2.0122792321331E-16));
#24732=CARTESIAN_POINT('Ctrl Pts',(-1.706752,-0.411552957311693,-0.0344244045173309));
#24733=CARTESIAN_POINT('Ctrl Pts',(-1.70562212620408,-0.407041111792943,
-0.0717778861362652));
#24734=CARTESIAN_POINT('Ctrl Pts',(-1.70107730356824,-0.387888272594439,
-0.143648558862931));
#24735=CARTESIAN_POINT('Ctrl Pts',(-1.69769003172132,-0.373243761060365,
-0.178166559972324));
#24736=CARTESIAN_POINT('Ctrl Pts',(-1.68958170688653,-0.335108247315849,
-0.244262842368623));
#24737=CARTESIAN_POINT('Ctrl Pts',(-1.68332504372461,-0.303141259068212,
-0.283214707341173));
#24738=CARTESIAN_POINT('Ctrl Pts',(-1.67246562047521,-0.236152929235938,
-0.341837165343982));
#24739=CARTESIAN_POINT('Ctrl Pts',(-1.66658649961961,-0.192480977588836,
-0.368536561654407));
#24740=CARTESIAN_POINT('Ctrl Pts',(-1.66063136041479,-0.123823518623745,
-0.394174530911059));
#24741=CARTESIAN_POINT('Ctrl Pts',(-1.65912839404491,-0.101649918886749,
-0.400393769631748));
#24742=CARTESIAN_POINT('Ctrl Pts',(-1.65807299932179,-0.0793800000000001,
-0.404717578595296));
#24743=CARTESIAN_POINT('',(-1.45861320581289,-0.07938,-0.886256117232623));
#24744=CARTESIAN_POINT('Origin',(0.,-0.07938,0.));
#24745=CARTESIAN_POINT('',(-0.886256117232623,-0.07938,-1.45861320581289));
#24746=CARTESIAN_POINT('Ctrl Pts',(-1.45861320581289,-0.0793800000000001,
-0.886256117232623));
#24747=CARTESIAN_POINT('Ctrl Pts',(-1.45630208793976,-0.101649918886749,
-0.890059788636852));
#24748=CARTESIAN_POINT('Ctrl Pts',(-1.45296717977858,-0.123823518623745,
-0.895520212222106));
#24749=CARTESIAN_POINT('Ctrl Pts',(-1.43904931717599,-0.192480977588835,
-0.917859913453974));
#24750=CARTESIAN_POINT('Ctrl Pts',(-1.4243271592157,-0.236152929235937,
-0.940896403863072));
#24751=CARTESIAN_POINT('Ctrl Pts',(-1.39055359345152,-0.303141259068212,
-0.990027513266106));
#24752=CARTESIAN_POINT('Ctrl Pts',(-1.36743459453896,-0.335108247315849,
-1.02199477007745));
#24753=CARTESIAN_POINT('Ctrl Pts',(-1.32643091652006,-0.373243761060364,
-1.07446535104584));
#24754=CARTESIAN_POINT('Ctrl Pts',(-1.30441816675528,-0.387888272594439,
-1.10126842659597));
#24755=CARTESIAN_POINT('Ctrl Pts',(-1.25681160160691,-0.407041111792943,
-1.15530234155453));
#24756=CARTESIAN_POINT('Ctrl Pts',(-1.23119764287622,-0.411552957311693,
-1.18251418313119));
#24757=CARTESIAN_POINT('Ctrl Pts',(-1.18251418313119,-0.411552957311693,
-1.23119764287622));
#24758=CARTESIAN_POINT('Ctrl Pts',(-1.15530234155453,-0.407041111792943,
-1.25681160160691));
#24759=CARTESIAN_POINT('Ctrl Pts',(-1.10126842659597,-0.387888272594439,
-1.30441816675528));
#24760=CARTESIAN_POINT('Ctrl Pts',(-1.07446535104584,-0.373243761060364,
-1.32643091652006));
#24761=CARTESIAN_POINT('Ctrl Pts',(-1.02199477007745,-0.335108247315848,
-1.36743459453896));
#24762=CARTESIAN_POINT('Ctrl Pts',(-0.990027513266105,-0.303141259068211,
-1.39055359345152));
#24763=CARTESIAN_POINT('Ctrl Pts',(-0.940896403863071,-0.236152929235936,
-1.42432715921571));
#24764=CARTESIAN_POINT('Ctrl Pts',(-0.917859913453974,-0.192480977588835,
-1.43904931717599));
#24765=CARTESIAN_POINT('Ctrl Pts',(-0.895520212222106,-0.123823518623745,
-1.45296717977858));
#24766=CARTESIAN_POINT('Ctrl Pts',(-0.890059788636851,-0.101649918886749,
-1.45630208793976));
#24767=CARTESIAN_POINT('Ctrl Pts',(-0.886256117232623,-0.0793800000000001,
-1.45861320581289));
#24768=CARTESIAN_POINT('',(-0.404717578595295,-0.07938,-1.65807299932179));
#24769=CARTESIAN_POINT('Origin',(0.,-0.07938,0.));
#24770=CARTESIAN_POINT('',(0.404717578595296,-0.07938,-1.65807299932179));
#24771=CARTESIAN_POINT('Ctrl Pts',(-0.404717578595296,-0.0793800000000001,
-1.65807299932179));
#24772=CARTESIAN_POINT('Ctrl Pts',(-0.400393769631747,-0.101649918886749,
-1.65912839404491));
#24773=CARTESIAN_POINT('Ctrl Pts',(-0.394174530911058,-0.123823518623746,
-1.66063136041479));
#24774=CARTESIAN_POINT('Ctrl Pts',(-0.368536561654407,-0.192480977588836,
-1.66658649961961));
#24775=CARTESIAN_POINT('Ctrl Pts',(-0.341837165343982,-0.236152929235938,
-1.67246562047521));
#24776=CARTESIAN_POINT('Ctrl Pts',(-0.283214707341173,-0.303141259068212,
-1.68332504372461));
#24777=CARTESIAN_POINT('Ctrl Pts',(-0.244262842368623,-0.335108247315849,
-1.68958170688653));
#24778=CARTESIAN_POINT('Ctrl Pts',(-0.178166559972324,-0.373243761060364,
-1.69769003172132));
#24779=CARTESIAN_POINT('Ctrl Pts',(-0.143648558862931,-0.387888272594439,
-1.70107730356824));
#24780=CARTESIAN_POINT('Ctrl Pts',(-0.0717778861362653,-0.407041111792943,
-1.70562212620408));
#24781=CARTESIAN_POINT('Ctrl Pts',(-0.034424404517331,-0.411552957311693,
-1.706752));
#24782=CARTESIAN_POINT('Ctrl Pts',(0.0344244045173312,-0.411552957311693,
-1.706752));
#24783=CARTESIAN_POINT('Ctrl Pts',(0.0717778861362655,-0.407041111792943,
-1.70562212620408));
#24784=CARTESIAN_POINT('Ctrl Pts',(0.143648558862931,-0.387888272594439,
-1.70107730356824));
#24785=CARTESIAN_POINT('Ctrl Pts',(0.178166559972324,-0.373243761060364,
-1.69769003172132));
#24786=CARTESIAN_POINT('Ctrl Pts',(0.244262842368623,-0.335108247315849,
-1.68958170688653));
#24787=CARTESIAN_POINT('Ctrl Pts',(0.283214707341173,-0.303141259068212,
-1.68332504372461));
#24788=CARTESIAN_POINT('Ctrl Pts',(0.341837165343982,-0.236152929235937,
-1.67246562047521));
#24789=CARTESIAN_POINT('Ctrl Pts',(0.368536561654407,-0.192480977588835,
-1.66658649961961));
#24790=CARTESIAN_POINT('Ctrl Pts',(0.394174530911059,-0.123823518623745,
-1.66063136041479));
#24791=CARTESIAN_POINT('Ctrl Pts',(0.400393769631748,-0.101649918886749,
-1.65912839404491));
#24792=CARTESIAN_POINT('Ctrl Pts',(0.404717578595296,-0.0793800000000001,
-1.65807299932179));
#24793=CARTESIAN_POINT('',(0.886256117232623,-0.07938,-1.45861320581289));
#24794=CARTESIAN_POINT('Origin',(0.,-0.07938,0.));
#24795=CARTESIAN_POINT('',(1.45861320581289,-0.07938,-0.886256117232623));
#24796=CARTESIAN_POINT('Ctrl Pts',(0.886256117232623,-0.0793800000000001,
-1.45861320581289));
#24797=CARTESIAN_POINT('Ctrl Pts',(0.890059788636852,-0.101649918886749,
-1.45630208793976));
#24798=CARTESIAN_POINT('Ctrl Pts',(0.895520212222106,-0.123823518623745,
-1.45296717977858));
#24799=CARTESIAN_POINT('Ctrl Pts',(0.917859913453974,-0.192480977588835,
-1.43904931717599));
#24800=CARTESIAN_POINT('Ctrl Pts',(0.940896403863072,-0.236152929235937,
-1.4243271592157));
#24801=CARTESIAN_POINT('Ctrl Pts',(0.990027513266106,-0.303141259068211,
-1.39055359345152));
#24802=CARTESIAN_POINT('Ctrl Pts',(1.02199477007745,-0.335108247315849,
-1.36743459453896));
#24803=CARTESIAN_POINT('Ctrl Pts',(1.07446535104584,-0.373243761060364,
-1.32643091652006));
#24804=CARTESIAN_POINT('Ctrl Pts',(1.10126842659597,-0.387888272594439,
-1.30441816675528));
#24805=CARTESIAN_POINT('Ctrl Pts',(1.15530234155453,-0.407041111792943,
-1.25681160160691));
#24806=CARTESIAN_POINT('Ctrl Pts',(1.18251418313119,-0.411552957311693,
-1.23119764287622));
#24807=CARTESIAN_POINT('Ctrl Pts',(1.23119764287622,-0.411552957311693,
-1.18251418313119));
#24808=CARTESIAN_POINT('Ctrl Pts',(1.25681160160691,-0.407041111792943,
-1.15530234155453));
#24809=CARTESIAN_POINT('Ctrl Pts',(1.30441816675528,-0.387888272594439,
-1.10126842659597));
#24810=CARTESIAN_POINT('Ctrl Pts',(1.32643091652006,-0.373243761060364,
-1.07446535104584));
#24811=CARTESIAN_POINT('Ctrl Pts',(1.36743459453896,-0.335108247315849,
-1.02199477007745));
#24812=CARTESIAN_POINT('Ctrl Pts',(1.39055359345152,-0.303141259068212,
-0.990027513266105));
#24813=CARTESIAN_POINT('Ctrl Pts',(1.4243271592157,-0.236152929235937,-0.940896403863071));
#24814=CARTESIAN_POINT('Ctrl Pts',(1.43904931717599,-0.192480977588835,
-0.917859913453974));
#24815=CARTESIAN_POINT('Ctrl Pts',(1.45296717977858,-0.123823518623745,
-0.895520212222106));
#24816=CARTESIAN_POINT('Ctrl Pts',(1.45630208793976,-0.101649918886749,
-0.890059788636852));
#24817=CARTESIAN_POINT('Ctrl Pts',(1.45861320581289,-0.0793800000000001,
-0.886256117232623));
#24818=CARTESIAN_POINT('',(1.65807299932179,-0.07938,-0.404717578595296));
#24819=CARTESIAN_POINT('Origin',(0.,-0.07938,0.));
#24820=CARTESIAN_POINT('',(1.65807299932179,-0.07938,0.404717578595296));
#24821=CARTESIAN_POINT('Ctrl Pts',(1.65807299932179,-0.0793800000000001,
-0.404717578595296));
#24822=CARTESIAN_POINT('Ctrl Pts',(1.65912839404491,-0.101649918886749,
-0.400393769631747));
#24823=CARTESIAN_POINT('Ctrl Pts',(1.66063136041479,-0.123823518623745,
-0.394174530911058));
#24824=CARTESIAN_POINT('Ctrl Pts',(1.66658649961961,-0.192480977588835,
-0.368536561654407));
#24825=CARTESIAN_POINT('Ctrl Pts',(1.67246562047521,-0.236152929235937,
-0.341837165343982));
#24826=CARTESIAN_POINT('Ctrl Pts',(1.68332504372461,-0.303141259068212,
-0.283214707341173));
#24827=CARTESIAN_POINT('Ctrl Pts',(1.68958170688653,-0.335108247315849,
-0.244262842368623));
#24828=CARTESIAN_POINT('Ctrl Pts',(1.69769003172132,-0.373243761060364,
-0.178166559972324));
#24829=CARTESIAN_POINT('Ctrl Pts',(1.70107730356824,-0.387888272594439,
-0.143648558862931));
#24830=CARTESIAN_POINT('Ctrl Pts',(1.70562212620408,-0.407041111792943,
-0.0717778861362655));
#24831=CARTESIAN_POINT('Ctrl Pts',(1.706752,-0.411552957311693,-0.0344244045173312));
#24832=CARTESIAN_POINT('Ctrl Pts',(1.706752,-0.411552957311693,0.0344244045173312));
#24833=CARTESIAN_POINT('Ctrl Pts',(1.70562212620408,-0.407041111792943,
0.0717778861362655));
#24834=CARTESIAN_POINT('Ctrl Pts',(1.70107730356824,-0.387888272594439,
0.143648558862931));
#24835=CARTESIAN_POINT('Ctrl Pts',(1.69769003172132,-0.373243761060364,
0.178166559972324));
#24836=CARTESIAN_POINT('Ctrl Pts',(1.68958170688653,-0.335108247315849,
0.244262842368623));
#24837=CARTESIAN_POINT('Ctrl Pts',(1.68332504372461,-0.303141259068212,
0.283214707341173));
#24838=CARTESIAN_POINT('Ctrl Pts',(1.67246562047521,-0.236152929235937,
0.341837165343982));
#24839=CARTESIAN_POINT('Ctrl Pts',(1.66658649961961,-0.192480977588835,
0.368536561654407));
#24840=CARTESIAN_POINT('Ctrl Pts',(1.66063136041479,-0.123823518623745,
0.394174530911058));
#24841=CARTESIAN_POINT('Ctrl Pts',(1.65912839404491,-0.101649918886749,
0.400393769631747));
#24842=CARTESIAN_POINT('Ctrl Pts',(1.65807299932179,-0.0793800000000001,
0.404717578595296));
#24843=CARTESIAN_POINT('Origin',(0.,-0.07938,0.));
#24844=CARTESIAN_POINT('Origin',(0.,-0.07938,0.));
#24845=CARTESIAN_POINT('',(0.397005914195118,-0.07938,1.59456899932179));
#24846=CARTESIAN_POINT('Origin',(0.,-0.07938,0.));
#24847=CARTESIAN_POINT('Origin',(-3.33066907387547E-16,-0.07938,1.675));
#24848=CARTESIAN_POINT('Origin',(-3.33066907387547E-16,0.,1.675));
#24849=CARTESIAN_POINT('',(-0.397005914195118,-0.07938,1.59456899932179));
#24850=CARTESIAN_POINT('Ctrl Pts',(-0.397005914195119,-0.0793800000000001,
1.59456899932179));
#24851=CARTESIAN_POINT('Ctrl Pts',(-0.3886265584581,-0.123401821157026,
1.59665523941937));
#24852=CARTESIAN_POINT('Ctrl Pts',(-0.373030350867485,-0.166543350814306,
1.60050712143809));
#24853=CARTESIAN_POINT('Ctrl Pts',(-0.333298652394954,-0.237231147975234,
1.60919314384089));
#24854=CARTESIAN_POINT('Ctrl Pts',(-0.311480544243687,-0.266264900654909,
1.61365775139403));
#24855=CARTESIAN_POINT('Ctrl Pts',(-0.261368388670537,-0.317195968905306,
1.62252828437015));
#24856=CARTESIAN_POINT('Ctrl Pts',(-0.233069203882014,-0.33909093068465,
1.62691869420078));
#24857=CARTESIAN_POINT('Ctrl Pts',(-0.174042761838764,-0.373586846396559,
1.63426473152765));
#24858=CARTESIAN_POINT('Ctrl Pts',(-0.14036578147155,-0.388086240756494,
1.63761964365402));
#24859=CARTESIAN_POINT('Ctrl Pts',(-0.0701778381840615,-0.407068917407805,
1.64212536811722));
#24860=CARTESIAN_POINT('Ctrl Pts',(-0.0336652739555918,-0.411552957311693,
1.643248));
#24861=CARTESIAN_POINT('Ctrl Pts',(0.0336652739555913,-0.411552957311693,
1.643248));
#24862=CARTESIAN_POINT('Ctrl Pts',(0.070177838184061,-0.407068917407805,
1.64212536811722));
#24863=CARTESIAN_POINT('Ctrl Pts',(0.140365781471549,-0.388086240756494,
1.63761964365402));
#24864=CARTESIAN_POINT('Ctrl Pts',(0.174042761838763,-0.373586846396559,
1.63426473152765));
#24865=CARTESIAN_POINT('Ctrl Pts',(0.233069203882014,-0.33909093068465,
1.62691869420078));
#24866=CARTESIAN_POINT('Ctrl Pts',(0.261368388670536,-0.317195968905306,
1.62252828437015));
#24867=CARTESIAN_POINT('Ctrl Pts',(0.311480544243686,-0.266264900654908,
1.61365775139403));
#24868=CARTESIAN_POINT('Ctrl Pts',(0.333298652394954,-0.237231147975234,
1.60919314384089));
#24869=CARTESIAN_POINT('Ctrl Pts',(0.373030350867484,-0.166543350814306,
1.60050712143809));
#24870=CARTESIAN_POINT('Ctrl Pts',(0.388626558458099,-0.123401821157026,
1.59665523941937));
#24871=CARTESIAN_POINT('Ctrl Pts',(0.397005914195118,-0.07938,1.59456899932179));
#24872=CARTESIAN_POINT('Origin',(-3.33066907387547E-16,-0.07938,1.675));
#24873=CARTESIAN_POINT('Origin',(0.,-0.07938,0.));
#24874=CARTESIAN_POINT('',(-0.846804978391754,-0.07938,1.40825612658882));
#24875=CARTESIAN_POINT('Origin',(0.,-0.07938,0.));
#24876=CARTESIAN_POINT('Origin',(-1.18440385848747,-0.07938,1.18440385848747));
#24877=CARTESIAN_POINT('Origin',(-1.18440385848747,0.,1.18440385848747));
#24878=CARTESIAN_POINT('',(-1.40825612658882,-0.07938,0.846804978391753));
#24879=CARTESIAN_POINT('Ctrl Pts',(-1.40825612658882,-0.0793800000000001,
0.846804978391753));
#24880=CARTESIAN_POINT('Ctrl Pts',(-1.40380622184538,-0.123401821157026,
0.854205272175555));
#24881=CARTESIAN_POINT('Ctrl Pts',(-1.39550172959303,-0.166543350814306,
0.867957148219442));
#24882=CARTESIAN_POINT('Ctrl Pts',(-1.3735491215176,-0.237231147975235,
0.902193646979983));
#24883=CARTESIAN_POINT('Ctrl Pts',(-1.36127834356734,-0.266264900654909,
0.920778333482565));
#24884=CARTESIAN_POINT('Ctrl Pts',(-1.33211611256184,-0.317195968905306,
0.962485392528369));
#24885=CARTESIAN_POINT('Ctrl Pts',(-1.31521005565926,-0.339090930684651,
0.985600426557816));
#24886=CARTESIAN_POINT('Ctrl Pts',(-1.27866649102984,-0.373586846396559,
1.03253285680459));
#24887=CARTESIAN_POINT('Ctrl Pts',(-1.25722555095714,-0.388086240756494,
1.05871835910697));
#24888=CARTESIAN_POINT('Ctrl Pts',(-1.2107812086231,-0.407068917407805,
1.11153475808518));
#24889=CARTESIAN_POINT('Ctrl Pts',(-1.18575674747573,-0.411552957311693,
1.13814686046673));
#24890=CARTESIAN_POINT('Ctrl Pts',(-1.13814686046673,-0.411552957311693,
1.18575674747573));
#24891=CARTESIAN_POINT('Ctrl Pts',(-1.11153475808518,-0.407068917407805,
1.2107812086231));
#24892=CARTESIAN_POINT('Ctrl Pts',(-1.05871835910697,-0.388086240756494,
1.25722555095714));
#24893=CARTESIAN_POINT('Ctrl Pts',(-1.03253285680459,-0.373586846396559,
1.27866649102984));
#24894=CARTESIAN_POINT('Ctrl Pts',(-0.985600426557816,-0.33909093068465,
1.31521005565926));
#24895=CARTESIAN_POINT('Ctrl Pts',(-0.962485392528369,-0.317195968905306,
1.33211611256184));
#24896=CARTESIAN_POINT('Ctrl Pts',(-0.920778333482565,-0.266264900654908,
1.36127834356734));
#24897=CARTESIAN_POINT('Ctrl Pts',(-0.902193646979983,-0.237231147975234,
1.3735491215176));
#24898=CARTESIAN_POINT('Ctrl Pts',(-0.867957148219442,-0.166543350814306,
1.39550172959303));
#24899=CARTESIAN_POINT('Ctrl Pts',(-0.854205272175555,-0.123401821157026,
1.40380622184538));
#24900=CARTESIAN_POINT('Ctrl Pts',(-0.846804978391753,-0.0793800000000001,
1.40825612658882));
#24901=CARTESIAN_POINT('Origin',(-1.18440385848747,-0.07938,1.18440385848747));
#24902=CARTESIAN_POINT('Origin',(0.,-0.07938,0.));
#24903=CARTESIAN_POINT('',(-1.59456899932179,-0.07938,0.397005914195118));
#24904=CARTESIAN_POINT('Origin',(0.,-0.07938,0.));
#24905=CARTESIAN_POINT('Origin',(-1.675,-0.07938,-2.22044604925031E-16));
#24906=CARTESIAN_POINT('Origin',(-1.675,0.,-2.22044604925031E-16));
#24907=CARTESIAN_POINT('',(-1.59456899932179,-0.07938,-0.397005914195118));
#24908=CARTESIAN_POINT('',(-1.643248,-0.411552957311693,3.47540551556327E-18));
#24909=CARTESIAN_POINT('Ctrl Pts',(-1.59456899932179,-0.0793800000000001,
-0.397005914195119));
#24910=CARTESIAN_POINT('Ctrl Pts',(-1.59665523941937,-0.123401821157026,
-0.388626558458099));
#24911=CARTESIAN_POINT('Ctrl Pts',(-1.60050712143809,-0.166543350814306,
-0.373030350867485));
#24912=CARTESIAN_POINT('Ctrl Pts',(-1.60919314384089,-0.237231147975234,
-0.333298652394954));
#24913=CARTESIAN_POINT('Ctrl Pts',(-1.61365775139403,-0.266264900654909,
-0.311480544243686));
#24914=CARTESIAN_POINT('Ctrl Pts',(-1.62252828437015,-0.317195968905306,
-0.261368388670537));
#24915=CARTESIAN_POINT('Ctrl Pts',(-1.62691869420078,-0.33909093068465,
-0.233069203882014));
#24916=CARTESIAN_POINT('Ctrl Pts',(-1.63426473152765,-0.373586846396559,
-0.174042761838764));
#24917=CARTESIAN_POINT('Ctrl Pts',(-1.63761964365402,-0.388086240756494,
-0.140365781471549));
#24918=CARTESIAN_POINT('Ctrl Pts',(-1.64212536811722,-0.407068917407805,
-0.0701778381840614));
#24919=CARTESIAN_POINT('Ctrl Pts',(-1.643248,-0.411552957311693,-0.0336652739555917));
#24920=CARTESIAN_POINT('Ctrl Pts',(-1.643248,-0.411552957311693,-2.0122792321331E-16));
#24921=CARTESIAN_POINT('Origin',(-1.675,-0.07938,-2.22044604925031E-16));
#24922=CARTESIAN_POINT('Ctrl Pts',(-1.643248,-0.411552957311693,-1.94289029309402E-16));
#24923=CARTESIAN_POINT('Ctrl Pts',(-1.643248,-0.411552957311693,0.0336652739555913));
#24924=CARTESIAN_POINT('Ctrl Pts',(-1.64212536811722,-0.407068917407805,
0.0701778381840609));
#24925=CARTESIAN_POINT('Ctrl Pts',(-1.63761964365402,-0.388086240756494,
0.140365781471549));
#24926=CARTESIAN_POINT('Ctrl Pts',(-1.63426473152765,-0.373586846396559,
0.174042761838763));
#24927=CARTESIAN_POINT('Ctrl Pts',(-1.62691869420078,-0.33909093068465,
0.233069203882014));
#24928=CARTESIAN_POINT('Ctrl Pts',(-1.62252828437015,-0.317195968905306,
0.261368388670536));
#24929=CARTESIAN_POINT('Ctrl Pts',(-1.61365775139403,-0.266264900654909,
0.311480544243686));
#24930=CARTESIAN_POINT('Ctrl Pts',(-1.60919314384089,-0.237231147975235,
0.333298652394954));
#24931=CARTESIAN_POINT('Ctrl Pts',(-1.60050712143809,-0.166543350814306,
0.373030350867484));
#24932=CARTESIAN_POINT('Ctrl Pts',(-1.59665523941937,-0.123401821157026,
0.388626558458099));
#24933=CARTESIAN_POINT('Ctrl Pts',(-1.59456899932179,-0.0793800000000001,
0.397005914195118));
#24934=CARTESIAN_POINT('Origin',(0.,-0.07938,0.));
#24935=CARTESIAN_POINT('',(-1.40825612658882,-0.07938,-0.846804978391753));
#24936=CARTESIAN_POINT('Origin',(0.,-0.07938,0.));
#24937=CARTESIAN_POINT('Origin',(-1.18440385848747,-0.07938,-1.18440385848747));
#24938=CARTESIAN_POINT('Origin',(-1.18440385848747,0.,-1.18440385848747));
#24939=CARTESIAN_POINT('',(-0.846804978391753,-0.07938,-1.40825612658882));
#24940=CARTESIAN_POINT('Ctrl Pts',(-0.846804978391753,-0.0793800000000001,
-1.40825612658882));
#24941=CARTESIAN_POINT('Ctrl Pts',(-0.854205272175555,-0.123401821157026,
-1.40380622184538));
#24942=CARTESIAN_POINT('Ctrl Pts',(-0.867957148219442,-0.166543350814306,
-1.39550172959303));
#24943=CARTESIAN_POINT('Ctrl Pts',(-0.902193646979982,-0.237231147975234,
-1.3735491215176));
#24944=CARTESIAN_POINT('Ctrl Pts',(-0.920778333482564,-0.266264900654908,
-1.36127834356734));
#24945=CARTESIAN_POINT('Ctrl Pts',(-0.962485392528368,-0.317195968905306,
-1.33211611256184));
#24946=CARTESIAN_POINT('Ctrl Pts',(-0.985600426557816,-0.33909093068465,
-1.31521005565926));
#24947=CARTESIAN_POINT('Ctrl Pts',(-1.03253285680459,-0.373586846396559,
-1.27866649102984));
#24948=CARTESIAN_POINT('Ctrl Pts',(-1.05871835910697,-0.388086240756494,
-1.25722555095714));
#24949=CARTESIAN_POINT('Ctrl Pts',(-1.11153475808518,-0.407068917407805,
-1.2107812086231));
#24950=CARTESIAN_POINT('Ctrl Pts',(-1.13814686046673,-0.411552957311693,
-1.18575674747573));
#24951=CARTESIAN_POINT('Ctrl Pts',(-1.18575674747573,-0.411552957311693,
-1.13814686046673));
#24952=CARTESIAN_POINT('Ctrl Pts',(-1.2107812086231,-0.407068917407805,
-1.11153475808518));
#24953=CARTESIAN_POINT('Ctrl Pts',(-1.25722555095714,-0.388086240756494,
-1.05871835910697));
#24954=CARTESIAN_POINT('Ctrl Pts',(-1.27866649102984,-0.373586846396559,
-1.03253285680459));
#24955=CARTESIAN_POINT('Ctrl Pts',(-1.31521005565926,-0.33909093068465,
-0.985600426557816));
#24956=CARTESIAN_POINT('Ctrl Pts',(-1.33211611256184,-0.317195968905306,
-0.962485392528369));
#24957=CARTESIAN_POINT('Ctrl Pts',(-1.36127834356734,-0.266264900654909,
-0.920778333482565));
#24958=CARTESIAN_POINT('Ctrl Pts',(-1.3735491215176,-0.237231147975234,
-0.902193646979983));
#24959=CARTESIAN_POINT('Ctrl Pts',(-1.39550172959303,-0.166543350814306,
-0.867957148219442));
#24960=CARTESIAN_POINT('Ctrl Pts',(-1.40380622184538,-0.123401821157026,
-0.854205272175555));
#24961=CARTESIAN_POINT('Ctrl Pts',(-1.40825612658882,-0.07938,-0.846804978391753));
#24962=CARTESIAN_POINT('Origin',(-1.18440385848747,-0.07938,-1.18440385848747));
#24963=CARTESIAN_POINT('Origin',(0.,-0.07938,0.));
#24964=CARTESIAN_POINT('',(-0.397005914195118,-0.07938,-1.59456899932179));
#24965=CARTESIAN_POINT('Origin',(0.,-0.07938,0.));
#24966=CARTESIAN_POINT('Origin',(1.11022302462516E-16,-0.07938,-1.675));
#24967=CARTESIAN_POINT('Origin',(1.11022302462516E-16,0.,-1.675));
#24968=CARTESIAN_POINT('',(0.397005914195118,-0.07938,-1.59456899932179));
#24969=CARTESIAN_POINT('Ctrl Pts',(0.397005914195119,-0.0793800000000001,
-1.59456899932179));
#24970=CARTESIAN_POINT('Ctrl Pts',(0.388626558458099,-0.123401821157026,
-1.59665523941937));
#24971=CARTESIAN_POINT('Ctrl Pts',(0.373030350867485,-0.166543350814306,
-1.60050712143809));
#24972=CARTESIAN_POINT('Ctrl Pts',(0.333298652394954,-0.237231147975234,
-1.60919314384089));
#24973=CARTESIAN_POINT('Ctrl Pts',(0.311480544243686,-0.266264900654909,
-1.61365775139403));
#24974=CARTESIAN_POINT('Ctrl Pts',(0.261368388670537,-0.317195968905306,
-1.62252828437015));
#24975=CARTESIAN_POINT('Ctrl Pts',(0.233069203882014,-0.33909093068465,
-1.62691869420078));
#24976=CARTESIAN_POINT('Ctrl Pts',(0.174042761838763,-0.373586846396559,
-1.63426473152765));
#24977=CARTESIAN_POINT('Ctrl Pts',(0.140365781471549,-0.388086240756494,
-1.63761964365402));
#24978=CARTESIAN_POINT('Ctrl Pts',(0.0701778381840612,-0.407068917407805,
-1.64212536811722));
#24979=CARTESIAN_POINT('Ctrl Pts',(0.0336652739555916,-0.411552957311693,
-1.643248));
#24980=CARTESIAN_POINT('Ctrl Pts',(-0.0336652739555915,-0.411552957311693,
-1.643248));
#24981=CARTESIAN_POINT('Ctrl Pts',(-0.0701778381840612,-0.407068917407805,
-1.64212536811722));
#24982=CARTESIAN_POINT('Ctrl Pts',(-0.140365781471549,-0.388086240756494,
-1.63761964365402));
#24983=CARTESIAN_POINT('Ctrl Pts',(-0.174042761838764,-0.373586846396559,
-1.63426473152765));
#24984=CARTESIAN_POINT('Ctrl Pts',(-0.233069203882014,-0.33909093068465,
-1.62691869420078));
#24985=CARTESIAN_POINT('Ctrl Pts',(-0.261368388670536,-0.317195968905306,
-1.62252828437015));
#24986=CARTESIAN_POINT('Ctrl Pts',(-0.311480544243686,-0.266264900654908,
-1.61365775139403));
#24987=CARTESIAN_POINT('Ctrl Pts',(-0.333298652394954,-0.237231147975234,
-1.60919314384089));
#24988=CARTESIAN_POINT('Ctrl Pts',(-0.373030350867485,-0.166543350814306,
-1.60050712143809));
#24989=CARTESIAN_POINT('Ctrl Pts',(-0.388626558458099,-0.123401821157026,
-1.59665523941937));
#24990=CARTESIAN_POINT('Ctrl Pts',(-0.397005914195118,-0.07938,-1.59456899932179));
#24991=CARTESIAN_POINT('Origin',(1.11022302462516E-16,-0.07938,-1.675));
#24992=CARTESIAN_POINT('Origin',(0.,-0.07938,0.));
#24993=CARTESIAN_POINT('',(0.846804978391753,-0.07938,-1.40825612658882));
#24994=CARTESIAN_POINT('Origin',(0.,-0.07938,0.));
#24995=CARTESIAN_POINT('Origin',(1.18440385848747,-0.07938,-1.18440385848747));
#24996=CARTESIAN_POINT('Origin',(1.18440385848747,0.,-1.18440385848747));
#24997=CARTESIAN_POINT('',(1.40825612658882,-0.07938,-0.846804978391753));
#24998=CARTESIAN_POINT('Ctrl Pts',(1.40825612658882,-0.0793800000000001,
-0.846804978391753));
#24999=CARTESIAN_POINT('Ctrl Pts',(1.40380622184538,-0.123401821157026,
-0.854205272175555));
#25000=CARTESIAN_POINT('Ctrl Pts',(1.39550172959303,-0.166543350814306,
-0.867957148219442));
#25001=CARTESIAN_POINT('Ctrl Pts',(1.3735491215176,-0.237231147975234,-0.902193646979983));
#25002=CARTESIAN_POINT('Ctrl Pts',(1.36127834356734,-0.266264900654908,
-0.920778333482565));
#25003=CARTESIAN_POINT('Ctrl Pts',(1.33211611256184,-0.317195968905306,
-0.962485392528369));
#25004=CARTESIAN_POINT('Ctrl Pts',(1.31521005565926,-0.33909093068465,-0.985600426557816));
#25005=CARTESIAN_POINT('Ctrl Pts',(1.27866649102984,-0.373586846396559,
-1.03253285680459));
#25006=CARTESIAN_POINT('Ctrl Pts',(1.25722555095714,-0.388086240756494,
-1.05871835910697));
#25007=CARTESIAN_POINT('Ctrl Pts',(1.2107812086231,-0.407068917407805,-1.11153475808518));
#25008=CARTESIAN_POINT('Ctrl Pts',(1.18575674747573,-0.411552957311693,
-1.13814686046673));
#25009=CARTESIAN_POINT('Ctrl Pts',(1.13814686046673,-0.411552957311693,
-1.18575674747573));
#25010=CARTESIAN_POINT('Ctrl Pts',(1.11153475808518,-0.407068917407805,
-1.2107812086231));
#25011=CARTESIAN_POINT('Ctrl Pts',(1.05871835910697,-0.388086240756494,
-1.25722555095714));
#25012=CARTESIAN_POINT('Ctrl Pts',(1.03253285680459,-0.373586846396559,
-1.27866649102984));
#25013=CARTESIAN_POINT('Ctrl Pts',(0.985600426557816,-0.33909093068465,
-1.31521005565926));
#25014=CARTESIAN_POINT('Ctrl Pts',(0.962485392528369,-0.317195968905306,
-1.33211611256184));
#25015=CARTESIAN_POINT('Ctrl Pts',(0.920778333482565,-0.266264900654909,
-1.36127834356734));
#25016=CARTESIAN_POINT('Ctrl Pts',(0.902193646979983,-0.237231147975234,
-1.3735491215176));
#25017=CARTESIAN_POINT('Ctrl Pts',(0.867957148219442,-0.166543350814306,
-1.39550172959303));
#25018=CARTESIAN_POINT('Ctrl Pts',(0.854205272175555,-0.123401821157026,
-1.40380622184538));
#25019=CARTESIAN_POINT('Ctrl Pts',(0.846804978391753,-0.0793800000000001,
-1.40825612658882));
#25020=CARTESIAN_POINT('Origin',(1.18440385848747,-0.07938,-1.18440385848747));
#25021=CARTESIAN_POINT('Origin',(0.,-0.27783,0.));
#25022=CARTESIAN_POINT('',(-1.643248,-0.47628,2.01239840340529E-16));
#25023=CARTESIAN_POINT('Origin',(0.,-0.47628,0.));
#25024=CARTESIAN_POINT('',(-1.643248,-0.27783,2.01239840340529E-16));
#25025=CARTESIAN_POINT('',(1.59456899932179,-0.07938,0.397005914195118));
#25026=CARTESIAN_POINT('Origin',(0.,-0.07938,0.));
#25027=CARTESIAN_POINT('',(1.59456899932179,-0.07938,-0.397005914195118));
#25028=CARTESIAN_POINT('Ctrl Pts',(1.59456899932179,-0.0793800000000001,
0.397005914195118));
#25029=CARTESIAN_POINT('Ctrl Pts',(1.59665523941937,-0.123401821157026,
0.388626558458099));
#25030=CARTESIAN_POINT('Ctrl Pts',(1.60050712143809,-0.166543350814306,
0.373030350867485));
#25031=CARTESIAN_POINT('Ctrl Pts',(1.60919314384089,-0.237231147975234,
0.333298652394954));
#25032=CARTESIAN_POINT('Ctrl Pts',(1.61365775139403,-0.266264900654909,
0.311480544243686));
#25033=CARTESIAN_POINT('Ctrl Pts',(1.62252828437015,-0.317195968905306,
0.261368388670537));
#25034=CARTESIAN_POINT('Ctrl Pts',(1.62691869420078,-0.33909093068465,0.233069203882014));
#25035=CARTESIAN_POINT('Ctrl Pts',(1.63426473152765,-0.373586846396559,
0.174042761838764));
#25036=CARTESIAN_POINT('Ctrl Pts',(1.63761964365402,-0.388086240756494,
0.140365781471549));
#25037=CARTESIAN_POINT('Ctrl Pts',(1.64212536811722,-0.407068917407805,
0.0701778381840612));
#25038=CARTESIAN_POINT('Ctrl Pts',(1.643248,-0.411552957311693,0.0336652739555916));
#25039=CARTESIAN_POINT('Ctrl Pts',(1.643248,-0.411552957311693,-0.0336652739555916));
#25040=CARTESIAN_POINT('Ctrl Pts',(1.64212536811722,-0.407068917407805,
-0.0701778381840612));
#25041=CARTESIAN_POINT('Ctrl Pts',(1.63761964365402,-0.388086240756494,
-0.140365781471549));
#25042=CARTESIAN_POINT('Ctrl Pts',(1.63426473152765,-0.373586846396559,
-0.174042761838764));
#25043=CARTESIAN_POINT('Ctrl Pts',(1.62691869420078,-0.33909093068465,-0.233069203882014));
#25044=CARTESIAN_POINT('Ctrl Pts',(1.62252828437015,-0.317195968905306,
-0.261368388670537));
#25045=CARTESIAN_POINT('Ctrl Pts',(1.61365775139403,-0.266264900654909,
-0.311480544243686));
#25046=CARTESIAN_POINT('Ctrl Pts',(1.60919314384089,-0.237231147975234,
-0.333298652394954));
#25047=CARTESIAN_POINT('Ctrl Pts',(1.60050712143809,-0.166543350814306,
-0.373030350867485));
#25048=CARTESIAN_POINT('Ctrl Pts',(1.59665523941937,-0.123401821157026,
-0.388626558458099));
#25049=CARTESIAN_POINT('Ctrl Pts',(1.59456899932179,-0.07938,-0.397005914195118));
#25050=CARTESIAN_POINT('Origin',(0.,-0.07938,0.));
#25051=CARTESIAN_POINT('Origin',(0.,-0.07938,0.));
#25052=CARTESIAN_POINT('Origin',(1.675,-0.07938,0.));
#25053=CARTESIAN_POINT('Origin',(1.675,0.,0.));
#25054=CARTESIAN_POINT('Origin',(1.675,-0.07938,0.));
#25055=CARTESIAN_POINT('Origin',(0.,-0.47628,0.));
#25056=CARTESIAN_POINT('Origin',(0.,-0.07938,0.));
#25057=CARTESIAN_POINT('',(0.,0.,0.));
#25058=CARTESIAN_POINT('Origin',(1.70469,0.695,0.));
#25059=CARTESIAN_POINT('',(-1.70469,0.695,-2.0876431520385E-16));
#25060=CARTESIAN_POINT('Origin',(0.,0.695,0.));
#25061=CARTESIAN_POINT('',(-1.65031,0.695,-2.02104685910087E-16));
#25062=CARTESIAN_POINT('Origin',(0.,0.695,0.));
#25063=CARTESIAN_POINT('Origin',(0.,0.6575,0.));
#25064=CARTESIAN_POINT('',(-1.70469,0.62,-2.0876431520385E-16));
#25065=CARTESIAN_POINT('Origin',(0.,0.62,0.));
#25066=CARTESIAN_POINT('',(-1.70469,0.6575,-2.0876431520385E-16));
#25067=CARTESIAN_POINT('Origin',(1.65031,0.62,0.));
#25068=CARTESIAN_POINT('',(-1.65031,0.62,-2.02104685910087E-16));
#25069=CARTESIAN_POINT('Origin',(0.,0.62,0.));
#25070=CARTESIAN_POINT('Origin',(0.,0.6575,0.));
#25071=CARTESIAN_POINT('',(-1.65031,0.6575,-2.02104685910087E-16));
#25072=CARTESIAN_POINT('Origin',(1.70469,-0.62,0.));
#25073=CARTESIAN_POINT('',(-1.70469,-0.62,-2.0876431520385E-16));
#25074=CARTESIAN_POINT('Origin',(0.,-0.62,0.));
#25075=CARTESIAN_POINT('',(-1.65031,-0.62,-2.02104685910087E-16));
#25076=CARTESIAN_POINT('Origin',(0.,-0.62,0.));
#25077=CARTESIAN_POINT('Origin',(0.,-0.6575,0.));
#25078=CARTESIAN_POINT('',(-1.70469,-0.695,-2.0876431520385E-16));
#25079=CARTESIAN_POINT('Origin',(0.,-0.695,0.));
#25080=CARTESIAN_POINT('',(-1.70469,-0.6575,-2.0876431520385E-16));
#25081=CARTESIAN_POINT('Origin',(1.65031,-0.695,0.));
#25082=CARTESIAN_POINT('',(-1.65031,-0.695,-2.02104685910087E-16));
#25083=CARTESIAN_POINT('Origin',(0.,-0.695,0.));
#25084=CARTESIAN_POINT('Origin',(0.,-0.6575,0.));
#25085=CARTESIAN_POINT('',(-1.65031,-0.6575,-2.02104685910087E-16));
#25086=CARTESIAN_POINT('',(0.,0.,0.));
#25087=CARTESIAN_POINT('',(0.,0.,0.));
#25088=CARTESIAN_POINT('',(0.,0.,0.));
#25089=CARTESIAN_POINT('',(0.,0.,0.));
#25090=CARTESIAN_POINT('',(0.,0.,0.));
#25091=CARTESIAN_POINT('',(0.,0.,0.));
#25092=CARTESIAN_POINT('Origin',(0.0866025403784439,-0.4,-0.15));
#25093=CARTESIAN_POINT('',(0.173205080756888,-0.4,0.));
#25094=CARTESIAN_POINT('',(0.0866025403784439,-0.4,-0.15));
#25095=CARTESIAN_POINT('',(0.173205080756888,-0.4,0.));
#25096=CARTESIAN_POINT('',(0.0866025403784439,-0.64,-0.15));
#25097=CARTESIAN_POINT('',(0.0866025403784439,-0.4,-0.15));
#25098=CARTESIAN_POINT('',(0.173205080756888,-0.64,0.));
#25099=CARTESIAN_POINT('',(0.173205080756888,-0.64,0.));
#25100=CARTESIAN_POINT('',(0.173205080756888,-0.4,0.));
#25101=CARTESIAN_POINT('Origin',(-0.0866025403784438,-0.4,-0.15));
#25102=CARTESIAN_POINT('',(-0.0866025403784438,-0.4,-0.15));
#25103=CARTESIAN_POINT('',(0.0866025403784439,-0.4,-0.15));
#25104=CARTESIAN_POINT('',(-0.0866025403784438,-0.64,-0.15));
#25105=CARTESIAN_POINT('',(-0.0866025403784438,-0.4,-0.15));
#25106=CARTESIAN_POINT('',(0.0866025403784439,-0.64,-0.15));
#25107=CARTESIAN_POINT('Origin',(-0.173205080756888,-0.4,-2.77555756156289E-17));
#25108=CARTESIAN_POINT('',(-0.173205080756888,-0.4,-2.12115047744981E-17));
#25109=CARTESIAN_POINT('',(-0.0866025403784438,-0.4,-0.15));
#25110=CARTESIAN_POINT('',(-0.173205080756888,-0.64,-2.77555756156289E-17));
#25111=CARTESIAN_POINT('',(-0.173205080756888,-0.4,-2.12115047744981E-17));
#25112=CARTESIAN_POINT('',(-0.0866025403784438,-0.64,-0.15));
#25113=CARTESIAN_POINT('Origin',(-0.0866025403784439,-0.4,0.15));
#25114=CARTESIAN_POINT('',(-0.0866025403784439,-0.4,0.15));
#25115=CARTESIAN_POINT('',(-0.173205080756888,-0.4,-2.12115047744981E-17));
#25116=CARTESIAN_POINT('',(-0.0866025403784439,-0.64,0.15));
#25117=CARTESIAN_POINT('',(-0.0866025403784439,-0.4,0.15));
#25118=CARTESIAN_POINT('',(-0.173205080756888,-0.64,-2.12115047744981E-17));
#25119=CARTESIAN_POINT('Origin',(0.0866025403784439,-0.4,0.15));
#25120=CARTESIAN_POINT('',(0.0866025403784439,-0.4,0.15));
#25121=CARTESIAN_POINT('',(-0.0866025403784439,-0.4,0.15));
#25122=CARTESIAN_POINT('',(0.0866025403784439,-0.64,0.15));
#25123=CARTESIAN_POINT('',(0.0866025403784439,-0.4,0.15));
#25124=CARTESIAN_POINT('',(-0.0866025403784439,-0.64,0.15));
#25125=CARTESIAN_POINT('Origin',(0.173205080756888,-0.4,0.));
#25126=CARTESIAN_POINT('',(0.0866025403784439,-0.4,0.15));
#25127=CARTESIAN_POINT('',(0.0866025403784439,-0.64,0.15));
#25128=CARTESIAN_POINT('Origin',(0.,-0.4,-2.77555756156289E-17));
#25129=CARTESIAN_POINT('Origin',(0.,-0.64,-2.77555756156289E-17));
#25130=CARTESIAN_POINT('Origin',(0.,-1.,0.));
#25131=CARTESIAN_POINT('',(-0.1954,-1.,2.39295984553393E-17));
#25132=CARTESIAN_POINT('Origin',(0.,-1.,0.));
#25133=CARTESIAN_POINT('Origin',(0.3,0.4,0.));
#25134=CARTESIAN_POINT('',(-0.3,0.4,-3.67394039744206E-17));
#25135=CARTESIAN_POINT('Origin',(0.,0.4,0.));
#25136=CARTESIAN_POINT('Origin',(0.,0.375,0.));
#25137=CARTESIAN_POINT('',(-0.35,0.35,-4.28626379701573E-17));
#25138=CARTESIAN_POINT('Origin',(0.,0.35,0.));
#25139=CARTESIAN_POINT('',(-0.325,0.375,-3.9801020972289E-17));
#25140=CARTESIAN_POINT('Origin',(0.,0.19,0.));
#25141=CARTESIAN_POINT('',(-0.35,0.03,-4.28626379701574E-17));
#25142=CARTESIAN_POINT('Origin',(0.,0.03,0.));
#25143=CARTESIAN_POINT('',(-0.35,0.19,-4.28626379701574E-17));
#25144=CARTESIAN_POINT('Origin',(0.,0.0149999999999999,0.));
#25145=CARTESIAN_POINT('',(-0.32,-3.29597460435593E-17,-3.91886975727153E-17));
#25146=CARTESIAN_POINT('Origin',(0.,0.,0.));
#25147=CARTESIAN_POINT('',(-0.335,0.0149999999999999,-4.10256677714363E-17));
#25148=CARTESIAN_POINT('Origin',(0.22,0.,0.));
#25149=CARTESIAN_POINT('',(-0.22,-6.93889390390723E-18,-2.69422295812418E-17));
#25150=CARTESIAN_POINT('Origin',(0.,0.,0.));
#25151=CARTESIAN_POINT('Origin',(0.,-0.02,0.));
#25152=CARTESIAN_POINT('',(-0.1954,-0.0492,2.39295984553393E-17));
#25153=CARTESIAN_POINT('Origin',(0.,-0.0492,0.));
#25154=CARTESIAN_POINT('',(-0.21,-0.02,-2.57175827820944E-17));
#25155=CARTESIAN_POINT('Origin',(0.,-0.8,0.));
#25156=CARTESIAN_POINT('',(-0.1954,-0.8,-2.39295984553393E-17));
#25157=CARTESIAN_POINT('',(0.,0.,0.));
#25158=CARTESIAN_POINT('Origin',(21.6782686989894,4.15,8.0458829327411));
#25159=CARTESIAN_POINT('',(21.6625326688994,4.2,7.98715526893581));
#25160=CARTESIAN_POINT('',(21.6782686989894,4.2,8.0458829327411));
#25161=CARTESIAN_POINT('',(21.6743346914669,4.2,8.03120101678986));
#25162=CARTESIAN_POINT('',(21.6625326688994,4.15,7.98715526893581));
#25163=CARTESIAN_POINT('',(21.6625326688994,4.15,7.98715526893581));
#25164=CARTESIAN_POINT('',(21.6782686989894,4.15,8.0458829327411));
#25165=CARTESIAN_POINT('',(21.6625326688994,4.15,7.98715526893581));
#25166=CARTESIAN_POINT('',(21.6782686989894,4.15,8.0458829327411));
#25167=CARTESIAN_POINT('Origin',(21.2910825201484,4.15,8.14631630824203));
#25168=CARTESIAN_POINT('',(21.2910825201484,4.2,8.14631630824203));
#25169=CARTESIAN_POINT('',(19.6455412600742,4.2,8.57315815412101));
#25170=CARTESIAN_POINT('',(21.2910825201484,4.15,8.14631630824203));
#25171=CARTESIAN_POINT('',(21.6782686989894,4.15,8.0458829327411));
#25172=CARTESIAN_POINT('',(21.2910825201484,4.15,8.14631630824203));
#25173=CARTESIAN_POINT('Origin',(21.2770029142784,4.15,8.09377050378467));
#25174=CARTESIAN_POINT('',(21.2770029142784,4.2,8.09377050378467));
#25175=CARTESIAN_POINT('',(21.2805228157459,4.2,8.10690695489906));
#25176=CARTESIAN_POINT('',(21.2770029142784,4.15,8.09377050378467));
#25177=CARTESIAN_POINT('',(21.2910825201484,4.15,8.14631630824203));
#25178=CARTESIAN_POINT('',(21.2770029142784,4.15,8.09377050378467));
#25179=CARTESIAN_POINT('Origin',(21.6625326688994,4.15,7.98715526893581));
#25180=CARTESIAN_POINT('',(19.8312663344497,4.2,8.49357763446791));
#25181=CARTESIAN_POINT('',(21.2770029142784,4.15,8.09377050378467));
#25182=CARTESIAN_POINT('Origin',(21.4776358066339,4.15,8.06673578858892));
#25183=CARTESIAN_POINT('Origin',(21.3059910641206,4.15,7.12638769112851));
#25184=CARTESIAN_POINT('',(21.2755913883862,4.2,7.07373390822296));
#25185=CARTESIAN_POINT('',(21.3059910641206,4.2,7.12638769112851));
#25186=CARTESIAN_POINT('',(21.298391145187,4.2,7.11322424540209));
#25187=CARTESIAN_POINT('',(21.2755913883862,4.15,7.07373390822296));
#25188=CARTESIAN_POINT('',(21.2755913883862,4.15,7.07373390822296));
#25189=CARTESIAN_POINT('',(21.3059910641206,4.15,7.12638769112851));
#25190=CARTESIAN_POINT('',(21.2755913883862,4.15,7.07373390822296));
#25191=CARTESIAN_POINT('',(21.3059910641206,4.15,7.12638769112851));
#25192=CARTESIAN_POINT('Origin',(20.9579920047395,4.15,7.32361003943077));
#25193=CARTESIAN_POINT('',(20.9579920047395,4.2,7.32361003943077));
#25194=CARTESIAN_POINT('',(19.4789960023697,4.2,8.16180501971539));
#25195=CARTESIAN_POINT('',(20.9579920047395,4.15,7.32361003943077));
#25196=CARTESIAN_POINT('',(21.3059910641206,4.15,7.12638769112851));
#25197=CARTESIAN_POINT('',(20.9579920047395,4.15,7.32361003943077));
#25198=CARTESIAN_POINT('Origin',(20.9307922948719,4.15,7.27649875998896));
#25199=CARTESIAN_POINT('',(20.9307922948719,4.2,7.27649875998896));
#25200=CARTESIAN_POINT('',(20.9375922223388,4.2,7.28827657984941));
#25201=CARTESIAN_POINT('',(20.9307922948719,4.15,7.27649875998896));
#25202=CARTESIAN_POINT('',(20.9579920047395,4.15,7.32361003943077));
#25203=CARTESIAN_POINT('',(20.9307922948719,4.15,7.27649875998896));
#25204=CARTESIAN_POINT('Origin',(21.2755913883862,4.15,7.07373390822296));
#25205=CARTESIAN_POINT('',(19.6377956941931,4.2,8.03686695411148));
#25206=CARTESIAN_POINT('',(20.9307922948719,4.15,7.27649875998896));
#25207=CARTESIAN_POINT('Origin',(21.1183916794962,4.15,7.19867197382686));
#25208=CARTESIAN_POINT('Origin',(20.7084156016405,4.15,6.33457603207478));
#25209=CARTESIAN_POINT('',(20.6654239679252,4.2,6.29158439835948));
#25210=CARTESIAN_POINT('',(20.7084156016405,4.2,6.33457603207478));
#25211=CARTESIAN_POINT('',(20.6976676932117,4.2,6.32382812364594));
#25212=CARTESIAN_POINT('',(20.6654239679252,4.15,6.29158439835948));
#25213=CARTESIAN_POINT('',(20.6654239679252,4.15,6.29158439835948));
#25214=CARTESIAN_POINT('',(20.7084156016405,4.15,6.33457603207478));
#25215=CARTESIAN_POINT('',(20.6654239679252,4.15,6.29158439835948));
#25216=CARTESIAN_POINT('',(20.7084156016405,4.15,6.33457603207478));
#25217=CARTESIAN_POINT('Origin',(20.4233192225205,4.15,6.6151469760669));
#25218=CARTESIAN_POINT('',(20.4233192225205,4.2,6.6151469760669));
#25219=CARTESIAN_POINT('',(19.2116596112602,4.2,7.80757348803345));
#25220=CARTESIAN_POINT('',(20.4233192225205,4.15,6.6151469760669));
#25221=CARTESIAN_POINT('',(20.7084156016405,4.15,6.33457603207478));
#25222=CARTESIAN_POINT('',(20.4233192225205,4.15,6.6151469760669));
#25223=CARTESIAN_POINT('Origin',(20.3848530239331,4.15,6.57668077747954));
#25224=CARTESIAN_POINT('',(20.3848530239331,4.2,6.57668077747954));
#25225=CARTESIAN_POINT('',(20.39446957358,4.2,6.58629732712641));
#25226=CARTESIAN_POINT('',(20.3848530239331,4.15,6.57668077747954));
#25227=CARTESIAN_POINT('',(20.4233192225205,4.15,6.6151469760669));
#25228=CARTESIAN_POINT('',(20.3848530239331,4.15,6.57668077747954));
#25229=CARTESIAN_POINT('Origin',(20.6654239679252,4.15,6.29158439835948));
#25230=CARTESIAN_POINT('',(19.3327119839626,4.2,7.64579219917974));
#25231=CARTESIAN_POINT('',(20.3848530239331,4.15,6.57668077747954));
#25232=CARTESIAN_POINT('Origin',(20.5466343127868,4.15,6.45336568721319));
#25233=CARTESIAN_POINT('Origin',(19.926266091777,4.15,5.72440861161377));
#25234=CARTESIAN_POINT('',(19.8736123088715,4.2,5.6940089358794));
#25235=CARTESIAN_POINT('',(19.926266091777,4.2,5.72440861161377));
#25236=CARTESIAN_POINT('',(19.9131026460507,4.2,5.71680869268019));
#25237=CARTESIAN_POINT('',(19.8736123088715,4.15,5.6940089358794));
#25238=CARTESIAN_POINT('',(19.8736123088715,4.15,5.6940089358794));
#25239=CARTESIAN_POINT('',(19.926266091777,4.15,5.72440861161377));
#25240=CARTESIAN_POINT('',(19.8736123088715,4.15,5.6940089358794));
#25241=CARTESIAN_POINT('',(19.926266091777,4.15,5.72440861161377));
#25242=CARTESIAN_POINT('Origin',(19.723501240011,4.15,6.06920770512811));
#25243=CARTESIAN_POINT('',(19.723501240011,4.2,6.06920770512811));
#25244=CARTESIAN_POINT('',(18.8617506200055,4.2,7.53460385256405));
#25245=CARTESIAN_POINT('',(19.723501240011,4.15,6.06920770512811));
#25246=CARTESIAN_POINT('',(19.926266091777,4.15,5.72440861161377));
#25247=CARTESIAN_POINT('',(19.723501240011,4.15,6.06920770512811));
#25248=CARTESIAN_POINT('Origin',(19.6763899605692,4.15,6.04200799526052));
#25249=CARTESIAN_POINT('',(19.6763899605692,4.2,6.04200799526052));
#25250=CARTESIAN_POINT('',(19.6881677804297,4.2,6.04880792272743));
#25251=CARTESIAN_POINT('',(19.6763899605692,4.15,6.04200799526052));
#25252=CARTESIAN_POINT('',(19.723501240011,4.15,6.06920770512811));
#25253=CARTESIAN_POINT('',(19.6763899605692,4.15,6.04200799526052));
#25254=CARTESIAN_POINT('Origin',(19.8736123088715,4.15,5.6940089358794));
#25255=CARTESIAN_POINT('',(18.9368061544358,4.2,7.3470044679397));
#25256=CARTESIAN_POINT('',(19.6763899605692,4.15,6.04200799526052));
#25257=CARTESIAN_POINT('Origin',(19.8013280261731,4.15,5.88160832050376));
#25258=CARTESIAN_POINT('Origin',(19.0128447310642,4.15,5.33746733110058));
#25259=CARTESIAN_POINT('',(18.9541170672589,4.2,5.32173130101059));
#25260=CARTESIAN_POINT('',(19.0128447310642,4.2,5.33746733110058));
#25261=CARTESIAN_POINT('',(18.9981628151129,4.2,5.33353332357809));
#25262=CARTESIAN_POINT('',(18.9541170672589,4.15,5.32173130101059));
#25263=CARTESIAN_POINT('',(18.9541170672589,4.15,5.32173130101059));
#25264=CARTESIAN_POINT('',(19.0128447310642,4.15,5.33746733110058));
#25265=CARTESIAN_POINT('',(18.9541170672589,4.15,5.32173130101059));
#25266=CARTESIAN_POINT('',(19.0128447310642,4.15,5.33746733110058));
#25267=CARTESIAN_POINT('Origin',(18.9062294962153,4.15,5.72299708572157));
#25268=CARTESIAN_POINT('',(18.9062294962153,4.2,5.72299708572157));
#25269=CARTESIAN_POINT('',(18.4531147481077,4.2,7.36149854286079));
#25270=CARTESIAN_POINT('',(18.9062294962153,4.15,5.72299708572157));
#25271=CARTESIAN_POINT('',(19.0128447310642,4.15,5.33746733110058));
#25272=CARTESIAN_POINT('',(18.9062294962153,4.15,5.72299708572157));
#25273=CARTESIAN_POINT('Origin',(18.853683691758,4.15,5.70891747985158));
#25274=CARTESIAN_POINT('',(18.853683691758,4.2,5.70891747985158));
#25275=CARTESIAN_POINT('',(18.8668201428723,4.2,5.71243738131908));
#25276=CARTESIAN_POINT('',(18.853683691758,4.15,5.70891747985158));
#25277=CARTESIAN_POINT('',(18.9062294962153,4.15,5.72299708572157));
#25278=CARTESIAN_POINT('',(18.853683691758,4.15,5.70891747985158));
#25279=CARTESIAN_POINT('Origin',(18.9541170672589,4.15,5.32173130101059));
#25280=CARTESIAN_POINT('',(18.4770585336294,4.2,7.16086565050529));
#25281=CARTESIAN_POINT('',(18.853683691758,4.15,5.70891747985158));
#25282=CARTESIAN_POINT('Origin',(18.9332642114111,4.15,5.52236419336608));
#25283=CARTESIAN_POINT('Origin',(18.0303996757344,4.15,5.20012159935147));
#25284=CARTESIAN_POINT('',(17.9696003242656,4.2,5.20012159935147));
#25285=CARTESIAN_POINT('',(18.0303996757344,4.2,5.20012159935147));
#25286=CARTESIAN_POINT('',(18.0151998378672,4.2,5.20012159935147));
#25287=CARTESIAN_POINT('',(17.9696003242656,4.15,5.20012159935147));
#25288=CARTESIAN_POINT('',(17.9696003242656,4.15,5.20012159935147));
#25289=CARTESIAN_POINT('',(18.0303996757344,4.15,5.20012159935147));
#25290=CARTESIAN_POINT('',(17.9696003242656,4.15,5.20012159935147));
#25291=CARTESIAN_POINT('',(18.0303996757344,4.15,5.20012159935147));
#25292=CARTESIAN_POINT('Origin',(18.0271997098676,4.15,5.60010879941973));
#25293=CARTESIAN_POINT('',(18.0271997098676,4.2,5.60010879941973));
#25294=CARTESIAN_POINT('',(18.0135998549338,4.2,7.30005439970987));
#25295=CARTESIAN_POINT('',(18.0271997098676,4.15,5.60010879941973));
#25296=CARTESIAN_POINT('',(18.0303996757344,4.15,5.20012159935147));
#25297=CARTESIAN_POINT('',(18.0271997098676,4.15,5.60010879941973));
#25298=CARTESIAN_POINT('Origin',(17.9728002901324,4.15,5.60010879941973));
#25299=CARTESIAN_POINT('',(17.9728002901324,4.2,5.60010879941973));
#25300=CARTESIAN_POINT('',(17.9864001450662,4.2,5.60010879941973));
#25301=CARTESIAN_POINT('',(17.9728002901324,4.15,5.60010879941973));
#25302=CARTESIAN_POINT('',(18.0271997098676,4.15,5.60010879941973));
#25303=CARTESIAN_POINT('',(17.9728002901324,4.15,5.60010879941973));
#25304=CARTESIAN_POINT('Origin',(17.9696003242656,4.15,5.20012159935147));
#25305=CARTESIAN_POINT('',(17.9848001621328,4.2,7.10006079967573));
#25306=CARTESIAN_POINT('',(17.9728002901324,4.15,5.60010879941973));
#25307=CARTESIAN_POINT('Origin',(18.,4.15,5.4001151993856));
#25308=CARTESIAN_POINT('Origin',(17.0458829327411,4.15,5.32173130101059));
#25309=CARTESIAN_POINT('',(16.9871552689358,4.2,5.33746733110058));
#25310=CARTESIAN_POINT('',(17.0458829327411,4.2,5.32173130101059));
#25311=CARTESIAN_POINT('',(17.0312010167898,4.2,5.32566530853307));
#25312=CARTESIAN_POINT('',(16.9871552689358,4.15,5.33746733110058));
#25313=CARTESIAN_POINT('',(16.9871552689358,4.15,5.33746733110058));
#25314=CARTESIAN_POINT('',(17.0458829327411,4.15,5.32173130101059));
#25315=CARTESIAN_POINT('',(16.9871552689358,4.15,5.33746733110058));
#25316=CARTESIAN_POINT('',(17.0458829327411,4.15,5.32173130101059));
#25317=CARTESIAN_POINT('Origin',(17.146316308242,4.15,5.70891747985158));
#25318=CARTESIAN_POINT('',(17.146316308242,4.2,5.70891747985158));
#25319=CARTESIAN_POINT('',(17.573158154121,4.2,7.35445873992579));
#25320=CARTESIAN_POINT('',(17.146316308242,4.15,5.70891747985158));
#25321=CARTESIAN_POINT('',(17.0458829327411,4.15,5.32173130101059));
#25322=CARTESIAN_POINT('',(17.146316308242,4.15,5.70891747985158));
#25323=CARTESIAN_POINT('Origin',(17.0937705037847,4.15,5.72299708572157));
#25324=CARTESIAN_POINT('',(17.0937705037847,4.2,5.72299708572157));
#25325=CARTESIAN_POINT('',(17.106906954899,4.2,5.71947718425408));
#25326=CARTESIAN_POINT('',(17.0937705037847,4.15,5.72299708572157));
#25327=CARTESIAN_POINT('',(17.146316308242,4.15,5.70891747985158));
#25328=CARTESIAN_POINT('',(17.0937705037847,4.15,5.72299708572157));
#25329=CARTESIAN_POINT('Origin',(16.9871552689358,4.15,5.33746733110058));
#25330=CARTESIAN_POINT('',(17.4935776344679,4.2,7.16873366555029));
#25331=CARTESIAN_POINT('',(17.0937705037847,4.15,5.72299708572157));
#25332=CARTESIAN_POINT('Origin',(17.0667357885889,4.15,5.52236419336608));
#25333=CARTESIAN_POINT('Origin',(16.1263876911285,4.15,5.6940089358794));
#25334=CARTESIAN_POINT('',(16.073733908223,4.2,5.72440861161377));
#25335=CARTESIAN_POINT('',(16.1263876911285,4.2,5.6940089358794));
#25336=CARTESIAN_POINT('',(16.1132242454022,4.2,5.70160885481298));
#25337=CARTESIAN_POINT('',(16.073733908223,4.15,5.72440861161377));
#25338=CARTESIAN_POINT('',(16.073733908223,4.15,5.72440861161377));
#25339=CARTESIAN_POINT('',(16.1263876911285,4.15,5.6940089358794));
#25340=CARTESIAN_POINT('',(16.073733908223,4.15,5.72440861161377));
#25341=CARTESIAN_POINT('',(16.1263876911285,4.15,5.6940089358794));
#25342=CARTESIAN_POINT('Origin',(16.3236100394308,4.15,6.04200799526052));
#25343=CARTESIAN_POINT('',(16.3236100394308,4.2,6.04200799526052));
#25344=CARTESIAN_POINT('',(17.1618050197154,4.2,7.52100399763026));
#25345=CARTESIAN_POINT('',(16.3236100394308,4.15,6.04200799526052));
#25346=CARTESIAN_POINT('',(16.1263876911285,4.15,5.6940089358794));
#25347=CARTESIAN_POINT('',(16.3236100394308,4.15,6.04200799526052));
#25348=CARTESIAN_POINT('Origin',(16.276498759989,4.15,6.06920770512811));
#25349=CARTESIAN_POINT('',(16.276498759989,4.2,6.06920770512811));
#25350=CARTESIAN_POINT('',(16.2882765798494,4.2,6.06240777766122));
#25351=CARTESIAN_POINT('',(16.276498759989,4.15,6.06920770512811));
#25352=CARTESIAN_POINT('',(16.3236100394308,4.15,6.04200799526052));
#25353=CARTESIAN_POINT('',(16.276498759989,4.15,6.06920770512811));
#25354=CARTESIAN_POINT('Origin',(16.073733908223,4.15,5.72440861161377));
#25355=CARTESIAN_POINT('',(17.0368669541115,4.2,7.36220430580689));
#25356=CARTESIAN_POINT('',(16.276498759989,4.15,6.06920770512811));
#25357=CARTESIAN_POINT('Origin',(16.1986719738269,4.15,5.88160832050376));
#25358=CARTESIAN_POINT('Origin',(15.3345760320748,4.15,6.29158439835949));
#25359=CARTESIAN_POINT('',(15.2915843983595,4.2,6.33457603207478));
#25360=CARTESIAN_POINT('',(15.3345760320748,4.2,6.29158439835949));
#25361=CARTESIAN_POINT('',(15.3238281236459,4.2,6.30233230678832));
#25362=CARTESIAN_POINT('',(15.2915843983595,4.15,6.33457603207478));
#25363=CARTESIAN_POINT('',(15.2915843983595,4.15,6.33457603207478));
#25364=CARTESIAN_POINT('',(15.3345760320748,4.15,6.29158439835949));
#25365=CARTESIAN_POINT('',(15.2915843983595,4.15,6.33457603207478));
#25366=CARTESIAN_POINT('',(15.3345760320748,4.15,6.29158439835949));
#25367=CARTESIAN_POINT('Origin',(15.6151469760669,4.15,6.57668077747954));
#25368=CARTESIAN_POINT('',(15.6151469760669,4.2,6.57668077747954));
#25369=CARTESIAN_POINT('',(16.8075734880335,4.2,7.78834038873977));
#25370=CARTESIAN_POINT('',(15.6151469760669,4.15,6.57668077747954));
#25371=CARTESIAN_POINT('',(15.3345760320748,4.15,6.29158439835949));
#25372=CARTESIAN_POINT('',(15.6151469760669,4.15,6.57668077747954));
#25373=CARTESIAN_POINT('Origin',(15.5766807774795,4.15,6.61514697606691));
#25374=CARTESIAN_POINT('',(15.5766807774795,4.2,6.61514697606691));
#25375=CARTESIAN_POINT('',(15.5862973271264,4.2,6.60553042642005));
#25376=CARTESIAN_POINT('',(15.5766807774795,4.15,6.61514697606691));
#25377=CARTESIAN_POINT('',(15.6151469760669,4.15,6.57668077747954));
#25378=CARTESIAN_POINT('',(15.5766807774795,4.15,6.61514697606691));
#25379=CARTESIAN_POINT('Origin',(15.2915843983595,4.15,6.33457603207478));
#25380=CARTESIAN_POINT('',(16.6457921991797,4.2,7.66728801603739));
#25381=CARTESIAN_POINT('',(15.5766807774795,4.15,6.61514697606691));
#25382=CARTESIAN_POINT('Origin',(15.4533656872132,4.15,6.4533656872132));
#25383=CARTESIAN_POINT('Origin',(14.7244086116138,4.15,7.07373390822296));
#25384=CARTESIAN_POINT('',(14.6940089358794,4.2,7.12638769112851));
#25385=CARTESIAN_POINT('',(14.7244086116138,4.2,7.07373390822296));
#25386=CARTESIAN_POINT('',(14.7168086926802,4.2,7.0868973539493));
#25387=CARTESIAN_POINT('',(14.6940089358794,4.15,7.12638769112851));
#25388=CARTESIAN_POINT('',(14.6940089358794,4.15,7.12638769112851));
#25389=CARTESIAN_POINT('',(14.7244086116138,4.15,7.07373390822296));
#25390=CARTESIAN_POINT('',(14.6940089358794,4.15,7.12638769112851));
#25391=CARTESIAN_POINT('',(14.7244086116138,4.15,7.07373390822296));
#25392=CARTESIAN_POINT('Origin',(15.0692077051281,4.15,7.27649875998896));
#25393=CARTESIAN_POINT('',(15.0692077051281,4.2,7.27649875998896));
#25394=CARTESIAN_POINT('',(16.5346038525641,4.2,8.13824937999448));
#25395=CARTESIAN_POINT('',(15.0692077051281,4.15,7.27649875998896));
#25396=CARTESIAN_POINT('',(14.7244086116138,4.15,7.07373390822296));
#25397=CARTESIAN_POINT('',(15.0692077051281,4.15,7.27649875998896));
#25398=CARTESIAN_POINT('Origin',(15.0420079952605,4.15,7.32361003943077));
#25399=CARTESIAN_POINT('',(15.0420079952605,4.2,7.32361003943077));
#25400=CARTESIAN_POINT('',(15.0488079227274,4.2,7.31183221957035));
#25401=CARTESIAN_POINT('',(15.0420079952605,4.15,7.32361003943077));
#25402=CARTESIAN_POINT('',(15.0692077051281,4.15,7.27649875998896));
#25403=CARTESIAN_POINT('',(15.0420079952605,4.15,7.32361003943077));
#25404=CARTESIAN_POINT('Origin',(14.6940089358794,4.15,7.12638769112851));
#25405=CARTESIAN_POINT('',(16.3470044679397,4.2,8.06319384556425));
#25406=CARTESIAN_POINT('',(15.0420079952605,4.15,7.32361003943077));
#25407=CARTESIAN_POINT('Origin',(14.8816083205038,4.15,7.19867197382687));
#25408=CARTESIAN_POINT('Origin',(14.3374673311006,4.15,7.98715526893581));
#25409=CARTESIAN_POINT('',(14.3217313010106,4.2,8.0458829327411));
#25410=CARTESIAN_POINT('',(14.3374673311006,4.2,7.98715526893581));
#25411=CARTESIAN_POINT('',(14.3335333235781,4.2,8.00183718488717));
#25412=CARTESIAN_POINT('',(14.3217313010106,4.15,8.0458829327411));
#25413=CARTESIAN_POINT('',(14.3217313010106,4.15,8.0458829327411));
#25414=CARTESIAN_POINT('',(14.3374673311006,4.15,7.98715526893581));
#25415=CARTESIAN_POINT('',(14.3217313010106,4.15,8.0458829327411));
#25416=CARTESIAN_POINT('',(14.3374673311006,4.15,7.98715526893581));
#25417=CARTESIAN_POINT('Origin',(14.7229970857216,4.15,8.09377050378467));
#25418=CARTESIAN_POINT('',(14.7229970857216,4.2,8.09377050378467));
#25419=CARTESIAN_POINT('',(16.3614985428608,4.2,8.54688525189233));
#25420=CARTESIAN_POINT('',(14.7229970857216,4.15,8.09377050378467));
#25421=CARTESIAN_POINT('',(14.3374673311006,4.15,7.98715526893581));
#25422=CARTESIAN_POINT('',(14.7229970857216,4.15,8.09377050378467));
#25423=CARTESIAN_POINT('Origin',(14.7089174798516,4.15,8.14631630824203));
#25424=CARTESIAN_POINT('',(14.7089174798516,4.2,8.14631630824203));
#25425=CARTESIAN_POINT('',(14.7124373813191,4.2,8.13317985712775));
#25426=CARTESIAN_POINT('',(14.7089174798516,4.15,8.14631630824203));
#25427=CARTESIAN_POINT('',(14.7229970857216,4.15,8.09377050378467));
#25428=CARTESIAN_POINT('',(14.7089174798516,4.15,8.14631630824203));
#25429=CARTESIAN_POINT('Origin',(14.3217313010106,4.15,8.0458829327411));
#25430=CARTESIAN_POINT('',(16.1608656505053,4.2,8.52294146637054));
#25431=CARTESIAN_POINT('',(14.7089174798516,4.15,8.14631630824203));
#25432=CARTESIAN_POINT('Origin',(14.5223641933661,4.15,8.06673578858892));
#25433=CARTESIAN_POINT('Origin',(14.2001215993515,4.15,8.96960032426563));
#25434=CARTESIAN_POINT('',(14.2001215993515,4.2,9.03039967573437));
#25435=CARTESIAN_POINT('',(14.2001215993515,4.2,8.96960032426563));
#25436=CARTESIAN_POINT('',(14.2001215993515,4.2,8.98480016213281));
#25437=CARTESIAN_POINT('',(14.2001215993515,4.15,9.03039967573437));
#25438=CARTESIAN_POINT('',(14.2001215993515,4.15,9.03039967573437));
#25439=CARTESIAN_POINT('',(14.2001215993515,4.15,8.96960032426563));
#25440=CARTESIAN_POINT('',(14.2001215993515,4.15,9.03039967573437));
#25441=CARTESIAN_POINT('',(14.2001215993515,4.15,8.96960032426563));
#25442=CARTESIAN_POINT('Origin',(14.6001087994197,4.15,8.9728002901324));
#25443=CARTESIAN_POINT('',(14.6001087994197,4.2,8.9728002901324));
#25444=CARTESIAN_POINT('',(16.3000543997099,4.2,8.9864001450662));
#25445=CARTESIAN_POINT('',(14.6001087994197,4.15,8.9728002901324));
#25446=CARTESIAN_POINT('',(14.2001215993515,4.15,8.96960032426563));
#25447=CARTESIAN_POINT('',(14.6001087994197,4.15,8.9728002901324));
#25448=CARTESIAN_POINT('Origin',(14.6001087994197,4.15,9.0271997098676));
#25449=CARTESIAN_POINT('',(14.6001087994197,4.2,9.0271997098676));
#25450=CARTESIAN_POINT('',(14.6001087994197,4.2,9.0135998549338));
#25451=CARTESIAN_POINT('',(14.6001087994197,4.15,9.0271997098676));
#25452=CARTESIAN_POINT('',(14.6001087994197,4.15,8.9728002901324));
#25453=CARTESIAN_POINT('',(14.6001087994197,4.15,9.0271997098676));
#25454=CARTESIAN_POINT('Origin',(14.2001215993515,4.15,9.03039967573437));
#25455=CARTESIAN_POINT('',(16.1000607996757,4.2,9.01519983786719));
#25456=CARTESIAN_POINT('',(14.6001087994197,4.15,9.0271997098676));
#25457=CARTESIAN_POINT('Origin',(14.4001151993856,4.15,9.));
#25458=CARTESIAN_POINT('Origin',(14.3217313010106,4.15,9.95411706725891));
#25459=CARTESIAN_POINT('',(14.3374673311006,4.2,10.0128447310642));
#25460=CARTESIAN_POINT('',(14.3217313010106,4.2,9.95411706725891));
#25461=CARTESIAN_POINT('',(14.3256653085331,4.2,9.96879898321025));
#25462=CARTESIAN_POINT('',(14.3374673311006,4.15,10.0128447310642));
#25463=CARTESIAN_POINT('',(14.3374673311006,4.15,10.0128447310642));
#25464=CARTESIAN_POINT('',(14.3217313010106,4.15,9.95411706725891));
#25465=CARTESIAN_POINT('',(14.3374673311006,4.15,10.0128447310642));
#25466=CARTESIAN_POINT('',(14.3217313010106,4.15,9.95411706725891));
#25467=CARTESIAN_POINT('Origin',(14.7089174798516,4.15,9.85368369175797));
#25468=CARTESIAN_POINT('',(14.7089174798516,4.2,9.85368369175797));
#25469=CARTESIAN_POINT('',(16.3544587399258,4.2,9.42684184587898));
#25470=CARTESIAN_POINT('',(14.7089174798516,4.15,9.85368369175797));
#25471=CARTESIAN_POINT('',(14.3217313010106,4.15,9.95411706725891));
#25472=CARTESIAN_POINT('',(14.7089174798516,4.15,9.85368369175797));
#25473=CARTESIAN_POINT('Origin',(14.7229970857216,4.15,9.90622949621533));
#25474=CARTESIAN_POINT('',(14.7229970857216,4.2,9.90622949621533));
#25475=CARTESIAN_POINT('',(14.7194771842541,4.2,9.89309304510103));
#25476=CARTESIAN_POINT('',(14.7229970857216,4.15,9.90622949621533));
#25477=CARTESIAN_POINT('',(14.7089174798516,4.15,9.85368369175797));
#25478=CARTESIAN_POINT('',(14.7229970857216,4.15,9.90622949621533));
#25479=CARTESIAN_POINT('Origin',(14.3374673311006,4.15,10.0128447310642));
#25480=CARTESIAN_POINT('',(16.1687336655503,4.2,9.5064223655321));
#25481=CARTESIAN_POINT('',(14.7229970857216,4.15,9.90622949621533));
#25482=CARTESIAN_POINT('Origin',(14.5223641933661,4.15,9.93326421141108));
#25483=CARTESIAN_POINT('Origin',(14.6940089358794,4.15,10.8736123088715));
#25484=CARTESIAN_POINT('',(14.7244086116138,4.2,10.926266091777));
#25485=CARTESIAN_POINT('',(14.6940089358794,4.2,10.8736123088715));
#25486=CARTESIAN_POINT('',(14.701608854813,4.2,10.8867757545979));
#25487=CARTESIAN_POINT('',(14.7244086116138,4.15,10.926266091777));
#25488=CARTESIAN_POINT('',(14.7244086116138,4.15,10.926266091777));
#25489=CARTESIAN_POINT('',(14.6940089358794,4.15,10.8736123088715));
#25490=CARTESIAN_POINT('',(14.7244086116138,4.15,10.926266091777));
#25491=CARTESIAN_POINT('',(14.6940089358794,4.15,10.8736123088715));
#25492=CARTESIAN_POINT('Origin',(15.0420079952605,4.15,10.6763899605692));
#25493=CARTESIAN_POINT('',(15.0420079952605,4.2,10.6763899605692));
#25494=CARTESIAN_POINT('',(16.5210039976303,4.2,9.83819498028462));
#25495=CARTESIAN_POINT('',(15.0420079952605,4.15,10.6763899605692));
#25496=CARTESIAN_POINT('',(14.6940089358794,4.15,10.8736123088715));
#25497=CARTESIAN_POINT('',(15.0420079952605,4.15,10.6763899605692));
#25498=CARTESIAN_POINT('Origin',(15.0692077051281,4.15,10.723501240011));
#25499=CARTESIAN_POINT('',(15.0692077051281,4.2,10.723501240011));
#25500=CARTESIAN_POINT('',(15.0624077776612,4.2,10.7117234201505));
#25501=CARTESIAN_POINT('',(15.0692077051281,4.15,10.723501240011));
#25502=CARTESIAN_POINT('',(15.0420079952605,4.15,10.6763899605692));
#25503=CARTESIAN_POINT('',(15.0692077051281,4.15,10.723501240011));
#25504=CARTESIAN_POINT('Origin',(14.7244086116138,4.15,10.926266091777));
#25505=CARTESIAN_POINT('',(16.3622043058069,4.2,9.96313304588852));
#25506=CARTESIAN_POINT('',(15.0692077051281,4.15,10.723501240011));
#25507=CARTESIAN_POINT('Origin',(14.8816083205038,4.15,10.8013280261731));
#25508=CARTESIAN_POINT('Origin',(15.2915843983595,4.15,11.6654239679252));
#25509=CARTESIAN_POINT('',(15.3345760320748,4.2,11.7084156016405));
#25510=CARTESIAN_POINT('',(15.2915843983595,4.2,11.6654239679252));
#25511=CARTESIAN_POINT('',(15.3023323067883,4.2,11.676171876354));
#25512=CARTESIAN_POINT('',(15.3345760320748,4.15,11.7084156016405));
#25513=CARTESIAN_POINT('',(15.3345760320748,4.15,11.7084156016405));
#25514=CARTESIAN_POINT('',(15.2915843983595,4.15,11.6654239679252));
#25515=CARTESIAN_POINT('',(15.3345760320748,4.15,11.7084156016405));
#25516=CARTESIAN_POINT('',(15.2915843983595,4.15,11.6654239679252));
#25517=CARTESIAN_POINT('Origin',(15.5766807774795,4.15,11.3848530239331));
#25518=CARTESIAN_POINT('',(15.5766807774795,4.2,11.3848530239331));
#25519=CARTESIAN_POINT('',(16.7883403887398,4.2,10.1924265119665));
#25520=CARTESIAN_POINT('',(15.5766807774795,4.15,11.3848530239331));
#25521=CARTESIAN_POINT('',(15.2915843983595,4.15,11.6654239679252));
#25522=CARTESIAN_POINT('',(15.5766807774795,4.15,11.3848530239331));
#25523=CARTESIAN_POINT('Origin',(15.6151469760669,4.15,11.4233192225205));
#25524=CARTESIAN_POINT('',(15.6151469760669,4.2,11.4233192225205));
#25525=CARTESIAN_POINT('',(15.6055304264201,4.2,11.4137026728736));
#25526=CARTESIAN_POINT('',(15.6151469760669,4.15,11.4233192225205));
#25527=CARTESIAN_POINT('',(15.5766807774795,4.15,11.3848530239331));
#25528=CARTESIAN_POINT('',(15.6151469760669,4.15,11.4233192225205));
#25529=CARTESIAN_POINT('Origin',(15.3345760320748,4.15,11.7084156016405));
#25530=CARTESIAN_POINT('',(16.6672880160374,4.2,10.3542078008203));
#25531=CARTESIAN_POINT('',(15.6151469760669,4.15,11.4233192225205));
#25532=CARTESIAN_POINT('Origin',(15.4533656872132,4.15,11.5466343127868));
#25533=CARTESIAN_POINT('Origin',(16.073733908223,4.15,12.2755913883862));
#25534=CARTESIAN_POINT('',(16.1263876911285,4.2,12.3059910641206));
#25535=CARTESIAN_POINT('',(16.073733908223,4.2,12.2755913883862));
#25536=CARTESIAN_POINT('',(16.0868973539493,4.2,12.2831913073198));
#25537=CARTESIAN_POINT('',(16.1263876911285,4.15,12.3059910641206));
#25538=CARTESIAN_POINT('',(16.1263876911285,4.15,12.3059910641206));
#25539=CARTESIAN_POINT('',(16.073733908223,4.15,12.2755913883862));
#25540=CARTESIAN_POINT('',(16.1263876911285,4.15,12.3059910641206));
#25541=CARTESIAN_POINT('',(16.073733908223,4.15,12.2755913883862));
#25542=CARTESIAN_POINT('Origin',(16.276498759989,4.15,11.9307922948719));
#25543=CARTESIAN_POINT('',(16.276498759989,4.2,11.9307922948719));
#25544=CARTESIAN_POINT('',(17.1382493799945,4.2,10.4653961474359));
#25545=CARTESIAN_POINT('',(16.276498759989,4.15,11.9307922948719));
#25546=CARTESIAN_POINT('',(16.073733908223,4.15,12.2755913883862));
#25547=CARTESIAN_POINT('',(16.276498759989,4.15,11.9307922948719));
#25548=CARTESIAN_POINT('Origin',(16.3236100394308,4.15,11.9579920047395));
#25549=CARTESIAN_POINT('',(16.3236100394308,4.2,11.9579920047395));
#25550=CARTESIAN_POINT('',(16.3118322195703,4.2,11.9511920772726));
#25551=CARTESIAN_POINT('',(16.3236100394308,4.15,11.9579920047395));
#25552=CARTESIAN_POINT('',(16.276498759989,4.15,11.9307922948719));
#25553=CARTESIAN_POINT('',(16.3236100394308,4.15,11.9579920047395));
#25554=CARTESIAN_POINT('Origin',(16.1263876911285,4.15,12.3059910641206));
#25555=CARTESIAN_POINT('',(17.0631938455643,4.2,10.6529955320603));
#25556=CARTESIAN_POINT('',(16.3236100394308,4.15,11.9579920047395));
#25557=CARTESIAN_POINT('Origin',(16.1986719738269,4.15,12.1183916794962));
#25558=CARTESIAN_POINT('Origin',(16.9871552689358,4.15,12.6625326688994));
#25559=CARTESIAN_POINT('',(17.0458829327411,4.2,12.6782686989894));
#25560=CARTESIAN_POINT('',(16.9871552689358,4.2,12.6625326688994));
#25561=CARTESIAN_POINT('',(17.0018371848871,4.2,12.6664666764219));
#25562=CARTESIAN_POINT('',(17.0458829327411,4.15,12.6782686989894));
#25563=CARTESIAN_POINT('',(17.0458829327411,4.15,12.6782686989894));
#25564=CARTESIAN_POINT('',(16.9871552689358,4.15,12.6625326688994));
#25565=CARTESIAN_POINT('',(17.0458829327411,4.15,12.6782686989894));
#25566=CARTESIAN_POINT('',(16.9871552689358,4.15,12.6625326688994));
#25567=CARTESIAN_POINT('Origin',(17.0937705037847,4.15,12.2770029142784));
#25568=CARTESIAN_POINT('',(17.0937705037847,4.2,12.2770029142784));
#25569=CARTESIAN_POINT('',(17.5468852518923,4.2,10.6385014571392));
#25570=CARTESIAN_POINT('',(17.0937705037847,4.15,12.2770029142784));
#25571=CARTESIAN_POINT('',(16.9871552689358,4.15,12.6625326688994));
#25572=CARTESIAN_POINT('',(17.0937705037847,4.15,12.2770029142784));
#25573=CARTESIAN_POINT('Origin',(17.146316308242,4.15,12.2910825201484));
#25574=CARTESIAN_POINT('',(17.146316308242,4.2,12.2910825201484));
#25575=CARTESIAN_POINT('',(17.1331798571277,4.2,12.2875626186809));
#25576=CARTESIAN_POINT('',(17.146316308242,4.15,12.2910825201484));
#25577=CARTESIAN_POINT('',(17.0937705037847,4.15,12.2770029142784));
#25578=CARTESIAN_POINT('',(17.146316308242,4.15,12.2910825201484));
#25579=CARTESIAN_POINT('Origin',(17.0458829327411,4.15,12.6782686989894));
#25580=CARTESIAN_POINT('',(17.5229414663705,4.2,10.8391343494947));
#25581=CARTESIAN_POINT('',(17.146316308242,4.15,12.2910825201484));
#25582=CARTESIAN_POINT('Origin',(17.0667357885889,4.15,12.4776358066339));
#25583=CARTESIAN_POINT('Origin',(17.9696003242656,4.15,12.7998784006485));
#25584=CARTESIAN_POINT('',(18.0303996757344,4.2,12.7998784006485));
#25585=CARTESIAN_POINT('',(17.9696003242656,4.2,12.7998784006485));
#25586=CARTESIAN_POINT('',(17.9848001621328,4.2,12.7998784006485));
#25587=CARTESIAN_POINT('',(18.0303996757344,4.15,12.7998784006485));
#25588=CARTESIAN_POINT('',(18.0303996757344,4.15,12.7998784006485));
#25589=CARTESIAN_POINT('',(17.9696003242656,4.15,12.7998784006485));
#25590=CARTESIAN_POINT('',(18.0303996757344,4.15,12.7998784006485));
#25591=CARTESIAN_POINT('',(17.9696003242656,4.15,12.7998784006485));
#25592=CARTESIAN_POINT('Origin',(17.9728002901324,4.15,12.3998912005803));
#25593=CARTESIAN_POINT('',(17.9728002901324,4.2,12.3998912005803));
#25594=CARTESIAN_POINT('',(17.9864001450662,4.2,10.6999456002901));
#25595=CARTESIAN_POINT('',(17.9728002901324,4.15,12.3998912005803));
#25596=CARTESIAN_POINT('',(17.9696003242656,4.15,12.7998784006485));
#25597=CARTESIAN_POINT('',(17.9728002901324,4.15,12.3998912005803));
#25598=CARTESIAN_POINT('Origin',(18.0271997098676,4.15,12.3998912005803));
#25599=CARTESIAN_POINT('',(18.0271997098676,4.2,12.3998912005803));
#25600=CARTESIAN_POINT('',(18.0135998549338,4.2,12.3998912005803));
#25601=CARTESIAN_POINT('',(18.0271997098676,4.15,12.3998912005803));
#25602=CARTESIAN_POINT('',(17.9728002901324,4.15,12.3998912005803));
#25603=CARTESIAN_POINT('',(18.0271997098676,4.15,12.3998912005803));
#25604=CARTESIAN_POINT('Origin',(18.0303996757344,4.15,12.7998784006485));
#25605=CARTESIAN_POINT('',(18.0151998378672,4.2,10.8999392003243));
#25606=CARTESIAN_POINT('',(18.0271997098676,4.15,12.3998912005803));
#25607=CARTESIAN_POINT('Origin',(18.,4.15,12.5998848006144));
#25608=CARTESIAN_POINT('Origin',(18.9541170672589,4.15,12.6782686989894));
#25609=CARTESIAN_POINT('',(19.0128447310642,4.2,12.6625326688994));
#25610=CARTESIAN_POINT('',(18.9541170672589,4.2,12.6782686989894));
#25611=CARTESIAN_POINT('',(18.9687989832102,4.2,12.6743346914669));
#25612=CARTESIAN_POINT('',(19.0128447310642,4.15,12.6625326688994));
#25613=CARTESIAN_POINT('',(19.0128447310642,4.15,12.6625326688994));
#25614=CARTESIAN_POINT('',(18.9541170672589,4.15,12.6782686989894));
#25615=CARTESIAN_POINT('',(19.0128447310642,4.15,12.6625326688994));
#25616=CARTESIAN_POINT('',(18.9541170672589,4.15,12.6782686989894));
#25617=CARTESIAN_POINT('Origin',(18.853683691758,4.15,12.2910825201484));
#25618=CARTESIAN_POINT('',(18.853683691758,4.2,12.2910825201484));
#25619=CARTESIAN_POINT('',(18.426841845879,4.2,10.6455412600742));
#25620=CARTESIAN_POINT('',(18.853683691758,4.15,12.2910825201484));
#25621=CARTESIAN_POINT('',(18.9541170672589,4.15,12.6782686989894));
#25622=CARTESIAN_POINT('',(18.853683691758,4.15,12.2910825201484));
#25623=CARTESIAN_POINT('Origin',(18.9062294962153,4.15,12.2770029142784));
#25624=CARTESIAN_POINT('',(18.9062294962153,4.2,12.2770029142784));
#25625=CARTESIAN_POINT('',(18.893093045101,4.2,12.2805228157459));
#25626=CARTESIAN_POINT('',(18.9062294962153,4.15,12.2770029142784));
#25627=CARTESIAN_POINT('',(18.853683691758,4.15,12.2910825201484));
#25628=CARTESIAN_POINT('',(18.9062294962153,4.15,12.2770029142784));
#25629=CARTESIAN_POINT('Origin',(19.0128447310642,4.15,12.6625326688994));
#25630=CARTESIAN_POINT('',(18.5064223655321,4.2,10.8312663344497));
#25631=CARTESIAN_POINT('',(18.9062294962153,4.15,12.2770029142784));
#25632=CARTESIAN_POINT('Origin',(18.9332642114111,4.15,12.4776358066339));
#25633=CARTESIAN_POINT('Origin',(19.8736123088715,4.15,12.3059910641206));
#25634=CARTESIAN_POINT('',(19.926266091777,4.2,12.2755913883862));
#25635=CARTESIAN_POINT('',(19.8736123088715,4.2,12.3059910641206));
#25636=CARTESIAN_POINT('',(19.8867757545979,4.2,12.298391145187));
#25637=CARTESIAN_POINT('',(19.926266091777,4.15,12.2755913883862));
#25638=CARTESIAN_POINT('',(19.926266091777,4.15,12.2755913883862));
#25639=CARTESIAN_POINT('',(19.8736123088715,4.15,12.3059910641206));
#25640=CARTESIAN_POINT('',(19.926266091777,4.15,12.2755913883862));
#25641=CARTESIAN_POINT('',(19.8736123088715,4.15,12.3059910641206));
#25642=CARTESIAN_POINT('Origin',(19.6763899605692,4.15,11.9579920047395));
#25643=CARTESIAN_POINT('',(19.6763899605692,4.2,11.9579920047395));
#25644=CARTESIAN_POINT('',(18.8381949802846,4.2,10.4789960023697));
#25645=CARTESIAN_POINT('',(19.6763899605692,4.15,11.9579920047395));
#25646=CARTESIAN_POINT('',(19.8736123088715,4.15,12.3059910641206));
#25647=CARTESIAN_POINT('',(19.6763899605692,4.15,11.9579920047395));
#25648=CARTESIAN_POINT('Origin',(19.723501240011,4.15,11.9307922948719));
#25649=CARTESIAN_POINT('',(19.723501240011,4.2,11.9307922948719));
#25650=CARTESIAN_POINT('',(19.7117234201506,4.2,11.9375922223388));
#25651=CARTESIAN_POINT('',(19.723501240011,4.15,11.9307922948719));
#25652=CARTESIAN_POINT('',(19.6763899605692,4.15,11.9579920047395));
#25653=CARTESIAN_POINT('',(19.723501240011,4.15,11.9307922948719));
#25654=CARTESIAN_POINT('Origin',(19.926266091777,4.15,12.2755913883862));
#25655=CARTESIAN_POINT('',(18.9631330458885,4.2,10.6377956941931));
#25656=CARTESIAN_POINT('',(19.723501240011,4.15,11.9307922948719));
#25657=CARTESIAN_POINT('Origin',(19.8013280261731,4.15,12.1183916794962));
#25658=CARTESIAN_POINT('Origin',(20.6654239679252,4.15,11.7084156016405));
#25659=CARTESIAN_POINT('',(20.7084156016405,4.2,11.6654239679252));
#25660=CARTESIAN_POINT('',(20.6654239679252,4.2,11.7084156016405));
#25661=CARTESIAN_POINT('',(20.676171876354,4.2,11.6976676932117));
#25662=CARTESIAN_POINT('',(20.7084156016405,4.15,11.6654239679252));
#25663=CARTESIAN_POINT('',(20.7084156016405,4.15,11.6654239679252));
#25664=CARTESIAN_POINT('',(20.6654239679252,4.15,11.7084156016405));
#25665=CARTESIAN_POINT('',(20.7084156016405,4.15,11.6654239679252));
#25666=CARTESIAN_POINT('',(20.6654239679252,4.15,11.7084156016405));
#25667=CARTESIAN_POINT('Origin',(20.3848530239331,4.15,11.4233192225205));
#25668=CARTESIAN_POINT('',(20.3848530239331,4.2,11.4233192225205));
#25669=CARTESIAN_POINT('',(19.1924265119665,4.2,10.2116596112602));
#25670=CARTESIAN_POINT('',(20.3848530239331,4.15,11.4233192225205));
#25671=CARTESIAN_POINT('',(20.6654239679252,4.15,11.7084156016405));
#25672=CARTESIAN_POINT('',(20.3848530239331,4.15,11.4233192225205));
#25673=CARTESIAN_POINT('Origin',(20.4233192225205,4.15,11.3848530239331));
#25674=CARTESIAN_POINT('',(20.4233192225205,4.2,11.3848530239331));
#25675=CARTESIAN_POINT('',(20.4137026728736,4.2,11.3944695735799));
#25676=CARTESIAN_POINT('',(20.4233192225205,4.15,11.3848530239331));
#25677=CARTESIAN_POINT('',(20.3848530239331,4.15,11.4233192225205));
#25678=CARTESIAN_POINT('',(20.4233192225205,4.15,11.3848530239331));
#25679=CARTESIAN_POINT('Origin',(20.7084156016405,4.15,11.6654239679252));
#25680=CARTESIAN_POINT('',(19.3542078008203,4.2,10.3327119839626));
#25681=CARTESIAN_POINT('',(20.4233192225205,4.15,11.3848530239331));
#25682=CARTESIAN_POINT('Origin',(20.5466343127868,4.15,11.5466343127868));
#25683=CARTESIAN_POINT('Origin',(21.2755913883862,4.15,10.926266091777));
#25684=CARTESIAN_POINT('',(21.3059910641206,4.2,10.8736123088715));
#25685=CARTESIAN_POINT('',(21.2755913883862,4.2,10.926266091777));
#25686=CARTESIAN_POINT('',(21.2831913073198,4.2,10.9131026460507));
#25687=CARTESIAN_POINT('',(21.3059910641206,4.15,10.8736123088715));
#25688=CARTESIAN_POINT('',(21.3059910641206,4.15,10.8736123088715));
#25689=CARTESIAN_POINT('',(21.2755913883862,4.15,10.926266091777));
#25690=CARTESIAN_POINT('',(21.3059910641206,4.15,10.8736123088715));
#25691=CARTESIAN_POINT('',(21.2755913883862,4.15,10.926266091777));
#25692=CARTESIAN_POINT('Origin',(20.9307922948719,4.15,10.723501240011));
#25693=CARTESIAN_POINT('',(20.9307922948719,4.2,10.723501240011));
#25694=CARTESIAN_POINT('',(19.4653961474359,4.2,9.86175062000551));
#25695=CARTESIAN_POINT('',(20.9307922948719,4.15,10.723501240011));
#25696=CARTESIAN_POINT('',(21.2755913883862,4.15,10.926266091777));
#25697=CARTESIAN_POINT('',(20.9307922948719,4.15,10.723501240011));
#25698=CARTESIAN_POINT('Origin',(20.9579920047395,4.15,10.6763899605692));
#25699=CARTESIAN_POINT('',(20.9579920047395,4.2,10.6763899605692));
#25700=CARTESIAN_POINT('',(20.9511920772726,4.2,10.6881677804297));
#25701=CARTESIAN_POINT('',(20.9579920047395,4.15,10.6763899605692));
#25702=CARTESIAN_POINT('',(20.9307922948719,4.15,10.723501240011));
#25703=CARTESIAN_POINT('',(20.9579920047395,4.15,10.6763899605692));
#25704=CARTESIAN_POINT('Origin',(21.3059910641206,4.15,10.8736123088715));
#25705=CARTESIAN_POINT('',(19.6529955320603,4.2,9.93680615443574));
#25706=CARTESIAN_POINT('',(20.9579920047395,4.15,10.6763899605692));
#25707=CARTESIAN_POINT('Origin',(21.1183916794962,4.15,10.8013280261731));
#25708=CARTESIAN_POINT('Origin',(21.6625326688994,4.15,10.0128447310642));
#25709=CARTESIAN_POINT('',(21.6782686989894,4.2,9.9541170672589));
#25710=CARTESIAN_POINT('',(21.6625326688994,4.2,10.0128447310642));
#25711=CARTESIAN_POINT('',(21.6664666764219,4.2,9.99816281511279));
#25712=CARTESIAN_POINT('',(21.6782686989894,4.15,9.9541170672589));
#25713=CARTESIAN_POINT('',(21.6782686989894,4.15,9.9541170672589));
#25714=CARTESIAN_POINT('',(21.6625326688994,4.15,10.0128447310642));
#25715=CARTESIAN_POINT('',(21.6782686989894,4.15,9.9541170672589));
#25716=CARTESIAN_POINT('',(21.6625326688994,4.15,10.0128447310642));
#25717=CARTESIAN_POINT('Origin',(21.2770029142784,4.15,9.90622949621533));
#25718=CARTESIAN_POINT('',(21.2770029142784,4.2,9.90622949621533));
#25719=CARTESIAN_POINT('',(19.6385014571392,4.2,9.45311474810766));
#25720=CARTESIAN_POINT('',(21.2770029142784,4.15,9.90622949621533));
#25721=CARTESIAN_POINT('',(21.6625326688994,4.15,10.0128447310642));
#25722=CARTESIAN_POINT('',(21.2770029142784,4.15,9.90622949621533));
#25723=CARTESIAN_POINT('Origin',(21.2910825201484,4.15,9.85368369175797));
#25724=CARTESIAN_POINT('',(21.2910825201484,4.2,9.85368369175797));
#25725=CARTESIAN_POINT('',(21.2875626186809,4.2,9.86682014287226));
#25726=CARTESIAN_POINT('',(21.2910825201484,4.15,9.85368369175797));
#25727=CARTESIAN_POINT('',(21.2770029142784,4.15,9.90622949621533));
#25728=CARTESIAN_POINT('',(21.2910825201484,4.15,9.85368369175797));
#25729=CARTESIAN_POINT('Origin',(21.6782686989894,4.15,9.9541170672589));
#25730=CARTESIAN_POINT('',(19.8391343494947,4.2,9.47705853362946));
#25731=CARTESIAN_POINT('',(21.2910825201484,4.15,9.85368369175797));
#25732=CARTESIAN_POINT('Origin',(21.4776358066339,4.15,9.93326421141108));
#25733=CARTESIAN_POINT('Origin',(21.7998784006485,4.15,9.03039967573437));
#25734=CARTESIAN_POINT('',(21.7998784006485,4.2,8.96960032426563));
#25735=CARTESIAN_POINT('',(21.7998784006485,4.2,9.03039967573437));
#25736=CARTESIAN_POINT('',(21.7998784006485,4.2,9.01519983786719));
#25737=CARTESIAN_POINT('',(21.7998784006485,4.15,8.96960032426563));
#25738=CARTESIAN_POINT('',(21.7998784006485,4.15,8.96960032426563));
#25739=CARTESIAN_POINT('',(21.7998784006485,4.15,9.03039967573437));
#25740=CARTESIAN_POINT('',(21.7998784006485,4.15,8.96960032426563));
#25741=CARTESIAN_POINT('',(21.7998784006485,4.15,9.03039967573437));
#25742=CARTESIAN_POINT('Origin',(21.3998912005803,4.15,9.0271997098676));
#25743=CARTESIAN_POINT('',(21.3998912005803,4.2,9.0271997098676));
#25744=CARTESIAN_POINT('',(19.6999456002901,4.2,9.0135998549338));
#25745=CARTESIAN_POINT('',(21.3998912005803,4.15,9.0271997098676));
#25746=CARTESIAN_POINT('',(21.7998784006485,4.15,9.03039967573437));
#25747=CARTESIAN_POINT('',(21.3998912005803,4.15,9.0271997098676));
#25748=CARTESIAN_POINT('Origin',(21.3998912005803,4.15,8.9728002901324));
#25749=CARTESIAN_POINT('',(21.3998912005803,4.2,8.9728002901324));
#25750=CARTESIAN_POINT('',(21.3998912005803,4.2,8.9864001450662));
#25751=CARTESIAN_POINT('',(21.3998912005803,4.15,8.9728002901324));
#25752=CARTESIAN_POINT('',(21.3998912005803,4.15,9.0271997098676));
#25753=CARTESIAN_POINT('',(21.3998912005803,4.15,8.9728002901324));
#25754=CARTESIAN_POINT('Origin',(21.7998784006485,4.15,8.96960032426563));
#25755=CARTESIAN_POINT('',(19.8999392003243,4.2,8.98480016213281));
#25756=CARTESIAN_POINT('',(21.3998912005803,4.15,8.9728002901324));
#25757=CARTESIAN_POINT('Origin',(21.5998848006144,4.15,9.));
#25758=CARTESIAN_POINT('Origin',(23.,3.7,14.));
#25759=CARTESIAN_POINT('',(22.775,3.8,14.));
#25760=CARTESIAN_POINT('Origin',(23.,3.8,14.));
#25761=CARTESIAN_POINT('',(22.775,4.2,14.));
#25762=CARTESIAN_POINT('',(22.775,3.7,14.));
#25763=CARTESIAN_POINT('Origin',(23.,4.2,14.));
#25764=CARTESIAN_POINT('Origin',(23.,3.7,4.));
#25765=CARTESIAN_POINT('',(22.775,3.8,4.));
#25766=CARTESIAN_POINT('Origin',(23.,3.8,4.));
#25767=CARTESIAN_POINT('',(22.775,4.2,4.));
#25768=CARTESIAN_POINT('',(22.775,3.7,4.));
#25769=CARTESIAN_POINT('Origin',(23.,4.2,4.));
#25770=CARTESIAN_POINT('Origin',(18.,3.7,9.));
#25771=CARTESIAN_POINT('',(16.475,3.8,9.));
#25772=CARTESIAN_POINT('Origin',(18.,3.8,9.));
#25773=CARTESIAN_POINT('',(16.475,4.2,9.));
#25774=CARTESIAN_POINT('',(16.475,3.7,9.));
#25775=CARTESIAN_POINT('Origin',(18.,4.2,9.));
#25776=CARTESIAN_POINT('Origin',(22.5,3.8,3.5));
#25777=CARTESIAN_POINT('',(22.5,3.8,9.5));
#25778=CARTESIAN_POINT('',(22.5,4.2,9.5));
#25779=CARTESIAN_POINT('',(22.5,3.8,9.5));
#25780=CARTESIAN_POINT('',(22.5,3.8,14.5));
#25781=CARTESIAN_POINT('',(22.5,3.8,14.5));
#25782=CARTESIAN_POINT('',(22.5,4.2,14.5));
#25783=CARTESIAN_POINT('',(22.5,3.8,14.5));
#25784=CARTESIAN_POINT('',(22.5,4.2,14.5));
#25785=CARTESIAN_POINT('Origin',(22.5,3.8,3.5));
#25786=CARTESIAN_POINT('',(22.5,4.2,8.5));
#25787=CARTESIAN_POINT('',(22.5,3.8,8.5));
#25788=CARTESIAN_POINT('',(22.5,3.8,8.5));
#25789=CARTESIAN_POINT('',(22.5,4.2,3.5));
#25790=CARTESIAN_POINT('',(22.5,4.2,14.5));
#25791=CARTESIAN_POINT('',(22.5,3.8,3.5));
#25792=CARTESIAN_POINT('',(22.5,3.8,3.5));
#25793=CARTESIAN_POINT('',(22.5,3.8,14.5));
#25794=CARTESIAN_POINT('Origin',(23.5,3.8,3.5));
#25795=CARTESIAN_POINT('',(23.5,3.8,3.5));
#25796=CARTESIAN_POINT('',(22.5,3.8,3.5));
#25797=CARTESIAN_POINT('',(23.5,4.2,3.5));
#25798=CARTESIAN_POINT('',(22.5,4.2,3.5));
#25799=CARTESIAN_POINT('',(23.5,3.8,3.5));
#25800=CARTESIAN_POINT('Origin',(23.5,3.8,14.5));
#25801=CARTESIAN_POINT('',(23.5,3.8,14.5));
#25802=CARTESIAN_POINT('',(23.5,3.8,3.5));
#25803=CARTESIAN_POINT('',(23.5,4.2,14.5));
#25804=CARTESIAN_POINT('',(23.5,4.2,3.5));
#25805=CARTESIAN_POINT('',(23.5,3.8,14.5));
#25806=CARTESIAN_POINT('Origin',(22.5,3.8,14.5));
#25807=CARTESIAN_POINT('',(23.5,3.8,14.5));
#25808=CARTESIAN_POINT('',(23.5,4.2,14.5));
#25809=CARTESIAN_POINT('Origin',(23.,3.8,8.5));
#25810=CARTESIAN_POINT('',(21.9686269665969,3.8,8.5));
#25811=CARTESIAN_POINT('',(18.,3.8,8.5));
#25812=CARTESIAN_POINT('',(21.9686269665969,4.2,8.5));
#25813=CARTESIAN_POINT('',(21.9686269665969,3.8,8.5));
#25814=CARTESIAN_POINT('',(18.,4.2,8.5));
#25815=CARTESIAN_POINT('Origin',(18.,3.8,9.));
#25816=CARTESIAN_POINT('',(21.9686269665969,3.8,9.5));
#25817=CARTESIAN_POINT('',(23.,3.8,9.5));
#25818=CARTESIAN_POINT('Origin',(18.,3.8,9.));
#25819=CARTESIAN_POINT('Origin',(18.,3.8,9.5));
#25820=CARTESIAN_POINT('',(21.9686269665969,4.2,9.5));
#25821=CARTESIAN_POINT('',(23.,4.2,9.5));
#25822=CARTESIAN_POINT('',(21.9686269665969,3.8,9.5));
#25823=CARTESIAN_POINT('Origin',(18.,4.2,9.));
#25824=CARTESIAN_POINT('Origin',(18.,4.2,9.));
#25825=CARTESIAN_POINT('Origin',(18.,3.8,9.));
#25826=CARTESIAN_POINT('',(0.,0.,0.));
#25827=CARTESIAN_POINT('Origin',(23.,-0.7,4.));
#25828=CARTESIAN_POINT('',(22.835,-0.6,4.));
#25829=CARTESIAN_POINT('Origin',(23.,-0.6,4.));
#25830=CARTESIAN_POINT('',(22.835,3.8,4.));
#25831=CARTESIAN_POINT('',(22.835,-0.7,4.));
#25832=CARTESIAN_POINT('Origin',(23.,3.8,4.));
#25833=CARTESIAN_POINT('Origin',(23.,-0.6,4.));
#25834=CARTESIAN_POINT('',(22.5,3.8,4.));
#25835=CARTESIAN_POINT('Origin',(23.,3.8,4.));
#25836=CARTESIAN_POINT('',(22.5,-0.6,4.));
#25837=CARTESIAN_POINT('',(22.5,-0.6,4.));
#25838=CARTESIAN_POINT('Origin',(23.,-0.6,4.));
#25839=CARTESIAN_POINT('Origin',(23.,3.8,4.));
#25840=CARTESIAN_POINT('Origin',(23.,-0.6,4.));
#25841=CARTESIAN_POINT('',(0.,0.,0.));
#25842=CARTESIAN_POINT('Origin',(23.,-0.7,14.));
#25843=CARTESIAN_POINT('',(22.835,-0.6,14.));
#25844=CARTESIAN_POINT('Origin',(23.,-0.6,14.));
#25845=CARTESIAN_POINT('',(22.835,3.8,14.));
#25846=CARTESIAN_POINT('',(22.835,-0.7,14.));
#25847=CARTESIAN_POINT('Origin',(23.,3.8,14.));
#25848=CARTESIAN_POINT('Origin',(23.,-0.6,14.));
#25849=CARTESIAN_POINT('',(22.5,3.8,14.));
#25850=CARTESIAN_POINT('Origin',(23.,3.8,14.));
#25851=CARTESIAN_POINT('',(22.5,-0.6,14.));
#25852=CARTESIAN_POINT('',(22.5,-0.6,14.));
#25853=CARTESIAN_POINT('Origin',(23.,-0.6,14.));
#25854=CARTESIAN_POINT('Origin',(23.,3.8,14.));
#25855=CARTESIAN_POINT('Origin',(23.,-0.6,14.));
#25856=CARTESIAN_POINT('',(0.,0.,0.));
#25857=CARTESIAN_POINT('Origin',(-2.,6.5,-0.5));
#25858=CARTESIAN_POINT('',(-2.,6.5,-0.5));
#25859=CARTESIAN_POINT('',(-4.,6.5,-0.5));
#25860=CARTESIAN_POINT('',(-2.,6.5,-0.5));
#25861=CARTESIAN_POINT('',(-4.,6.5,0.));
#25862=CARTESIAN_POINT('',(-4.,6.5,-0.5));
#25863=CARTESIAN_POINT('',(-2.,6.5,0.));
#25864=CARTESIAN_POINT('',(-2.,6.5,0.));
#25865=CARTESIAN_POINT('',(-2.,6.5,-0.5));
#25866=CARTESIAN_POINT('Origin',(-2.,-6.5,-0.5));
#25867=CARTESIAN_POINT('',(-2.,-6.5,-0.5));
#25868=CARTESIAN_POINT('',(-2.,-6.5,-0.5));
#25869=CARTESIAN_POINT('',(-2.,-6.5,0.));
#25870=CARTESIAN_POINT('',(-2.,-6.5,0.));
#25871=CARTESIAN_POINT('',(-2.,-6.5,-0.5));
#25872=CARTESIAN_POINT('Origin',(-4.,-6.5,-0.5));
#25873=CARTESIAN_POINT('',(-4.,-6.5,-0.5));
#25874=CARTESIAN_POINT('',(-4.,-6.5,-0.5));
#25875=CARTESIAN_POINT('',(-4.,-6.5,0.));
#25876=CARTESIAN_POINT('',(-4.,-6.5,0.));
#25877=CARTESIAN_POINT('',(-4.,-6.5,-0.5));
#25878=CARTESIAN_POINT('Origin',(-4.,6.5,-0.5));
#25879=CARTESIAN_POINT('',(-4.,6.5,-0.5));
#25880=CARTESIAN_POINT('',(-4.,6.5,0.));
#25881=CARTESIAN_POINT('Origin',(-3.,0.,0.));
#25882=CARTESIAN_POINT('Origin',(-3.,0.,-0.5));
#25883=CARTESIAN_POINT('',(0.,0.,0.));
#25884=CARTESIAN_POINT('Origin',(24.,6.5,-0.5));
#25885=CARTESIAN_POINT('',(24.,6.5,-0.5));
#25886=CARTESIAN_POINT('',(22.,6.5,-0.5));
#25887=CARTESIAN_POINT('',(24.,6.5,-0.5));
#25888=CARTESIAN_POINT('',(22.,6.5,0.));
#25889=CARTESIAN_POINT('',(22.,6.5,-0.5));
#25890=CARTESIAN_POINT('',(24.,6.5,0.));
#25891=CARTESIAN_POINT('',(24.,6.5,0.));
#25892=CARTESIAN_POINT('',(24.,6.5,-0.5));
#25893=CARTESIAN_POINT('Origin',(24.,-6.5,-0.5));
#25894=CARTESIAN_POINT('',(24.,-6.5,-0.5));
#25895=CARTESIAN_POINT('',(24.,-6.5,-0.5));
#25896=CARTESIAN_POINT('',(24.,-6.5,0.));
#25897=CARTESIAN_POINT('',(24.,-6.5,0.));
#25898=CARTESIAN_POINT('',(24.,-6.5,-0.5));
#25899=CARTESIAN_POINT('Origin',(22.,-6.5,-0.5));
#25900=CARTESIAN_POINT('',(22.,-6.5,-0.5));
#25901=CARTESIAN_POINT('',(22.,-6.5,-0.5));
#25902=CARTESIAN_POINT('',(22.,-6.5,0.));
#25903=CARTESIAN_POINT('',(22.,-6.5,0.));
#25904=CARTESIAN_POINT('',(22.,-6.5,-0.5));
#25905=CARTESIAN_POINT('Origin',(22.,6.5,-0.5));
#25906=CARTESIAN_POINT('',(22.,6.5,-0.5));
#25907=CARTESIAN_POINT('',(22.,6.5,0.));
#25908=CARTESIAN_POINT('Origin',(23.,0.,0.));
#25909=CARTESIAN_POINT('Origin',(23.,0.,-0.5));
#25910=CARTESIAN_POINT('',(0.,0.,0.));
#25911=CARTESIAN_POINT('Origin',(0.0866025403784439,-0.4,-0.15));
#25912=CARTESIAN_POINT('',(0.173205080756888,-0.4,0.));
#25913=CARTESIAN_POINT('',(0.0866025403784439,-0.4,-0.15));
#25914=CARTESIAN_POINT('',(0.173205080756888,-0.4,0.));
#25915=CARTESIAN_POINT('',(0.0866025403784439,-0.64,-0.15));
#25916=CARTESIAN_POINT('',(0.0866025403784439,-0.4,-0.15));
#25917=CARTESIAN_POINT('',(0.173205080756888,-0.64,0.));
#25918=CARTESIAN_POINT('',(0.173205080756888,-0.64,0.));
#25919=CARTESIAN_POINT('',(0.173205080756888,-0.4,0.));
#25920=CARTESIAN_POINT('Origin',(-0.0866025403784438,-0.4,-0.15));
#25921=CARTESIAN_POINT('',(-0.0866025403784438,-0.4,-0.15));
#25922=CARTESIAN_POINT('',(0.0866025403784439,-0.4,-0.15));
#25923=CARTESIAN_POINT('',(-0.0866025403784438,-0.64,-0.15));
#25924=CARTESIAN_POINT('',(-0.0866025403784438,-0.4,-0.15));
#25925=CARTESIAN_POINT('',(0.0866025403784439,-0.64,-0.15));
#25926=CARTESIAN_POINT('Origin',(-0.173205080756888,-0.4,-2.77555756156289E-17));
#25927=CARTESIAN_POINT('',(-0.173205080756888,-0.4,-2.12115047744981E-17));
#25928=CARTESIAN_POINT('',(-0.0866025403784438,-0.4,-0.15));
#25929=CARTESIAN_POINT('',(-0.173205080756888,-0.64,-2.77555756156289E-17));
#25930=CARTESIAN_POINT('',(-0.173205080756888,-0.4,-2.12115047744981E-17));
#25931=CARTESIAN_POINT('',(-0.0866025403784438,-0.64,-0.15));
#25932=CARTESIAN_POINT('Origin',(-0.0866025403784439,-0.4,0.15));
#25933=CARTESIAN_POINT('',(-0.0866025403784439,-0.4,0.15));
#25934=CARTESIAN_POINT('',(-0.173205080756888,-0.4,-2.12115047744981E-17));
#25935=CARTESIAN_POINT('',(-0.0866025403784439,-0.64,0.15));
#25936=CARTESIAN_POINT('',(-0.0866025403784439,-0.4,0.15));
#25937=CARTESIAN_POINT('',(-0.173205080756888,-0.64,-2.12115047744981E-17));
#25938=CARTESIAN_POINT('Origin',(0.0866025403784439,-0.4,0.15));
#25939=CARTESIAN_POINT('',(0.0866025403784439,-0.4,0.15));
#25940=CARTESIAN_POINT('',(-0.0866025403784439,-0.4,0.15));
#25941=CARTESIAN_POINT('',(0.0866025403784439,-0.64,0.15));
#25942=CARTESIAN_POINT('',(0.0866025403784439,-0.4,0.15));
#25943=CARTESIAN_POINT('',(-0.0866025403784439,-0.64,0.15));
#25944=CARTESIAN_POINT('Origin',(0.173205080756888,-0.4,0.));
#25945=CARTESIAN_POINT('',(0.0866025403784439,-0.4,0.15));
#25946=CARTESIAN_POINT('',(0.0866025403784439,-0.64,0.15));
#25947=CARTESIAN_POINT('Origin',(0.,-0.4,-2.77555756156289E-17));
#25948=CARTESIAN_POINT('Origin',(0.,-0.64,-2.77555756156289E-17));
#25949=CARTESIAN_POINT('Origin',(0.,-1.5,0.));
#25950=CARTESIAN_POINT('',(-0.2,-1.5,2.44929359829471E-17));
#25951=CARTESIAN_POINT('Origin',(0.,-1.5,0.));
#25952=CARTESIAN_POINT('',(-0.1954,-1.5,2.39295984553393E-17));
#25953=CARTESIAN_POINT('Origin',(0.,-1.5,0.));
#25954=CARTESIAN_POINT('Origin',(0.,-3.,0.));
#25955=CARTESIAN_POINT('',(-0.2,-3.,2.44929359829471E-17));
#25956=CARTESIAN_POINT('',(-0.2,-3.,2.44929359829471E-17));
#25957=CARTESIAN_POINT('Origin',(0.,-3.,0.));
#25958=CARTESIAN_POINT('Origin',(0.,-3.,0.));
#25959=CARTESIAN_POINT('Origin',(0.3,0.4,0.));
#25960=CARTESIAN_POINT('',(-0.3,0.4,-3.67394039744206E-17));
#25961=CARTESIAN_POINT('Origin',(0.,0.4,0.));
#25962=CARTESIAN_POINT('Origin',(0.,0.375,0.));
#25963=CARTESIAN_POINT('',(-0.35,0.35,-4.28626379701573E-17));
#25964=CARTESIAN_POINT('Origin',(0.,0.35,0.));
#25965=CARTESIAN_POINT('',(-0.325,0.375,-3.9801020972289E-17));
#25966=CARTESIAN_POINT('Origin',(0.,0.19,0.));
#25967=CARTESIAN_POINT('',(-0.35,0.03,-4.28626379701574E-17));
#25968=CARTESIAN_POINT('Origin',(0.,0.03,0.));
#25969=CARTESIAN_POINT('',(-0.35,0.19,-4.28626379701574E-17));
#25970=CARTESIAN_POINT('Origin',(0.,0.0149999999999999,0.));
#25971=CARTESIAN_POINT('',(-0.32,-3.29597460435593E-17,-3.91886975727153E-17));
#25972=CARTESIAN_POINT('Origin',(0.,0.,0.));
#25973=CARTESIAN_POINT('',(-0.335,0.0149999999999999,-4.10256677714363E-17));
#25974=CARTESIAN_POINT('Origin',(0.22,0.,0.));
#25975=CARTESIAN_POINT('',(-0.22,-6.93889390390723E-18,-2.69422295812418E-17));
#25976=CARTESIAN_POINT('Origin',(0.,0.,0.));
#25977=CARTESIAN_POINT('Origin',(0.,-0.02,0.));
#25978=CARTESIAN_POINT('',(-0.1954,-0.0492,2.39295984553393E-17));
#25979=CARTESIAN_POINT('Origin',(0.,-0.0492,0.));
#25980=CARTESIAN_POINT('',(-0.21,-0.02,-2.57175827820944E-17));
#25981=CARTESIAN_POINT('Origin',(0.,-0.8,0.));
#25982=CARTESIAN_POINT('',(-0.1954,-0.8,-2.39295984553393E-17));
#25983=CARTESIAN_POINT('',(0.,0.,0.));
#25984=CARTESIAN_POINT('',(0.,0.,0.));
#25985=CARTESIAN_POINT('Origin',(0.,4.6,9.));
#25986=CARTESIAN_POINT('',(-0.165,4.6,9.));
#25987=CARTESIAN_POINT('Origin',(0.,4.6,9.));
#25988=CARTESIAN_POINT('',(-0.165,6.,9.));
#25989=CARTESIAN_POINT('',(-0.165,4.6,9.));
#25990=CARTESIAN_POINT('Origin',(0.,6.,9.));
#25991=CARTESIAN_POINT('Origin',(0.,4.6,9.));
#25992=CARTESIAN_POINT('Origin',(-0.2,3.9,8.3));
#25993=CARTESIAN_POINT('',(-0.2,5.3,8.43431457505076));
#25994=CARTESIAN_POINT('',(-0.2,3.9,8.43431457505076));
#25995=CARTESIAN_POINT('',(-0.2,-3.6,8.43431457505076));
#25996=CARTESIAN_POINT('',(-0.2,5.3,8.65));
#25997=CARTESIAN_POINT('',(-0.2,5.3,8.65));
#25998=CARTESIAN_POINT('',(-0.2,3.9,8.65));
#25999=CARTESIAN_POINT('',(-0.2,3.9,8.65));
#26000=CARTESIAN_POINT('',(-0.2,3.9,8.65));
#26001=CARTESIAN_POINT('Origin',(0.,3.9,8.475));
#26002=CARTESIAN_POINT('',(0.2,3.9,8.43431457505076));
#26003=CARTESIAN_POINT('Origin',(0.,3.9,9.));
#26004=CARTESIAN_POINT('',(0.2,3.9,8.65));
#26005=CARTESIAN_POINT('',(0.2,3.9,8.65));
#26006=CARTESIAN_POINT('',(0.2,3.9,8.3));
#26007=CARTESIAN_POINT('Origin',(0.2,3.9,8.65));
#26008=CARTESIAN_POINT('',(0.2,5.3,8.43431457505076));
#26009=CARTESIAN_POINT('',(0.2,-3.6,8.43431457505076));
#26010=CARTESIAN_POINT('',(0.2,5.3,8.65));
#26011=CARTESIAN_POINT('',(0.2,3.9,8.65));
#26012=CARTESIAN_POINT('',(0.2,5.3,8.3));
#26013=CARTESIAN_POINT('Origin',(-0.2,3.9,8.65));
#26014=CARTESIAN_POINT('',(0.2,5.3,8.65));
#26015=CARTESIAN_POINT('Origin',(0.,5.3,8.475));
#26016=CARTESIAN_POINT('Origin',(0.,5.3,9.));
#26017=CARTESIAN_POINT('Origin',(-0.2,0.9,7.8));
#26018=CARTESIAN_POINT('',(-0.2,2.3,8.43431457505076));
#26019=CARTESIAN_POINT('',(-0.2,0.9,8.43431457505076));
#26020=CARTESIAN_POINT('',(-0.2,-3.6,8.43431457505076));
#26021=CARTESIAN_POINT('',(-0.2,2.3,8.65));
#26022=CARTESIAN_POINT('',(-0.2,2.3,8.65));
#26023=CARTESIAN_POINT('',(-0.2,0.9,8.65));
#26024=CARTESIAN_POINT('',(-0.2,0.9,8.65));
#26025=CARTESIAN_POINT('',(-0.2,0.9,8.65));
#26026=CARTESIAN_POINT('Origin',(0.,0.9,8.225));
#26027=CARTESIAN_POINT('',(0.2,0.9,8.43431457505076));
#26028=CARTESIAN_POINT('Origin',(0.,0.9,9.));
#26029=CARTESIAN_POINT('',(0.2,0.9,8.65));
#26030=CARTESIAN_POINT('',(0.2,0.9,8.65));
#26031=CARTESIAN_POINT('',(0.2,0.9,7.8));
#26032=CARTESIAN_POINT('Origin',(0.2,0.9,8.65));
#26033=CARTESIAN_POINT('',(0.2,2.3,8.43431457505076));
#26034=CARTESIAN_POINT('',(0.2,-3.6,8.43431457505076));
#26035=CARTESIAN_POINT('',(0.2,2.3,8.65));
#26036=CARTESIAN_POINT('',(0.2,0.9,8.65));
#26037=CARTESIAN_POINT('',(0.2,2.3,7.8));
#26038=CARTESIAN_POINT('Origin',(-0.2,0.9,8.65));
#26039=CARTESIAN_POINT('',(0.2,2.3,8.65));
#26040=CARTESIAN_POINT('Origin',(0.,2.3,8.225));
#26041=CARTESIAN_POINT('Origin',(0.,2.3,9.));
#26042=CARTESIAN_POINT('Origin',(0.,-0.4,9.));
#26043=CARTESIAN_POINT('',(-0.9,-0.4,9.));
#26044=CARTESIAN_POINT('Origin',(0.,-0.4,9.));
#26045=CARTESIAN_POINT('',(-0.6,-0.4,9.));
#26046=CARTESIAN_POINT('Origin',(0.,-0.4,9.));
#26047=CARTESIAN_POINT('Origin',(0.,-1.,9.));
#26048=CARTESIAN_POINT('',(-0.9,-1.,9.));
#26049=CARTESIAN_POINT('Origin',(0.,-1.,9.));
#26050=CARTESIAN_POINT('',(-0.6,-1.,9.));
#26051=CARTESIAN_POINT('Origin',(0.,-1.,9.));
#26052=CARTESIAN_POINT('Origin',(0.,-1.,9.));
#26053=CARTESIAN_POINT('',(-0.9,-1.,9.));
#26054=CARTESIAN_POINT('Origin',(0.,-3.6,9.));
#26055=CARTESIAN_POINT('',(-0.6,-3.6,9.));
#26056=CARTESIAN_POINT('',(-0.6,-3.6,9.));
#26057=CARTESIAN_POINT('Origin',(0.,-3.6,9.));
#26058=CARTESIAN_POINT('Origin',(0.,-3.6,9.));
#26059=CARTESIAN_POINT('',(-0.6,6.,9.));
#26060=CARTESIAN_POINT('Origin',(0.,6.,9.));
#26061=CARTESIAN_POINT('',(-0.6,-3.6,9.));
#26062=CARTESIAN_POINT('Origin',(0.,6.,9.));
#26063=CARTESIAN_POINT('Origin',(0.,-3.6,9.));
#26064=CARTESIAN_POINT('',(0.,0.,0.));
#26065=CARTESIAN_POINT('Origin',(0.,-0.4,9.));
#26066=CARTESIAN_POINT('',(-0.605,0.,9.));
#26067=CARTESIAN_POINT('Origin',(0.,0.,9.));
#26068=CARTESIAN_POINT('',(-0.605,-0.4,9.));
#26069=CARTESIAN_POINT('',(-0.605,-0.4,9.));
#26070=CARTESIAN_POINT('Origin',(0.,-0.4,9.));
#26071=CARTESIAN_POINT('Origin',(0.,-0.4,9.));
#26072=CARTESIAN_POINT('',(-0.9,0.,9.));
#26073=CARTESIAN_POINT('Origin',(0.,0.,9.));
#26074=CARTESIAN_POINT('',(-0.9,-0.4,9.));
#26075=CARTESIAN_POINT('',(-0.9,-0.4,9.));
#26076=CARTESIAN_POINT('Origin',(0.,-0.4,9.));
#26077=CARTESIAN_POINT('Origin',(0.,0.,9.));
#26078=CARTESIAN_POINT('Origin',(0.,-0.4,9.));
#26079=CARTESIAN_POINT('',(0.,0.,0.));
#26080=CARTESIAN_POINT('Origin',(0.,-2.8,9.));
#26081=CARTESIAN_POINT('',(-0.605,-2.,9.));
#26082=CARTESIAN_POINT('Origin',(0.,-2.,9.));
#26083=CARTESIAN_POINT('',(-0.605,-2.8,9.));
#26084=CARTESIAN_POINT('',(-0.605,-2.8,9.));
#26085=CARTESIAN_POINT('Origin',(0.,-2.8,9.));
#26086=CARTESIAN_POINT('Origin',(0.,-2.8,9.));
#26087=CARTESIAN_POINT('',(-0.9,-2.,9.));
#26088=CARTESIAN_POINT('Origin',(0.,-2.,9.));
#26089=CARTESIAN_POINT('',(-0.9,-2.8,9.));
#26090=CARTESIAN_POINT('',(-0.9,-2.8,9.));
#26091=CARTESIAN_POINT('Origin',(0.,-2.8,9.));
#26092=CARTESIAN_POINT('Origin',(0.,-2.,9.));
#26093=CARTESIAN_POINT('Origin',(0.,-2.8,9.));
#26094=CARTESIAN_POINT('',(0.,0.,0.));
#26095=CARTESIAN_POINT('Origin',(0.,-3.2,9.59));
#26096=CARTESIAN_POINT('',(0.133884278389952,-3.36178689687364,9.59));
#26097=CARTESIAN_POINT('',(0.133884278389952,-3.03821310312636,9.59));
#26098=CARTESIAN_POINT('',(0.133884278389952,-3.6,9.59));
#26099=CARTESIAN_POINT('Origin',(0.,-3.2,9.59));
#26100=CARTESIAN_POINT('Origin',(0.,-3.2,9.59));
#26101=CARTESIAN_POINT('',(-0.133884278389952,-3.36178689687364,9.59));
#26102=CARTESIAN_POINT('Ctrl Pts',(-0.133884278389951,-3.36178689687364,
9.59));
#26103=CARTESIAN_POINT('Ctrl Pts',(-0.118254395260798,-3.37472116821763,
9.59354677224418));
#26104=CARTESIAN_POINT('Ctrl Pts',(-0.100109787682297,-3.38579931658744,
9.59698224789957));
#26105=CARTESIAN_POINT('Ctrl Pts',(-0.054829872132519,-3.40463856105443,
9.6030741628997));
#26106=CARTESIAN_POINT('Ctrl Pts',(-0.0266020595922904,-3.41,9.605));
#26107=CARTESIAN_POINT('Ctrl Pts',(0.0266020595922903,-3.41,9.605));
#26108=CARTESIAN_POINT('Ctrl Pts',(0.0548298721325192,-3.40463856105443,
9.6030741628997));
#26109=CARTESIAN_POINT('Ctrl Pts',(0.100109787682297,-3.38579931658744,
9.59698224789957));
#26110=CARTESIAN_POINT('Ctrl Pts',(0.118254395260799,-3.37472116821763,
9.59354677224418));
#26111=CARTESIAN_POINT('Ctrl Pts',(0.133884278389952,-3.36178689687364,
9.59));
#26112=CARTESIAN_POINT('',(-0.21,-3.2,9.59));
#26113=CARTESIAN_POINT('Origin',(0.,-3.2,9.59));
#26114=CARTESIAN_POINT('',(-0.21,-3.2,9.97770138590472));
#26115=CARTESIAN_POINT('',(-0.21,-3.2,9.59));
#26116=CARTESIAN_POINT('',(0.21,-3.2,9.97770138590472));
#26117=CARTESIAN_POINT('Ctrl Pts',(0.21,-3.2,9.97770138590472));
#26118=CARTESIAN_POINT('Ctrl Pts',(0.21,-3.22645388258983,9.97770138590472));
#26119=CARTESIAN_POINT('Ctrl Pts',(0.204697017125528,-3.25461525830869,
9.97888646613217));
#26120=CARTESIAN_POINT('Ctrl Pts',(0.183241751515529,-3.30633042130174,
9.98312869991147));
#26121=CARTESIAN_POINT('Ctrl Pts',(0.167093586802906,-3.32989126129544,
9.98612044796649));
#26122=CARTESIAN_POINT('Ctrl Pts',(0.129892533236543,-3.36709231486181,
9.99170645156379));
#26123=CARTESIAN_POINT('Ctrl Pts',(0.106331154992714,-3.38324147510569,
9.99466914446598));
#26124=CARTESIAN_POINT('Ctrl Pts',(0.0546141143983532,-3.40469746372443,
9.99884449237241));
#26125=CARTESIAN_POINT('Ctrl Pts',(0.0264520736824499,-3.41,10.));
#26126=CARTESIAN_POINT('Ctrl Pts',(-0.0264520736824498,-3.41,10.));
#26127=CARTESIAN_POINT('Ctrl Pts',(-0.0546141143983531,-3.40469746372443,
9.99884449237241));
#26128=CARTESIAN_POINT('Ctrl Pts',(-0.106331154992714,-3.38324147510569,
9.99466914446598));
#26129=CARTESIAN_POINT('Ctrl Pts',(-0.129892533236543,-3.36709231486181,
9.99170645156379));
#26130=CARTESIAN_POINT('Ctrl Pts',(-0.167093586802906,-3.32989126129544,
9.98612044796649));
#26131=CARTESIAN_POINT('Ctrl Pts',(-0.183241751515529,-3.30633042130174,
9.98312869991147));
#26132=CARTESIAN_POINT('Ctrl Pts',(-0.204697017125528,-3.25461525830869,
9.97888646613217));
#26133=CARTESIAN_POINT('Ctrl Pts',(-0.21,-3.22645388258983,9.97770138590472));
#26134=CARTESIAN_POINT('Ctrl Pts',(-0.21,-3.2,9.97770138590472));
#26135=CARTESIAN_POINT('Ctrl Pts',(-0.21,-3.2,9.97770138590472));
#26136=CARTESIAN_POINT('Ctrl Pts',(-0.21,-3.17354611741017,9.97770138590472));
#26137=CARTESIAN_POINT('Ctrl Pts',(-0.204697017125528,-3.14538474169131,
9.97888646613217));
#26138=CARTESIAN_POINT('Ctrl Pts',(-0.183241751515529,-3.09366957869826,
9.98312869991147));
#26139=CARTESIAN_POINT('Ctrl Pts',(-0.167093586802906,-3.07010873870456,
9.98612044796649));
#26140=CARTESIAN_POINT('Ctrl Pts',(-0.129892533236543,-3.03290768513819,
9.99170645156379));
#26141=CARTESIAN_POINT('Ctrl Pts',(-0.106331154992714,-3.01675852489431,
9.99466914446598));
#26142=CARTESIAN_POINT('Ctrl Pts',(-0.0546141143983532,-2.99530253627557,
9.99884449237241));
#26143=CARTESIAN_POINT('Ctrl Pts',(-0.0264520736824499,-2.99,10.));
#26144=CARTESIAN_POINT('Ctrl Pts',(0.0264520736824498,-2.99,10.));
#26145=CARTESIAN_POINT('Ctrl Pts',(0.0546141143983531,-2.99530253627557,
9.99884449237241));
#26146=CARTESIAN_POINT('Ctrl Pts',(0.106331154992714,-3.01675852489431,
9.99466914446598));
#26147=CARTESIAN_POINT('Ctrl Pts',(0.129892533236543,-3.03290768513819,
9.99170645156379));
#26148=CARTESIAN_POINT('Ctrl Pts',(0.167093586802906,-3.07010873870456,
9.98612044796649));
#26149=CARTESIAN_POINT('Ctrl Pts',(0.183241751515529,-3.09366957869826,
9.98312869991147));
#26150=CARTESIAN_POINT('Ctrl Pts',(0.204697017125528,-3.14538474169131,
9.97888646613217));
#26151=CARTESIAN_POINT('Ctrl Pts',(0.21,-3.17354611741017,9.97770138590472));
#26152=CARTESIAN_POINT('Ctrl Pts',(0.21,-3.2,9.97770138590472));
#26153=CARTESIAN_POINT('',(-0.133884278389952,-3.03821310312636,9.59));
#26154=CARTESIAN_POINT('Origin',(0.,-3.2,9.59));
#26155=CARTESIAN_POINT('Ctrl Pts',(0.133884278389952,-3.03821310312636,
9.59));
#26156=CARTESIAN_POINT('Ctrl Pts',(0.118254395260799,-3.02527883178237,
9.59354677224418));
#26157=CARTESIAN_POINT('Ctrl Pts',(0.100109787682297,-3.01420068341256,
9.59698224789957));
#26158=CARTESIAN_POINT('Ctrl Pts',(0.054829872132519,-2.99536143894557,
9.6030741628997));
#26159=CARTESIAN_POINT('Ctrl Pts',(0.0266020595922904,-2.99,9.605));
#26160=CARTESIAN_POINT('Ctrl Pts',(-0.0266020595922903,-2.99,9.605));
#26161=CARTESIAN_POINT('Ctrl Pts',(-0.054829872132519,-2.99536143894557,
9.6030741628997));
#26162=CARTESIAN_POINT('Ctrl Pts',(-0.100109787682297,-3.01420068341256,
9.59698224789957));
#26163=CARTESIAN_POINT('Ctrl Pts',(-0.118254395260798,-3.02527883178237,
9.59354677224418));
#26164=CARTESIAN_POINT('Ctrl Pts',(-0.133884278389952,-3.03821310312636,
9.59));
#26165=CARTESIAN_POINT('Origin',(0.,-3.2,9.59));
#26166=CARTESIAN_POINT('',(-0.133884278389952,-3.6,9.59));
#26167=CARTESIAN_POINT('Origin',(0.,-3.6,9.));
#26168=CARTESIAN_POINT('',(-0.605,-2.8,9.));
#26169=CARTESIAN_POINT('Origin',(0.,-2.8,9.));
#26170=CARTESIAN_POINT('',(-0.605,-3.6,9.));
#26171=CARTESIAN_POINT('',(-0.605,-3.6,9.));
#26172=CARTESIAN_POINT('Origin',(0.,-3.6,9.));
#26173=CARTESIAN_POINT('Origin',(0.,-3.6,9.));
#26174=CARTESIAN_POINT('',(-1.,-2.8,9.));
#26175=CARTESIAN_POINT('Origin',(0.,-2.8,9.));
#26176=CARTESIAN_POINT('',(-1.,-3.6,9.));
#26177=CARTESIAN_POINT('',(-1.,-3.6,9.));
#26178=CARTESIAN_POINT('Origin',(0.,-3.6,9.));
#26179=CARTESIAN_POINT('Origin',(0.,-2.8,9.));
#26180=CARTESIAN_POINT('Origin',(0.,-3.6,9.));
#26181=CARTESIAN_POINT('',(0.,0.,0.));
#26182=CARTESIAN_POINT('Origin',(0.,3.9,13.));
#26183=CARTESIAN_POINT('',(-0.25,4.,13.));
#26184=CARTESIAN_POINT('Origin',(0.,4.,13.));
#26185=CARTESIAN_POINT('',(-0.25,4.8,13.));
#26186=CARTESIAN_POINT('',(-0.25,3.9,13.));
#26187=CARTESIAN_POINT('Origin',(0.,4.8,13.));
#26188=CARTESIAN_POINT('Origin',(-0.2,3.3,8.22));
#26189=CARTESIAN_POINT('',(-0.2,3.4,8.22));
#26190=CARTESIAN_POINT('',(-0.2,3.4,8.43431457505076));
#26191=CARTESIAN_POINT('',(-0.2,3.4,8.61));
#26192=CARTESIAN_POINT('',(-0.2,5.8,8.22));
#26193=CARTESIAN_POINT('',(-0.2,3.3,8.22));
#26194=CARTESIAN_POINT('',(-0.2,5.8,8.43431457505076));
#26195=CARTESIAN_POINT('',(-0.2,5.8,8.61));
#26196=CARTESIAN_POINT('',(-0.2,3.4,8.43431457505076));
#26197=CARTESIAN_POINT('Origin',(0.2,3.3,8.22));
#26198=CARTESIAN_POINT('',(0.2,3.4,8.22));
#26199=CARTESIAN_POINT('',(0.1,3.4,8.22));
#26200=CARTESIAN_POINT('',(0.2,5.8,8.22));
#26201=CARTESIAN_POINT('',(0.2,3.3,8.22));
#26202=CARTESIAN_POINT('',(0.1,5.8,8.22));
#26203=CARTESIAN_POINT('Origin',(0.2,3.3,9.));
#26204=CARTESIAN_POINT('',(0.2,3.4,8.43431457505076));
#26205=CARTESIAN_POINT('',(0.2,3.4,9.));
#26206=CARTESIAN_POINT('',(0.2,5.8,8.43431457505076));
#26207=CARTESIAN_POINT('',(0.2,3.4,8.43431457505076));
#26208=CARTESIAN_POINT('',(0.2,5.8,9.));
#26209=CARTESIAN_POINT('Origin',(0.,5.8,9.));
#26210=CARTESIAN_POINT('',(-1.25,5.8,9.));
#26211=CARTESIAN_POINT('Origin',(0.,5.8,9.));
#26212=CARTESIAN_POINT('Origin',(0.,5.8,9.));
#26213=CARTESIAN_POINT('Origin',(0.,3.4,9.));
#26214=CARTESIAN_POINT('Origin',(0.,3.4,9.));
#26215=CARTESIAN_POINT('Origin',(0.,4.,13.));
#26216=CARTESIAN_POINT('',(0.6,4.8,12.2));
#26217=CARTESIAN_POINT('',(0.6,4.,12.2));
#26218=CARTESIAN_POINT('',(0.6,4.,12.2));
#26219=CARTESIAN_POINT('',(-0.6,4.8,12.2));
#26220=CARTESIAN_POINT('Origin',(0.,4.8,13.));
#26221=CARTESIAN_POINT('',(-0.6,4.,12.2));
#26222=CARTESIAN_POINT('',(-0.6,4.,12.2));
#26223=CARTESIAN_POINT('Origin',(0.,4.,13.));
#26224=CARTESIAN_POINT('Origin',(0.,4.,11.));
#26225=CARTESIAN_POINT('',(-0.6,4.,10.0965856099731));
#26226=CARTESIAN_POINT('',(-0.6,4.,13.));
#26227=CARTESIAN_POINT('',(0.6,4.,10.0965856099731));
#26228=CARTESIAN_POINT('Origin',(0.,4.,9.));
#26229=CARTESIAN_POINT('',(0.6,4.,9.));
#26230=CARTESIAN_POINT('Origin',(-0.6,4.,9.));
#26231=CARTESIAN_POINT('',(-0.6,4.8,10.0965856099731));
#26232=CARTESIAN_POINT('',(-0.6,4.8,13.));
#26233=CARTESIAN_POINT('',(-0.6,3.4,10.0965856099731));
#26234=CARTESIAN_POINT('Origin',(0.,4.8,11.));
#26235=CARTESIAN_POINT('',(0.6,4.8,10.0965856099731));
#26236=CARTESIAN_POINT('',(0.6,4.8,9.));
#26237=CARTESIAN_POINT('Origin',(0.,4.8,9.));
#26238=CARTESIAN_POINT('Origin',(0.6,4.,13.));
#26239=CARTESIAN_POINT('',(0.6,3.4,10.0965856099731));
#26240=CARTESIAN_POINT('Origin',(0.,3.4,9.));
#26241=CARTESIAN_POINT('',(-1.25,3.4,9.));
#26242=CARTESIAN_POINT('',(-1.25,3.4,9.));
#26243=CARTESIAN_POINT('Origin',(0.,3.4,9.));
#26244=CARTESIAN_POINT('Origin',(0.,3.4,9.));
#26245=CARTESIAN_POINT('',(0.,0.,0.));
#26246=CARTESIAN_POINT('Origin',(0.,3.2,9.));
#26247=CARTESIAN_POINT('',(-0.605,3.4,9.));
#26248=CARTESIAN_POINT('Origin',(0.,3.4,9.));
#26249=CARTESIAN_POINT('',(-0.605,3.2,9.));
#26250=CARTESIAN_POINT('',(-0.605,3.2,9.));
#26251=CARTESIAN_POINT('Origin',(0.,3.2,9.));
#26252=CARTESIAN_POINT('Origin',(0.,3.2,9.));
#26253=CARTESIAN_POINT('',(-0.9,3.4,9.));
#26254=CARTESIAN_POINT('Origin',(0.,3.4,9.));
#26255=CARTESIAN_POINT('',(-0.9,3.2,9.));
#26256=CARTESIAN_POINT('',(-0.9,3.2,9.));
#26257=CARTESIAN_POINT('Origin',(0.,3.2,9.));
#26258=CARTESIAN_POINT('Origin',(0.,3.4,9.));
#26259=CARTESIAN_POINT('Origin',(0.,3.2,9.));
#26260=CARTESIAN_POINT('',(0.,0.,0.));
#26261=CARTESIAN_POINT('Origin',(0.,5.8,9.));
#26262=CARTESIAN_POINT('',(-0.605,6.,9.));
#26263=CARTESIAN_POINT('Origin',(0.,6.,9.));
#26264=CARTESIAN_POINT('',(-0.605,5.8,9.));
#26265=CARTESIAN_POINT('',(-0.605,5.8,9.));
#26266=CARTESIAN_POINT('Origin',(0.,5.8,9.));
#26267=CARTESIAN_POINT('Origin',(0.,5.8,9.));
#26268=CARTESIAN_POINT('',(-0.9,6.,9.));
#26269=CARTESIAN_POINT('Origin',(0.,6.,9.));
#26270=CARTESIAN_POINT('',(-0.9,5.8,9.));
#26271=CARTESIAN_POINT('',(-0.9,5.8,9.));
#26272=CARTESIAN_POINT('Origin',(0.,5.8,9.));
#26273=CARTESIAN_POINT('Origin',(0.,6.,9.));
#26274=CARTESIAN_POINT('Origin',(0.,5.8,9.));
#26275=CARTESIAN_POINT('',(0.,0.,0.));
#26276=CARTESIAN_POINT('Origin',(0.,6.,9.));
#26277=CARTESIAN_POINT('',(-0.225,6.2,9.));
#26278=CARTESIAN_POINT('Origin',(0.,6.2,9.));
#26279=CARTESIAN_POINT('',(-0.225,6.,9.));
#26280=CARTESIAN_POINT('',(-0.225,6.,9.));
#26281=CARTESIAN_POINT('Origin',(0.,6.,9.));
#26282=CARTESIAN_POINT('Origin',(0.,6.,9.));
#26283=CARTESIAN_POINT('',(-1.,6.2,9.));
#26284=CARTESIAN_POINT('Origin',(0.,6.2,9.));
#26285=CARTESIAN_POINT('',(-1.,6.,9.));
#26286=CARTESIAN_POINT('',(-1.,6.,9.));
#26287=CARTESIAN_POINT('Origin',(0.,6.,9.));
#26288=CARTESIAN_POINT('Origin',(0.,6.2,9.));
#26289=CARTESIAN_POINT('Origin',(0.,6.,9.));
#26290=CARTESIAN_POINT('',(0.,0.,0.));
#26291=CARTESIAN_POINT('Origin',(0.,4.8,13.));
#26292=CARTESIAN_POINT('',(-0.33,6.8,13.));
#26293=CARTESIAN_POINT('Origin',(0.,6.8,13.));
#26294=CARTESIAN_POINT('',(-0.33,4.8,13.));
#26295=CARTESIAN_POINT('',(-0.33,4.8,13.));
#26296=CARTESIAN_POINT('Origin',(0.,4.8,13.));
#26297=CARTESIAN_POINT('Origin',(0.,4.8,13.));
#26298=CARTESIAN_POINT('',(-0.4,6.8,13.));
#26299=CARTESIAN_POINT('Origin',(0.,6.8,13.));
#26300=CARTESIAN_POINT('',(-0.4,4.8,13.));
#26301=CARTESIAN_POINT('',(-0.4,4.8,13.));
#26302=CARTESIAN_POINT('Origin',(0.,4.8,13.));
#26303=CARTESIAN_POINT('Origin',(0.,6.8,13.));
#26304=CARTESIAN_POINT('Origin',(0.,4.8,13.));
#26305=CARTESIAN_POINT('',(0.,0.,0.));
#26306=CARTESIAN_POINT('Origin',(0.,0.,0.));
#26307=CARTESIAN_POINT('',(-0.32,0.16,3.91886975727153E-17));
#26308=CARTESIAN_POINT('Origin',(0.,0.16,0.));
#26309=CARTESIAN_POINT('',(-0.32,0.,3.91886975727153E-17));
#26310=CARTESIAN_POINT('',(-0.32,0.,3.91886975727153E-17));
#26311=CARTESIAN_POINT('Origin',(0.,0.,0.));
#26312=CARTESIAN_POINT('Origin',(0.,0.,0.));
#26313=CARTESIAN_POINT('',(-0.6,0.16,7.34788079488412E-17));
#26314=CARTESIAN_POINT('Origin',(0.,0.16,0.));
#26315=CARTESIAN_POINT('',(-0.6,0.,7.34788079488412E-17));
#26316=CARTESIAN_POINT('',(-0.6,0.,7.34788079488412E-17));
#26317=CARTESIAN_POINT('Origin',(0.,0.,0.));
#26318=CARTESIAN_POINT('Origin',(0.,0.16,0.));
#26319=CARTESIAN_POINT('Origin',(0.,0.,0.));
#26320=CARTESIAN_POINT('',(0.,0.,0.));
#26321=CARTESIAN_POINT('Origin',(0.144337567297406,-0.6,-0.25));
#26322=CARTESIAN_POINT('',(0.288675134594813,-0.6,0.));
#26323=CARTESIAN_POINT('',(0.144337567297406,-0.6,-0.25));
#26324=CARTESIAN_POINT('',(0.288675134594813,-0.6,0.));
#26325=CARTESIAN_POINT('',(0.144337567297406,-0.96,-0.25));
#26326=CARTESIAN_POINT('',(0.144337567297406,-0.6,-0.25));
#26327=CARTESIAN_POINT('',(0.288675134594813,-0.96,0.));
#26328=CARTESIAN_POINT('',(0.288675134594813,-0.96,0.));
#26329=CARTESIAN_POINT('',(0.288675134594813,-0.6,0.));
#26330=CARTESIAN_POINT('Origin',(-0.144337567297406,-0.6,-0.25));
#26331=CARTESIAN_POINT('',(-0.144337567297406,-0.6,-0.25));
#26332=CARTESIAN_POINT('',(0.144337567297406,-0.6,-0.25));
#26333=CARTESIAN_POINT('',(-0.144337567297406,-0.96,-0.25));
#26334=CARTESIAN_POINT('',(-0.144337567297406,-0.6,-0.25));
#26335=CARTESIAN_POINT('',(0.144337567297406,-0.96,-0.25));
#26336=CARTESIAN_POINT('Origin',(-0.288675134594813,-0.6,-8.32667268468867E-17));
#26337=CARTESIAN_POINT('',(-0.288675134594813,-0.6,-3.53525079574969E-17));
#26338=CARTESIAN_POINT('',(-0.144337567297406,-0.6,-0.25));
#26339=CARTESIAN_POINT('',(-0.288675134594813,-0.96,-5.55111512312578E-17));
#26340=CARTESIAN_POINT('',(-0.288675134594813,-0.6,-3.53525079574969E-17));
#26341=CARTESIAN_POINT('',(-0.144337567297406,-0.96,-0.25));
#26342=CARTESIAN_POINT('Origin',(-0.144337567297407,-0.6,0.25));
#26343=CARTESIAN_POINT('',(-0.144337567297407,-0.6,0.25));
#26344=CARTESIAN_POINT('',(-0.288675134594813,-0.6,-3.53525079574969E-17));
#26345=CARTESIAN_POINT('',(-0.144337567297407,-0.96,0.25));
#26346=CARTESIAN_POINT('',(-0.144337567297407,-0.6,0.25));
#26347=CARTESIAN_POINT('',(-0.288675134594813,-0.96,-3.53525079574969E-17));
#26348=CARTESIAN_POINT('Origin',(0.144337567297406,-0.6,0.25));
#26349=CARTESIAN_POINT('',(0.144337567297406,-0.6,0.25));
#26350=CARTESIAN_POINT('',(-0.144337567297407,-0.6,0.25));
#26351=CARTESIAN_POINT('',(0.144337567297406,-0.96,0.25));
#26352=CARTESIAN_POINT('',(0.144337567297406,-0.6,0.25));
#26353=CARTESIAN_POINT('',(-0.144337567297407,-0.96,0.25));
#26354=CARTESIAN_POINT('Origin',(0.288675134594813,-0.6,0.));
#26355=CARTESIAN_POINT('',(0.144337567297406,-0.6,0.25));
#26356=CARTESIAN_POINT('',(0.144337567297406,-0.96,0.25));
#26357=CARTESIAN_POINT('Origin',(0.,-0.6,0.));
#26358=CARTESIAN_POINT('Origin',(0.,-0.96,0.));
#26359=CARTESIAN_POINT('Origin',(0.,-2.4,0.));
#26360=CARTESIAN_POINT('',(-0.3,-2.4,3.67394039744206E-17));
#26361=CARTESIAN_POINT('Origin',(0.,-2.4,0.));
#26362=CARTESIAN_POINT('',(-0.2942,-2.4,3.60291088309151E-17));
#26363=CARTESIAN_POINT('Origin',(0.,-2.4,0.));
#26364=CARTESIAN_POINT('Origin',(0.,-3.,0.));
#26365=CARTESIAN_POINT('',(-0.3,-3.,3.67394039744206E-17));
#26366=CARTESIAN_POINT('',(-0.3,-3.,3.67394039744206E-17));
#26367=CARTESIAN_POINT('Origin',(0.,-3.,0.));
#26368=CARTESIAN_POINT('Origin',(0.,-3.,0.));
#26369=CARTESIAN_POINT('Origin',(0.45,0.6,0.));
#26370=CARTESIAN_POINT('',(-0.45,0.6,-5.51091059616309E-17));
#26371=CARTESIAN_POINT('Origin',(0.,0.6,0.));
#26372=CARTESIAN_POINT('Origin',(0.,0.575,0.));
#26373=CARTESIAN_POINT('',(-0.5,0.55,-6.12323399573677E-17));
#26374=CARTESIAN_POINT('Origin',(0.,0.55,0.));
#26375=CARTESIAN_POINT('',(-0.475,0.575,-5.81707229594993E-17));
#26376=CARTESIAN_POINT('Origin',(0.,0.29,0.));
#26377=CARTESIAN_POINT('',(-0.5,0.0299999999999998,-6.12323399573677E-17));
#26378=CARTESIAN_POINT('Origin',(0.,0.0299999999999998,0.));
#26379=CARTESIAN_POINT('',(-0.5,0.29,-6.12323399573677E-17));
#26380=CARTESIAN_POINT('Origin',(0.,0.0150000000000001,0.));
#26381=CARTESIAN_POINT('',(-0.47,7.11236625150491E-17,-5.75583995599256E-17));
#26382=CARTESIAN_POINT('Origin',(0.,0.,0.));
#26383=CARTESIAN_POINT('',(-0.485,0.0150000000000001,-5.93953697586466E-17));
#26384=CARTESIAN_POINT('Origin',(0.32,0.,0.));
#26385=CARTESIAN_POINT('',(-0.32,-6.93889390390723E-18,-3.91886975727153E-17));
#26386=CARTESIAN_POINT('Origin',(0.,0.,0.));
#26387=CARTESIAN_POINT('Origin',(0.,-0.02,0.));
#26388=CARTESIAN_POINT('',(-0.2942,-0.0515999999999999,3.60291088309151E-17));
#26389=CARTESIAN_POINT('Origin',(0.,-0.0515999999999999,0.));
#26390=CARTESIAN_POINT('',(-0.31,-0.02,-3.7964050773568E-17));
#26391=CARTESIAN_POINT('Origin',(0.,-1.24,0.));
#26392=CARTESIAN_POINT('',(-0.2942,-1.24,-3.60291088309151E-17));
#26393=CARTESIAN_POINT('',(0.,0.,0.));
#26394=CARTESIAN_POINT('',(0.,0.,0.));
#26395=CARTESIAN_POINT('Origin',(6.,1.8,9.));
#26396=CARTESIAN_POINT('',(5.835,1.8,9.));
#26397=CARTESIAN_POINT('Origin',(6.,1.8,9.));
#26398=CARTESIAN_POINT('',(5.835,3.2,9.));
#26399=CARTESIAN_POINT('',(5.835,1.8,9.));
#26400=CARTESIAN_POINT('Origin',(6.,3.2,9.));
#26401=CARTESIAN_POINT('Origin',(6.,1.8,9.));
#26402=CARTESIAN_POINT('Origin',(5.7,0.6,7.));
#26403=CARTESIAN_POINT('',(5.7,2.6,8.04606079858305));
#26404=CARTESIAN_POINT('',(5.7,0.6,8.04606079858305));
#26405=CARTESIAN_POINT('',(5.7,-3.6,8.04606079858305));
#26406=CARTESIAN_POINT('',(5.7,2.6,8.35));
#26407=CARTESIAN_POINT('',(5.7,2.6,8.35));
#26408=CARTESIAN_POINT('',(5.7,0.6,8.35));
#26409=CARTESIAN_POINT('',(5.7,0.6,8.35));
#26410=CARTESIAN_POINT('',(5.7,0.6,8.35));
#26411=CARTESIAN_POINT('Origin',(6.,0.6,7.675));
#26412=CARTESIAN_POINT('',(6.3,0.6,8.04606079858305));
#26413=CARTESIAN_POINT('Origin',(6.,0.6,9.));
#26414=CARTESIAN_POINT('',(6.3,0.6,8.35));
#26415=CARTESIAN_POINT('',(6.3,0.6,8.35));
#26416=CARTESIAN_POINT('',(6.3,0.6,7.));
#26417=CARTESIAN_POINT('Origin',(6.3,0.6,8.35));
#26418=CARTESIAN_POINT('',(6.3,2.6,8.04606079858305));
#26419=CARTESIAN_POINT('',(6.3,-3.6,8.04606079858305));
#26420=CARTESIAN_POINT('',(6.3,2.6,8.35));
#26421=CARTESIAN_POINT('',(6.3,0.6,8.35));
#26422=CARTESIAN_POINT('',(6.3,2.6,7.));
#26423=CARTESIAN_POINT('Origin',(5.7,0.6,8.35));
#26424=CARTESIAN_POINT('',(6.3,2.6,8.35));
#26425=CARTESIAN_POINT('Origin',(6.,2.6,7.675));
#26426=CARTESIAN_POINT('Origin',(6.,2.6,9.));
#26427=CARTESIAN_POINT('Origin',(6.,-0.4,9.));
#26428=CARTESIAN_POINT('',(4.7,-0.4,9.));
#26429=CARTESIAN_POINT('Origin',(6.,-0.4,9.));
#26430=CARTESIAN_POINT('',(5.,-0.4,9.));
#26431=CARTESIAN_POINT('Origin',(6.,-0.4,9.));
#26432=CARTESIAN_POINT('Origin',(6.,-0.8,9.));
#26433=CARTESIAN_POINT('',(4.7,-0.8,9.));
#26434=CARTESIAN_POINT('Origin',(6.,-0.8,9.));
#26435=CARTESIAN_POINT('',(5.,-0.8,9.));
#26436=CARTESIAN_POINT('Origin',(6.,-0.8,9.));
#26437=CARTESIAN_POINT('Origin',(6.,-0.8,9.));
#26438=CARTESIAN_POINT('',(4.7,-0.8,9.));
#26439=CARTESIAN_POINT('Origin',(6.,-3.6,9.));
#26440=CARTESIAN_POINT('',(5.,-3.6,9.));
#26441=CARTESIAN_POINT('',(5.,-3.6,9.));
#26442=CARTESIAN_POINT('Origin',(6.,-3.6,9.));
#26443=CARTESIAN_POINT('Origin',(6.,-3.6,9.));
#26444=CARTESIAN_POINT('',(5.,3.2,9.));
#26445=CARTESIAN_POINT('Origin',(6.,3.2,9.));
#26446=CARTESIAN_POINT('',(5.,-3.6,9.));
#26447=CARTESIAN_POINT('Origin',(6.,3.2,9.));
#26448=CARTESIAN_POINT('Origin',(6.,-3.6,9.));
#26449=CARTESIAN_POINT('',(0.,0.,0.));
#26450=CARTESIAN_POINT('Origin',(6.,-0.4,9.));
#26451=CARTESIAN_POINT('',(4.995,0.,9.));
#26452=CARTESIAN_POINT('Origin',(6.,0.,9.));
#26453=CARTESIAN_POINT('',(4.995,-0.4,9.));
#26454=CARTESIAN_POINT('',(4.995,-0.4,9.));
#26455=CARTESIAN_POINT('Origin',(6.,-0.4,9.));
#26456=CARTESIAN_POINT('Origin',(6.,-0.4,9.));
#26457=CARTESIAN_POINT('',(4.7,0.,9.));
#26458=CARTESIAN_POINT('Origin',(6.,0.,9.));
#26459=CARTESIAN_POINT('',(4.7,-0.4,9.));
#26460=CARTESIAN_POINT('',(4.7,-0.4,9.));
#26461=CARTESIAN_POINT('Origin',(6.,-0.4,9.));
#26462=CARTESIAN_POINT('Origin',(6.,0.,9.));
#26463=CARTESIAN_POINT('Origin',(6.,-0.4,9.));
#26464=CARTESIAN_POINT('',(0.,0.,0.));
#26465=CARTESIAN_POINT('Origin',(6.,-2.8,9.));
#26466=CARTESIAN_POINT('',(4.995,-2.2,9.));
#26467=CARTESIAN_POINT('Origin',(6.,-2.2,9.));
#26468=CARTESIAN_POINT('',(4.995,-2.8,9.));
#26469=CARTESIAN_POINT('',(4.995,-2.8,9.));
#26470=CARTESIAN_POINT('Origin',(6.,-2.8,9.));
#26471=CARTESIAN_POINT('Origin',(6.,-2.8,9.));
#26472=CARTESIAN_POINT('',(4.7,-2.2,9.));
#26473=CARTESIAN_POINT('Origin',(6.,-2.2,9.));
#26474=CARTESIAN_POINT('',(4.7,-2.8,9.));
#26475=CARTESIAN_POINT('',(4.7,-2.8,9.));
#26476=CARTESIAN_POINT('Origin',(6.,-2.8,9.));
#26477=CARTESIAN_POINT('Origin',(6.,-2.2,9.));
#26478=CARTESIAN_POINT('Origin',(6.,-2.8,9.));
#26479=CARTESIAN_POINT('',(0.,0.,0.));
#26480=CARTESIAN_POINT('Origin',(6.,-3.2,9.99));
#26481=CARTESIAN_POINT('',(6.17298843892005,-3.31905880899792,9.99));
#26482=CARTESIAN_POINT('',(6.17298843892005,-3.08094119100208,9.99));
#26483=CARTESIAN_POINT('',(6.17298843892005,-3.6,9.99));
#26484=CARTESIAN_POINT('Origin',(6.,-3.2,9.99));
#26485=CARTESIAN_POINT('Origin',(6.,-3.2,9.99));
#26486=CARTESIAN_POINT('',(5.82701156107995,-3.31905880899792,9.99));
#26487=CARTESIAN_POINT('Ctrl Pts',(5.82701156107995,-3.31905880899792,9.99));
#26488=CARTESIAN_POINT('Ctrl Pts',(5.83440513468869,-3.3298014223953,9.99129192197638));
#26489=CARTESIAN_POINT('Ctrl Pts',(5.8427028612744,-3.33968770937275,9.99265394943905));
#26490=CARTESIAN_POINT('Ctrl Pts',(5.87010792615492,-3.36709277425327,9.9967480843909));
#26491=CARTESIAN_POINT('Ctrl Pts',(5.89366983224072,-3.38324205633295,9.99969589327638));
#26492=CARTESIAN_POINT('Ctrl Pts',(5.94538709536759,-3.40469779396491,10.0038502947236));
#26493=CARTESIAN_POINT('Ctrl Pts',(5.97354876917015,-3.41,10.005));
#26494=CARTESIAN_POINT('Ctrl Pts',(6.02645123082985,-3.41,10.005));
#26495=CARTESIAN_POINT('Ctrl Pts',(6.05461290463241,-3.40469779396491,10.0038502947236));
#26496=CARTESIAN_POINT('Ctrl Pts',(6.10633016775928,-3.38324205633295,9.99969589327638));
#26497=CARTESIAN_POINT('Ctrl Pts',(6.12989207384508,-3.36709277425327,9.9967480843909));
#26498=CARTESIAN_POINT('Ctrl Pts',(6.1572971387256,-3.33968770937275,9.99265394943905));
#26499=CARTESIAN_POINT('Ctrl Pts',(6.16559486531131,-3.3298014223953,9.99129192197638));
#26500=CARTESIAN_POINT('Ctrl Pts',(6.17298843892005,-3.31905880899792,9.99));
#26501=CARTESIAN_POINT('',(5.79,-3.2,9.99));
#26502=CARTESIAN_POINT('Origin',(6.,-3.2,9.99));
#26503=CARTESIAN_POINT('',(5.79,-3.2,10.38416039533));
#26504=CARTESIAN_POINT('',(5.79,-3.2,9.99));
#26505=CARTESIAN_POINT('',(6.21,-3.2,10.38416039533));
#26506=CARTESIAN_POINT('Ctrl Pts',(6.21,-3.2,10.38416039533));
#26507=CARTESIAN_POINT('Ctrl Pts',(6.21,-3.22641116018715,10.38416039533));
#26508=CARTESIAN_POINT('Ctrl Pts',(6.20471354911189,-3.2545550596171,10.3849944296993));
#26509=CARTESIAN_POINT('Ctrl Pts',(6.18326999585849,-3.30628264999174,10.3879947099895));
#26510=CARTESIAN_POINT('Ctrl Pts',(6.16711503760643,-3.32986981049192,10.3901162943626));
#26511=CARTESIAN_POINT('Ctrl Pts',(6.12987013519678,-3.36711471290157,10.394089123191));
#26512=CARTESIAN_POINT('Ctrl Pts',(6.10628283459019,-3.38326992585508,10.3962002442067));
#26513=CARTESIAN_POINT('Ctrl Pts',(6.05455476560391,-3.40471366447292,10.3991765222353));
#26514=CARTESIAN_POINT('Ctrl Pts',(6.02641069968078,-3.41,10.4));
#26515=CARTESIAN_POINT('Ctrl Pts',(5.97358930031922,-3.41,10.4));
#26516=CARTESIAN_POINT('Ctrl Pts',(5.94544523439609,-3.40471366447292,10.3991765222353));
#26517=CARTESIAN_POINT('Ctrl Pts',(5.89371716540981,-3.38326992585508,10.3962002442067));
#26518=CARTESIAN_POINT('Ctrl Pts',(5.87012986480322,-3.36711471290157,10.394089123191));
#26519=CARTESIAN_POINT('Ctrl Pts',(5.83288496239357,-3.32986981049192,10.3901162943626));
#26520=CARTESIAN_POINT('Ctrl Pts',(5.81673000414151,-3.30628264999174,10.3879947099895));
#26521=CARTESIAN_POINT('Ctrl Pts',(5.79528645088811,-3.2545550596171,10.3849944296993));
#26522=CARTESIAN_POINT('Ctrl Pts',(5.79,-3.22641116018715,10.38416039533));
#26523=CARTESIAN_POINT('Ctrl Pts',(5.79,-3.2,10.38416039533));
#26524=CARTESIAN_POINT('Ctrl Pts',(5.79,-3.2,10.38416039533));
#26525=CARTESIAN_POINT('Ctrl Pts',(5.79,-3.17358883981285,10.38416039533));
#26526=CARTESIAN_POINT('Ctrl Pts',(5.79528645088811,-3.1454449403829,10.3849944296993));
#26527=CARTESIAN_POINT('Ctrl Pts',(5.81673000414151,-3.09371735000826,10.3879947099895));
#26528=CARTESIAN_POINT('Ctrl Pts',(5.83288496239357,-3.07013018950808,10.3901162943626));
#26529=CARTESIAN_POINT('Ctrl Pts',(5.87012986480322,-3.03288528709844,10.394089123191));
#26530=CARTESIAN_POINT('Ctrl Pts',(5.89371716540981,-3.01673007414492,10.3962002442067));
#26531=CARTESIAN_POINT('Ctrl Pts',(5.94544523439609,-2.99528633552708,10.3991765222353));
#26532=CARTESIAN_POINT('Ctrl Pts',(5.97358930031922,-2.99,10.4));
#26533=CARTESIAN_POINT('Ctrl Pts',(6.02641069968078,-2.99,10.4));
#26534=CARTESIAN_POINT('Ctrl Pts',(6.05455476560391,-2.99528633552708,10.3991765222353));
#26535=CARTESIAN_POINT('Ctrl Pts',(6.10628283459019,-3.01673007414492,10.3962002442067));
#26536=CARTESIAN_POINT('Ctrl Pts',(6.12987013519678,-3.03288528709844,10.394089123191));
#26537=CARTESIAN_POINT('Ctrl Pts',(6.16711503760643,-3.07013018950808,10.3901162943626));
#26538=CARTESIAN_POINT('Ctrl Pts',(6.18326999585849,-3.09371735000826,10.3879947099895));
#26539=CARTESIAN_POINT('Ctrl Pts',(6.20471354911189,-3.1454449403829,10.3849944296993));
#26540=CARTESIAN_POINT('Ctrl Pts',(6.21,-3.17358883981285,10.38416039533));
#26541=CARTESIAN_POINT('Ctrl Pts',(6.21,-3.2,10.38416039533));
#26542=CARTESIAN_POINT('',(5.82701156107995,-3.08094119100208,9.99));
#26543=CARTESIAN_POINT('Origin',(6.,-3.2,9.99));
#26544=CARTESIAN_POINT('Ctrl Pts',(6.17298843892005,-3.08094119100208,9.99));
#26545=CARTESIAN_POINT('Ctrl Pts',(6.16559486531131,-3.0701985776047,9.99129192197638));
#26546=CARTESIAN_POINT('Ctrl Pts',(6.15729713872561,-3.06031229062725,9.99265394943905));
#26547=CARTESIAN_POINT('Ctrl Pts',(6.12989207384508,-3.03290722574673,9.9967480843909));
#26548=CARTESIAN_POINT('Ctrl Pts',(6.10633016775929,-3.01675794366705,9.99969589327638));
#26549=CARTESIAN_POINT('Ctrl Pts',(6.05461290463241,-2.99530220603509,10.0038502947236));
#26550=CARTESIAN_POINT('Ctrl Pts',(6.02645123082985,-2.99,10.005));
#26551=CARTESIAN_POINT('Ctrl Pts',(5.97354876917015,-2.99,10.005));
#26552=CARTESIAN_POINT('Ctrl Pts',(5.94538709536759,-2.99530220603509,10.0038502947236));
#26553=CARTESIAN_POINT('Ctrl Pts',(5.89366983224072,-3.01675794366705,9.99969589327638));
#26554=CARTESIAN_POINT('Ctrl Pts',(5.87010792615492,-3.03290722574673,9.9967480843909));
#26555=CARTESIAN_POINT('Ctrl Pts',(5.8427028612744,-3.06031229062725,9.99265394943905));
#26556=CARTESIAN_POINT('Ctrl Pts',(5.83440513468869,-3.0701985776047,9.99129192197638));
#26557=CARTESIAN_POINT('Ctrl Pts',(5.82701156107995,-3.08094119100208,9.99));
#26558=CARTESIAN_POINT('Origin',(6.,-3.2,9.99));
#26559=CARTESIAN_POINT('',(5.82701156107995,-3.6,9.99));
#26560=CARTESIAN_POINT('Origin',(6.,-3.6,9.));
#26561=CARTESIAN_POINT('',(4.995,-2.8,9.));
#26562=CARTESIAN_POINT('Origin',(6.,-2.8,9.));
#26563=CARTESIAN_POINT('',(4.995,-3.6,9.));
#26564=CARTESIAN_POINT('',(4.995,-3.6,9.));
#26565=CARTESIAN_POINT('Origin',(6.,-3.6,9.));
#26566=CARTESIAN_POINT('Origin',(6.,-3.6,9.));
#26567=CARTESIAN_POINT('',(4.6,-2.8,9.));
#26568=CARTESIAN_POINT('Origin',(6.,-2.8,9.));
#26569=CARTESIAN_POINT('',(4.6,-3.6,9.));
#26570=CARTESIAN_POINT('',(4.6,-3.6,9.));
#26571=CARTESIAN_POINT('Origin',(6.,-3.6,9.));
#26572=CARTESIAN_POINT('Origin',(6.,-2.8,9.));
#26573=CARTESIAN_POINT('Origin',(6.,-3.6,9.));
#26574=CARTESIAN_POINT('',(0.,0.,0.));
#26575=CARTESIAN_POINT('Origin',(6.,3.2,9.));
#26576=CARTESIAN_POINT('',(5.775,3.4,9.));
#26577=CARTESIAN_POINT('Origin',(6.,3.4,9.));
#26578=CARTESIAN_POINT('',(5.775,3.2,9.));
#26579=CARTESIAN_POINT('',(5.775,3.2,9.));
#26580=CARTESIAN_POINT('Origin',(6.,3.2,9.));
#26581=CARTESIAN_POINT('Origin',(6.,3.2,9.));
#26582=CARTESIAN_POINT('',(4.6,3.4,9.));
#26583=CARTESIAN_POINT('Origin',(6.,3.4,9.));
#26584=CARTESIAN_POINT('',(4.6,3.2,9.));
#26585=CARTESIAN_POINT('',(4.6,3.2,9.));
#26586=CARTESIAN_POINT('Origin',(6.,3.2,9.));
#26587=CARTESIAN_POINT('Origin',(6.,3.4,9.));
#26588=CARTESIAN_POINT('Origin',(6.,3.2,9.));
#26589=CARTESIAN_POINT('',(0.,0.,0.));
#26590=CARTESIAN_POINT('',(0.,0.,0.));
#26591=CARTESIAN_POINT('Origin',(12.,1.8,9.));
#26592=CARTESIAN_POINT('',(11.835,1.8,9.));
#26593=CARTESIAN_POINT('Origin',(12.,1.8,9.));
#26594=CARTESIAN_POINT('',(11.835,3.2,9.));
#26595=CARTESIAN_POINT('',(11.835,1.8,9.));
#26596=CARTESIAN_POINT('Origin',(12.,3.2,9.));
#26597=CARTESIAN_POINT('Origin',(12.,1.8,9.));
#26598=CARTESIAN_POINT('Origin',(11.8,0.9,7.8));
#26599=CARTESIAN_POINT('',(11.8,2.3,8.43431457505076));
#26600=CARTESIAN_POINT('',(11.8,0.9,8.43431457505076));
#26601=CARTESIAN_POINT('',(11.8,-3.6,8.43431457505076));
#26602=CARTESIAN_POINT('',(11.8,2.3,8.65));
#26603=CARTESIAN_POINT('',(11.8,2.3,8.65));
#26604=CARTESIAN_POINT('',(11.8,0.9,8.65));
#26605=CARTESIAN_POINT('',(11.8,0.9,8.65));
#26606=CARTESIAN_POINT('',(11.8,0.9,8.65));
#26607=CARTESIAN_POINT('Origin',(12.,0.9,8.225));
#26608=CARTESIAN_POINT('',(12.2,0.9,8.43431457505076));
#26609=CARTESIAN_POINT('Origin',(12.,0.9,9.));
#26610=CARTESIAN_POINT('',(12.2,0.9,8.65));
#26611=CARTESIAN_POINT('',(12.2,0.9,8.65));
#26612=CARTESIAN_POINT('',(12.2,0.9,7.8));
#26613=CARTESIAN_POINT('Origin',(12.2,0.9,8.65));
#26614=CARTESIAN_POINT('',(12.2,2.3,8.43431457505076));
#26615=CARTESIAN_POINT('',(12.2,-3.6,8.43431457505076));
#26616=CARTESIAN_POINT('',(12.2,2.3,8.65));
#26617=CARTESIAN_POINT('',(12.2,0.9,8.65));
#26618=CARTESIAN_POINT('',(12.2,2.3,7.8));
#26619=CARTESIAN_POINT('Origin',(11.8,0.9,8.65));
#26620=CARTESIAN_POINT('',(12.2,2.3,8.65));
#26621=CARTESIAN_POINT('Origin',(12.,2.3,8.225));
#26622=CARTESIAN_POINT('Origin',(12.,2.3,9.));
#26623=CARTESIAN_POINT('Origin',(12.,-0.4,9.));
#26624=CARTESIAN_POINT('',(11.1,-0.4,9.));
#26625=CARTESIAN_POINT('Origin',(12.,-0.4,9.));
#26626=CARTESIAN_POINT('',(11.4,-0.4,9.));
#26627=CARTESIAN_POINT('Origin',(12.,-0.4,9.));
#26628=CARTESIAN_POINT('Origin',(12.,-1.,9.));
#26629=CARTESIAN_POINT('',(11.1,-1.,9.));
#26630=CARTESIAN_POINT('Origin',(12.,-1.,9.));
#26631=CARTESIAN_POINT('',(11.4,-1.,9.));
#26632=CARTESIAN_POINT('Origin',(12.,-1.,9.));
#26633=CARTESIAN_POINT('Origin',(12.,-1.,9.));
#26634=CARTESIAN_POINT('',(11.1,-1.,9.));
#26635=CARTESIAN_POINT('Origin',(12.,-3.6,9.));
#26636=CARTESIAN_POINT('',(11.4,-3.6,9.));
#26637=CARTESIAN_POINT('',(11.4,-3.6,9.));
#26638=CARTESIAN_POINT('Origin',(12.,-3.6,9.));
#26639=CARTESIAN_POINT('Origin',(12.,-3.6,9.));
#26640=CARTESIAN_POINT('',(11.4,3.2,9.));
#26641=CARTESIAN_POINT('Origin',(12.,3.2,9.));
#26642=CARTESIAN_POINT('',(11.4,-3.6,9.));
#26643=CARTESIAN_POINT('Origin',(12.,3.2,9.));
#26644=CARTESIAN_POINT('Origin',(12.,-3.6,9.));
#26645=CARTESIAN_POINT('',(0.,0.,0.));
#26646=CARTESIAN_POINT('Origin',(12.,-0.4,9.));
#26647=CARTESIAN_POINT('',(11.395,0.,9.));
#26648=CARTESIAN_POINT('Origin',(12.,0.,9.));
#26649=CARTESIAN_POINT('',(11.395,-0.4,9.));
#26650=CARTESIAN_POINT('',(11.395,-0.4,9.));
#26651=CARTESIAN_POINT('Origin',(12.,-0.4,9.));
#26652=CARTESIAN_POINT('Origin',(12.,-0.4,9.));
#26653=CARTESIAN_POINT('',(11.1,0.,9.));
#26654=CARTESIAN_POINT('Origin',(12.,0.,9.));
#26655=CARTESIAN_POINT('',(11.1,-0.4,9.));
#26656=CARTESIAN_POINT('',(11.1,-0.4,9.));
#26657=CARTESIAN_POINT('Origin',(12.,-0.4,9.));
#26658=CARTESIAN_POINT('Origin',(12.,0.,9.));
#26659=CARTESIAN_POINT('Origin',(12.,-0.4,9.));
#26660=CARTESIAN_POINT('',(0.,0.,0.));
#26661=CARTESIAN_POINT('Origin',(12.,-2.8,9.));
#26662=CARTESIAN_POINT('',(11.395,-2.,9.));
#26663=CARTESIAN_POINT('Origin',(12.,-2.,9.));
#26664=CARTESIAN_POINT('',(11.395,-2.8,9.));
#26665=CARTESIAN_POINT('',(11.395,-2.8,9.));
#26666=CARTESIAN_POINT('Origin',(12.,-2.8,9.));
#26667=CARTESIAN_POINT('Origin',(12.,-2.8,9.));
#26668=CARTESIAN_POINT('',(11.1,-2.,9.));
#26669=CARTESIAN_POINT('Origin',(12.,-2.,9.));
#26670=CARTESIAN_POINT('',(11.1,-2.8,9.));
#26671=CARTESIAN_POINT('',(11.1,-2.8,9.));
#26672=CARTESIAN_POINT('Origin',(12.,-2.8,9.));
#26673=CARTESIAN_POINT('Origin',(12.,-2.,9.));
#26674=CARTESIAN_POINT('Origin',(12.,-2.8,9.));
#26675=CARTESIAN_POINT('',(0.,0.,0.));
#26676=CARTESIAN_POINT('Origin',(12.,-3.2,9.59));
#26677=CARTESIAN_POINT('',(12.1338842783899,-3.36178689687366,9.59));
#26678=CARTESIAN_POINT('',(12.1338842783899,-3.03821310312634,9.59));
#26679=CARTESIAN_POINT('',(12.13388427839,-3.6,9.59));
#26680=CARTESIAN_POINT('Origin',(12.,-3.2,9.59));
#26681=CARTESIAN_POINT('Origin',(12.,-3.2,9.59));
#26682=CARTESIAN_POINT('',(11.8661157216101,-3.36178689687366,9.59));
#26683=CARTESIAN_POINT('Ctrl Pts',(11.8661157216101,-3.36178689687366,9.59000000000001));
#26684=CARTESIAN_POINT('Ctrl Pts',(11.8817456047392,-3.37472116821764,9.59354677224418));
#26685=CARTESIAN_POINT('Ctrl Pts',(11.8998902123177,-3.38579931658744,9.59698224789958));
#26686=CARTESIAN_POINT('Ctrl Pts',(11.9451701278675,-3.40463856105443,9.60307416289971));
#26687=CARTESIAN_POINT('Ctrl Pts',(11.9733979404077,-3.41,9.605));
#26688=CARTESIAN_POINT('Ctrl Pts',(12.0266020595923,-3.41,9.605));
#26689=CARTESIAN_POINT('Ctrl Pts',(12.0548298721325,-3.40463856105443,9.60307416289971));
#26690=CARTESIAN_POINT('Ctrl Pts',(12.1001097876823,-3.38579931658744,9.59698224789958));
#26691=CARTESIAN_POINT('Ctrl Pts',(12.1182543952608,-3.37472116821764,9.59354677224418));
#26692=CARTESIAN_POINT('Ctrl Pts',(12.1338842783899,-3.36178689687366,9.59000000000001));
#26693=CARTESIAN_POINT('',(11.79,-3.2,9.59));
#26694=CARTESIAN_POINT('Origin',(12.,-3.2,9.59));
#26695=CARTESIAN_POINT('',(11.79,-3.2,9.97770138590471));
#26696=CARTESIAN_POINT('',(11.79,-3.2,9.59));
#26697=CARTESIAN_POINT('',(12.21,-3.2,9.97770138590471));
#26698=CARTESIAN_POINT('Ctrl Pts',(12.21,-3.2,9.97770138590471));
#26699=CARTESIAN_POINT('Ctrl Pts',(12.21,-3.22645388258983,9.97770138590471));
#26700=CARTESIAN_POINT('Ctrl Pts',(12.2046970171255,-3.25461525830869,9.97888646613217));
#26701=CARTESIAN_POINT('Ctrl Pts',(12.1832417515155,-3.30633042130174,9.98312869991148));
#26702=CARTESIAN_POINT('Ctrl Pts',(12.1670935868029,-3.32989126129544,9.98612044796649));
#26703=CARTESIAN_POINT('Ctrl Pts',(12.1298925332365,-3.36709231486181,9.99170645156379));
#26704=CARTESIAN_POINT('Ctrl Pts',(12.1063311549927,-3.38324147510569,9.99466914446598));
#26705=CARTESIAN_POINT('Ctrl Pts',(12.0546141143984,-3.40469746372443,9.99884449237241));
#26706=CARTESIAN_POINT('Ctrl Pts',(12.0264520736824,-3.41,10.));
#26707=CARTESIAN_POINT('Ctrl Pts',(11.9735479263176,-3.41,10.));
#26708=CARTESIAN_POINT('Ctrl Pts',(11.9453858856017,-3.40469746372443,9.99884449237241));
#26709=CARTESIAN_POINT('Ctrl Pts',(11.8936688450073,-3.38324147510569,9.99466914446598));
#26710=CARTESIAN_POINT('Ctrl Pts',(11.8701074667635,-3.36709231486181,9.99170645156379));
#26711=CARTESIAN_POINT('Ctrl Pts',(11.8329064131971,-3.32989126129544,9.98612044796649));
#26712=CARTESIAN_POINT('Ctrl Pts',(11.8167582484845,-3.30633042130174,9.98312869991148));
#26713=CARTESIAN_POINT('Ctrl Pts',(11.7953029828745,-3.25461525830869,9.97888646613217));
#26714=CARTESIAN_POINT('Ctrl Pts',(11.79,-3.22645388258983,9.97770138590472));
#26715=CARTESIAN_POINT('Ctrl Pts',(11.79,-3.2,9.97770138590472));
#26716=CARTESIAN_POINT('Ctrl Pts',(11.79,-3.2,9.97770138590471));
#26717=CARTESIAN_POINT('Ctrl Pts',(11.79,-3.17354611741017,9.97770138590471));
#26718=CARTESIAN_POINT('Ctrl Pts',(11.7953029828745,-3.14538474169131,9.97888646613217));
#26719=CARTESIAN_POINT('Ctrl Pts',(11.8167582484845,-3.09366957869826,9.98312869991148));
#26720=CARTESIAN_POINT('Ctrl Pts',(11.8329064131971,-3.07010873870456,9.98612044796649));
#26721=CARTESIAN_POINT('Ctrl Pts',(11.8701074667635,-3.03290768513819,9.99170645156379));
#26722=CARTESIAN_POINT('Ctrl Pts',(11.8936688450073,-3.01675852489431,9.99466914446598));
#26723=CARTESIAN_POINT('Ctrl Pts',(11.9453858856016,-2.99530253627557,9.99884449237241));
#26724=CARTESIAN_POINT('Ctrl Pts',(11.9735479263176,-2.99,10.));
#26725=CARTESIAN_POINT('Ctrl Pts',(12.0264520736824,-2.99,10.));
#26726=CARTESIAN_POINT('Ctrl Pts',(12.0546141143984,-2.99530253627557,9.99884449237241));
#26727=CARTESIAN_POINT('Ctrl Pts',(12.1063311549927,-3.01675852489431,9.99466914446598));
#26728=CARTESIAN_POINT('Ctrl Pts',(12.1298925332365,-3.03290768513819,9.99170645156379));
#26729=CARTESIAN_POINT('Ctrl Pts',(12.1670935868029,-3.07010873870456,9.98612044796649));
#26730=CARTESIAN_POINT('Ctrl Pts',(12.1832417515155,-3.09366957869826,9.98312869991147));
#26731=CARTESIAN_POINT('Ctrl Pts',(12.2046970171255,-3.14538474169131,9.97888646613217));
#26732=CARTESIAN_POINT('Ctrl Pts',(12.21,-3.17354611741017,9.97770138590471));
#26733=CARTESIAN_POINT('Ctrl Pts',(12.21,-3.2,9.97770138590471));
#26734=CARTESIAN_POINT('',(11.8661157216101,-3.03821310312634,9.59));
#26735=CARTESIAN_POINT('Origin',(12.,-3.2,9.59));
#26736=CARTESIAN_POINT('Ctrl Pts',(12.1338842783899,-3.03821310312634,9.59000000000001));
#26737=CARTESIAN_POINT('Ctrl Pts',(12.1182543952608,-3.02527883178236,9.59354677224418));
#26738=CARTESIAN_POINT('Ctrl Pts',(12.1001097876823,-3.01420068341256,9.59698224789958));
#26739=CARTESIAN_POINT('Ctrl Pts',(12.0548298721325,-2.99536143894557,9.60307416289971));
#26740=CARTESIAN_POINT('Ctrl Pts',(12.0266020595923,-2.99,9.605));
#26741=CARTESIAN_POINT('Ctrl Pts',(11.9733979404077,-2.99,9.605));
#26742=CARTESIAN_POINT('Ctrl Pts',(11.9451701278675,-2.99536143894557,9.60307416289971));
#26743=CARTESIAN_POINT('Ctrl Pts',(11.8998902123177,-3.01420068341256,9.59698224789958));
#26744=CARTESIAN_POINT('Ctrl Pts',(11.8817456047392,-3.02527883178236,9.59354677224418));
#26745=CARTESIAN_POINT('Ctrl Pts',(11.8661157216101,-3.03821310312634,9.59000000000001));
#26746=CARTESIAN_POINT('Origin',(12.,-3.2,9.59));
#26747=CARTESIAN_POINT('',(11.86611572161,-3.6,9.59));
#26748=CARTESIAN_POINT('Origin',(12.,-3.6,9.));
#26749=CARTESIAN_POINT('',(11.395,-2.8,9.));
#26750=CARTESIAN_POINT('Origin',(12.,-2.8,9.));
#26751=CARTESIAN_POINT('',(11.395,-3.6,9.));
#26752=CARTESIAN_POINT('',(11.395,-3.6,9.));
#26753=CARTESIAN_POINT('Origin',(12.,-3.6,9.));
#26754=CARTESIAN_POINT('Origin',(12.,-3.6,9.));
#26755=CARTESIAN_POINT('',(11.,-2.8,9.));
#26756=CARTESIAN_POINT('Origin',(12.,-2.8,9.));
#26757=CARTESIAN_POINT('',(11.,-3.6,9.));
#26758=CARTESIAN_POINT('',(11.,-3.6,9.));
#26759=CARTESIAN_POINT('Origin',(12.,-3.6,9.));
#26760=CARTESIAN_POINT('Origin',(12.,-2.8,9.));
#26761=CARTESIAN_POINT('Origin',(12.,-3.6,9.));
#26762=CARTESIAN_POINT('',(0.,0.,0.));
#26763=CARTESIAN_POINT('Origin',(12.,3.2,9.));
#26764=CARTESIAN_POINT('',(11.775,3.4,9.));
#26765=CARTESIAN_POINT('Origin',(12.,3.4,9.));
#26766=CARTESIAN_POINT('',(11.775,3.2,9.));
#26767=CARTESIAN_POINT('',(11.775,3.2,9.));
#26768=CARTESIAN_POINT('Origin',(12.,3.2,9.));
#26769=CARTESIAN_POINT('Origin',(12.,3.2,9.));
#26770=CARTESIAN_POINT('',(11.,3.4,9.));
#26771=CARTESIAN_POINT('Origin',(12.,3.4,9.));
#26772=CARTESIAN_POINT('',(11.,3.2,9.));
#26773=CARTESIAN_POINT('',(11.,3.2,9.));
#26774=CARTESIAN_POINT('Origin',(12.,3.2,9.));
#26775=CARTESIAN_POINT('Origin',(12.,3.4,9.));
#26776=CARTESIAN_POINT('Origin',(12.,3.2,9.));
#26777=CARTESIAN_POINT('',(0.,0.,0.));
#26778=CARTESIAN_POINT('Origin',(0.2,0.,0.));
#26779=CARTESIAN_POINT('',(0.2,2.2,-0.78));
#26780=CARTESIAN_POINT('',(0.2,2.2,-0.565685424949238));
#26781=CARTESIAN_POINT('',(0.2,2.2,0.));
#26782=CARTESIAN_POINT('',(0.2,-1.,-0.78));
#26783=CARTESIAN_POINT('',(0.2,0.,-0.78));
#26784=CARTESIAN_POINT('',(0.2,-1.,-0.565685424949238));
#26785=CARTESIAN_POINT('',(0.2,-1.,0.));
#26786=CARTESIAN_POINT('',(0.2,0.,-0.565685424949238));
#26787=CARTESIAN_POINT('Origin',(0.2,0.,-0.78));
#26788=CARTESIAN_POINT('',(-0.2,2.2,-0.78));
#26789=CARTESIAN_POINT('',(0.1,2.2,-0.78));
#26790=CARTESIAN_POINT('',(-0.2,-1.,-0.78));
#26791=CARTESIAN_POINT('',(-0.2,0.,-0.78));
#26792=CARTESIAN_POINT('',(0.1,-1.,-0.78));
#26793=CARTESIAN_POINT('Origin',(-0.2,0.,-0.78));
#26794=CARTESIAN_POINT('',(-0.2,2.2,-0.565685424949238));
#26795=CARTESIAN_POINT('',(-0.2,2.2,-0.39));
#26796=CARTESIAN_POINT('',(-0.2,-1.,-0.565685424949238));
#26797=CARTESIAN_POINT('',(-0.2,0.,-0.565685424949238));
#26798=CARTESIAN_POINT('',(-0.2,-1.,-0.39));
#26799=CARTESIAN_POINT('Origin',(0.,-1.,0.));
#26800=CARTESIAN_POINT('',(1.60662857109684,-1.,0.693717979106306));
#26801=CARTESIAN_POINT('',(1.5055822144029,-1.,0.892032620296856));
#26802=CARTESIAN_POINT('Origin',(0.,-1.,0.));
#26803=CARTESIAN_POINT('',(1.81978687191668,-1.,1.23627494547115));
#26804=CARTESIAN_POINT('Ctrl Pts',(1.5055822144029,-1.,0.892032620296856));
#26805=CARTESIAN_POINT('Ctrl Pts',(1.50980486806688,-1.,0.894452006964544));
#26806=CARTESIAN_POINT('Ctrl Pts',(1.51805569590094,-1.,0.899185047483511));
#26807=CARTESIAN_POINT('Ctrl Pts',(1.52984849887993,-1.,0.905967409625651));
#26808=CARTESIAN_POINT('Ctrl Pts',(1.54440491149498,-1.,0.914375919026456));
#26809=CARTESIAN_POINT('Ctrl Pts',(1.56065988578893,-1.,0.923832188944341));
#26810=CARTESIAN_POINT('Ctrl Pts',(1.57499388382243,-1.,0.932246680108685));
#26811=CARTESIAN_POINT('Ctrl Pts',(1.58744937487176,-1.,0.939646377893399));
#26812=CARTESIAN_POINT('Ctrl Pts',(1.59810042043673,-1.,0.946078063315257));
#26813=CARTESIAN_POINT('Ctrl Pts',(1.60706069896936,-1.,0.951613284356035));
#26814=CARTESIAN_POINT('Ctrl Pts',(1.61449324337085,-1.,0.956354422920671));
#26815=CARTESIAN_POINT('Ctrl Pts',(1.62061638140221,-1.,0.960438326101729));
#26816=CARTESIAN_POINT('Ctrl Pts',(1.62571930670187,-1.,0.964046107040536));
#26817=CARTESIAN_POINT('Ctrl Pts',(1.63013849959461,-1.,0.967387853230345));
#26818=CARTESIAN_POINT('Ctrl Pts',(1.63420665729798,-1.,0.970669715997509));
#26819=CARTESIAN_POINT('Ctrl Pts',(1.63820952658144,-1.,0.974066058287419));
#26820=CARTESIAN_POINT('Ctrl Pts',(1.64233990826687,-1.,0.977689794119417));
#26821=CARTESIAN_POINT('Ctrl Pts',(1.64665139190656,-1.,0.981562530939489));
#26822=CARTESIAN_POINT('Ctrl Pts',(1.65110016612638,-1.,0.985642622920821));
#26823=CARTESIAN_POINT('Ctrl Pts',(1.65559044289699,-1.,0.989855627854165));
#26824=CARTESIAN_POINT('Ctrl Pts',(1.66001553809947,-1.,0.994121836661306));
#26825=CARTESIAN_POINT('Ctrl Pts',(1.66430758030376,-1.,0.998389654952758));
#26826=CARTESIAN_POINT('Ctrl Pts',(1.66846059277303,-1.,1.00265091003727));
#26827=CARTESIAN_POINT('Ctrl Pts',(1.67250335383293,-1.,1.00692206696414));
#26828=CARTESIAN_POINT('Ctrl Pts',(1.67648246776464,-1.,1.01123236493511));
#26829=CARTESIAN_POINT('Ctrl Pts',(1.68044289894798,-1.,1.01561026162773));
#26830=CARTESIAN_POINT('Ctrl Pts',(1.68440578021706,-1.,1.02006795074201));
#26831=CARTESIAN_POINT('Ctrl Pts',(1.68836910178447,-1.,1.02460180535255));
#26832=CARTESIAN_POINT('Ctrl Pts',(1.69231840863458,-1.,1.02919977579147));
#26833=CARTESIAN_POINT('Ctrl Pts',(1.69623414782771,-1.,1.03384646003588));
#26834=CARTESIAN_POINT('Ctrl Pts',(1.70010052930962,-1.,1.03852922490789));
#26835=CARTESIAN_POINT('Ctrl Pts',(1.70391338707982,-1.,1.04324363334554));
#26836=CARTESIAN_POINT('Ctrl Pts',(1.70767646263649,-1.,1.04799085404995));
#26837=CARTESIAN_POINT('Ctrl Pts',(1.71139783543989,-1.,1.05277517202855));
#26838=CARTESIAN_POINT('Ctrl Pts',(1.7150865442702,-1.,1.05760163192479));
#26839=CARTESIAN_POINT('Ctrl Pts',(1.71874858456904,-1.,1.06247324680647));
#26840=CARTESIAN_POINT('Ctrl Pts',(1.72238500928453,-1.,1.06738966975462));
#26841=CARTESIAN_POINT('Ctrl Pts',(1.72599406198488,-1.,1.07234866990252));
#26842=CARTESIAN_POINT('Ctrl Pts',(1.72957248977424,-1.,1.0773470373727));
#26843=CARTESIAN_POINT('Ctrl Pts',(1.73311705663407,-1.,1.08238162784749));
#26844=CARTESIAN_POINT('Ctrl Pts',(1.73662628326091,-1.,1.08745056285427));
#26845=CARTESIAN_POINT('Ctrl Pts',(1.74010053962247,-1.,1.09255329056493));
#26846=CARTESIAN_POINT('Ctrl Pts',(1.74354119236208,-1.,1.09768999241226));
#26847=CARTESIAN_POINT('Ctrl Pts',(1.74695004214923,-1.,1.10286118991143));
#26848=CARTESIAN_POINT('Ctrl Pts',(1.7503286607592,-1.,1.10806728183007));
#26849=CARTESIAN_POINT('Ctrl Pts',(1.7536777209463,-1.,1.11330807582551));
#26850=CARTESIAN_POINT('Ctrl Pts',(1.75699720772105,-1.,1.11858293216763));
#26851=CARTESIAN_POINT('Ctrl Pts',(1.76028671825096,-1.,1.12389096855086));
#26852=CARTESIAN_POINT('Ctrl Pts',(1.7635457196617,-1.,1.12923123555075));
#26853=CARTESIAN_POINT('Ctrl Pts',(1.76677384551862,-1.,1.1346029180462));
#26854=CARTESIAN_POINT('Ctrl Pts',(1.76997111386769,-1.,1.14000548336975));
#26855=CARTESIAN_POINT('Ctrl Pts',(1.77313777896194,-1.,1.1454385822692));
#26856=CARTESIAN_POINT('Ctrl Pts',(1.7762742255701,-1.,1.15090197841515));
#26857=CARTESIAN_POINT('Ctrl Pts',(1.77938085564275,-1.,1.15639547194698));
#26858=CARTESIAN_POINT('Ctrl Pts',(1.78245795881009,-1.,1.16191881298499));
#26859=CARTESIAN_POINT('Ctrl Pts',(1.78550566040443,-1.,1.16747166312303));
#26860=CARTESIAN_POINT('Ctrl Pts',(1.78852398877616,-1.,1.17305363177328));
#26861=CARTESIAN_POINT('Ctrl Pts',(1.79151291552689,-1.,1.17866429440809));
#26862=CARTESIAN_POINT('Ctrl Pts',(1.79447240321515,-1.,1.18430321697432));
#26863=CARTESIAN_POINT('Ctrl Pts',(1.79740245923478,-1.,1.18996997934445));
#26864=CARTESIAN_POINT('Ctrl Pts',(1.80030314369879,-1.,1.19566418930242));
#26865=CARTESIAN_POINT('Ctrl Pts',(1.80317454838603,-1.,1.20138548938974));
#26866=CARTESIAN_POINT('Ctrl Pts',(1.80601678480707,-1.,1.20713356605475));
#26867=CARTESIAN_POINT('Ctrl Pts',(1.80882996917129,-1.,1.21290815708314));
#26868=CARTESIAN_POINT('Ctrl Pts',(1.81161420806656,-1.,1.21870906103557));
#26869=CARTESIAN_POINT('Ctrl Pts',(1.81436959210434,-1.,1.2245361330495));
#26870=CARTESIAN_POINT('Ctrl Pts',(1.8165508718364,-1.,1.2292186489137));
#26871=CARTESIAN_POINT('Ctrl Pts',(1.81817389921279,-1.,1.2327422452705));
#26872=CARTESIAN_POINT('Ctrl Pts',(1.81925017193666,-1.,1.23509651170476));
#26873=CARTESIAN_POINT('Ctrl Pts',(1.81978687191668,-1.,1.23627494547115));
#26874=CARTESIAN_POINT('',(1.73811241238545,-1.,1.34869019493419));
#26875=CARTESIAN_POINT('',(1.81978687191668,-1.,1.23627494547115));
#26876=CARTESIAN_POINT('',(1.31362392696032,-1.,1.15624053661742));
#26877=CARTESIAN_POINT('Ctrl Pts',(1.73811241238545,-1.,1.34869019493419));
#26878=CARTESIAN_POINT('Ctrl Pts',(1.73682580585691,-1.,1.34854391898045));
#26879=CARTESIAN_POINT('Ctrl Pts',(1.73425417885907,-1.,1.34824783112887));
#26880=CARTESIAN_POINT('Ctrl Pts',(1.7304014965394,-1.,1.34779309152035));
#26881=CARTESIAN_POINT('Ctrl Pts',(1.72527410680674,-1.,1.34716554819527));
#26882=CARTESIAN_POINT('Ctrl Pts',(1.7188807715049,-1.,1.34634568653227));
#26883=CARTESIAN_POINT('Ctrl Pts',(1.71250340686822,-1.,1.34549029589416));
#26884=CARTESIAN_POINT('Ctrl Pts',(1.70614212266738,-1.,1.34459924533831));
#26885=CARTESIAN_POINT('Ctrl Pts',(1.69979707754427,-1.,1.34367237124483));
#26886=CARTESIAN_POINT('Ctrl Pts',(1.6934684849687,-1.,1.34270948206319));
#26887=CARTESIAN_POINT('Ctrl Pts',(1.68715660868764,-1.,1.341710374848));
#26888=CARTESIAN_POINT('Ctrl Pts',(1.68086176030362,-1.,1.34067485185203));
#26889=CARTESIAN_POINT('Ctrl Pts',(1.67458429426086,-1.,1.3396027347034));
#26890=CARTESIAN_POINT('Ctrl Pts',(1.66832460783989,-1.,1.33849388654388));
#26891=CARTESIAN_POINT('Ctrl Pts',(1.66208312541983,-1.,1.33734820885262));
#26892=CARTESIAN_POINT('Ctrl Pts',(1.65586025952593,-1.,1.33616559745172));
#26893=CARTESIAN_POINT('Ctrl Pts',(1.6496563728683,-1.,1.33494590467993));
#26894=CARTESIAN_POINT('Ctrl Pts',(1.6434717485603,-1.,1.33368890676572));
#26895=CARTESIAN_POINT('Ctrl Pts',(1.63730653475089,-1.,1.33239425103724));
#26896=CARTESIAN_POINT('Ctrl Pts',(1.63116079730923,-1.,1.33106149345645));
#26897=CARTESIAN_POINT('Ctrl Pts',(1.62503464209797,-1.,1.3296901950568));
#26898=CARTESIAN_POINT('Ctrl Pts',(1.61892832270724,-1.,1.32828000610449));
#26899=CARTESIAN_POINT('Ctrl Pts',(1.6128423401575,-1.,1.32683074483356));
#26900=CARTESIAN_POINT('Ctrl Pts',(1.60677758290954,-1.,1.32534250785782));
#26901=CARTESIAN_POINT('Ctrl Pts',(1.60073511858687,-1.,1.32381550858256));
#26902=CARTESIAN_POINT('Ctrl Pts',(1.59471591079403,-1.,1.32224985747682));
#26903=CARTESIAN_POINT('Ctrl Pts',(1.58872057258245,-1.,1.32064537110892));
#26904=CARTESIAN_POINT('Ctrl Pts',(1.58274907898834,-1.,1.31900135021432));
#26905=CARTESIAN_POINT('Ctrl Pts',(1.5768005650559,-1.,1.31731642317187));
#26906=CARTESIAN_POINT('Ctrl Pts',(1.57087397835723,-1.,1.31558903860016));
#26907=CARTESIAN_POINT('Ctrl Pts',(1.56496872402353,-1.,1.31381795281002));
#26908=CARTESIAN_POINT('Ctrl Pts',(1.55908521254821,-1.,1.31200264341696));
#26909=CARTESIAN_POINT('Ctrl Pts',(1.55322568759481,-1.,1.31014393684222));
#26910=CARTESIAN_POINT('Ctrl Pts',(1.54739413957185,-1.,1.30824393907473));
#26911=CARTESIAN_POINT('Ctrl Pts',(1.54159462645432,-1.,1.30630475189556));
#26912=CARTESIAN_POINT('Ctrl Pts',(1.53582981268977,-1.,1.30432735639489));
#26913=CARTESIAN_POINT('Ctrl Pts',(1.53009970283891,-1.,1.30231064395568));
#26914=CARTESIAN_POINT('Ctrl Pts',(1.52439957861062,-1.,1.30024984366328));
#26915=CARTESIAN_POINT('Ctrl Pts',(1.51872184912724,-1.,1.29813791800747));
#26916=CARTESIAN_POINT('Ctrl Pts',(1.51305994241402,-1.,1.29596850710509));
#26917=CARTESIAN_POINT('Ctrl Pts',(1.50741159078365,-1.,1.29373841372842));
#26918=CARTESIAN_POINT('Ctrl Pts',(1.50178230149776,-1.,1.29145022885181));
#26919=CARTESIAN_POINT('Ctrl Pts',(1.49618896881754,-1.,1.28911506584254));
#26920=CARTESIAN_POINT('Ctrl Pts',(1.4906522831278,-1.,1.2867467611644));
#26921=CARTESIAN_POINT('Ctrl Pts',(1.4851881711891,-1.,1.28435533880201));
#26922=CARTESIAN_POINT('Ctrl Pts',(1.47980070347095,-1.,1.28194158939517));
#26923=CARTESIAN_POINT('Ctrl Pts',(1.4744717526707,-1.,1.2794891824849));
#26924=CARTESIAN_POINT('Ctrl Pts',(1.46916035917133,-1.,1.2769641483109));
#26925=CARTESIAN_POINT('Ctrl Pts',(1.46382431332476,-1.,1.27433119897822));
#26926=CARTESIAN_POINT('Ctrl Pts',(1.45843906294697,-1.,1.27156805265289));
#26927=CARTESIAN_POINT('Ctrl Pts',(1.45301422764247,-1.,1.2686778680489));
#26928=CARTESIAN_POINT('Ctrl Pts',(1.44761985001662,-1.,1.26570925118868));
#26929=CARTESIAN_POINT('Ctrl Pts',(1.44236470511303,-1.,1.26273903323859));
#26930=CARTESIAN_POINT('Ctrl Pts',(1.43734919180847,-1.,1.25983531012005));
#26931=CARTESIAN_POINT('Ctrl Pts',(1.43262645609691,-1.,1.25702687965755));
#26932=CARTESIAN_POINT('Ctrl Pts',(1.42815938799387,-1.,1.25426945222639));
#26933=CARTESIAN_POINT('Ctrl Pts',(1.42378102115575,-1.,1.2514145557001));
#26934=CARTESIAN_POINT('Ctrl Pts',(1.41923722596025,-1.,1.24824430986571));
#26935=CARTESIAN_POINT('Ctrl Pts',(1.41422913175179,-1.,1.24450600513056));
#26936=CARTESIAN_POINT('Ctrl Pts',(1.40845295531283,-1.,1.23994455029534));
#26937=CARTESIAN_POINT('Ctrl Pts',(1.40164708206106,-1.,1.23434087290423));
#26938=CARTESIAN_POINT('Ctrl Pts',(1.39361389568796,-1.,1.22752961899387));
#26939=CARTESIAN_POINT('Ctrl Pts',(1.38420564527715,-1.,1.21938737280852));
#26940=CARTESIAN_POINT('Ctrl Pts',(1.37331915607905,-1.,1.20982812925645));
#26941=CARTESIAN_POINT('Ctrl Pts',(1.36088705043885,-1.,1.1987959077932));
#26942=CARTESIAN_POINT('Ctrl Pts',(1.34687054001093,-1.,1.18625865667441));
#26943=CARTESIAN_POINT('Ctrl Pts',(1.33437539347008,-1.,1.17501305789857));
#26944=CARTESIAN_POINT('Ctrl Pts',(1.32428080721772,-1.,1.16589330093588));
#26945=CARTESIAN_POINT('Ctrl Pts',(1.31722977216397,-1.,1.15950888730809));
#26946=CARTESIAN_POINT('Ctrl Pts',(1.31362392696032,-1.,1.15624053661742));
#26947=CARTESIAN_POINT('',(1.15624053661742,-1.,1.31362392696033));
#26948=CARTESIAN_POINT('Origin',(0.,-1.,0.));
#26949=CARTESIAN_POINT('',(1.34869019493419,-1.,1.73811241238545));
#26950=CARTESIAN_POINT('Ctrl Pts',(1.15624053661742,-1.,1.31362392696033));
#26951=CARTESIAN_POINT('Ctrl Pts',(1.15950888730433,-1.,1.3172297721596));
#26952=CARTESIAN_POINT('Ctrl Pts',(1.16589330092532,-1.,1.32428080720544));
#26953=CARTESIAN_POINT('Ctrl Pts',(1.17501305787994,-1.,1.33437539344842));
#26954=CARTESIAN_POINT('Ctrl Pts',(1.18625865664915,-1.,1.34687053998157));
#26955=CARTESIAN_POINT('Ctrl Pts',(1.1987959077656,-1.,1.36088705040677));
#26956=CARTESIAN_POINT('Ctrl Pts',(1.20982812923113,-1.,1.37331915604962));
#26957=CARTESIAN_POINT('Ctrl Pts',(1.21938737278853,-1.,1.38420564525391));
#26958=CARTESIAN_POINT('Ctrl Pts',(1.22752961898063,-1.,1.39361389567257));
#26959=CARTESIAN_POINT('Ctrl Pts',(1.23434087289768,-1.,1.40164708205345));
#26960=CARTESIAN_POINT('Ctrl Pts',(1.23994455029421,-1.,1.40845295531151));
#26961=CARTESIAN_POINT('Ctrl Pts',(1.24450600513278,-1.,1.41422913175437));
#26962=CARTESIAN_POINT('Ctrl Pts',(1.24824430986911,-1.,1.41923722596421));
#26963=CARTESIAN_POINT('Ctrl Pts',(1.25141455570299,-1.,1.42378102115911));
#26964=CARTESIAN_POINT('Ctrl Pts',(1.25426945222783,-1.,1.42815938799555));
#26965=CARTESIAN_POINT('Ctrl Pts',(1.25702687965744,-1.,1.43262645609679));
#26966=CARTESIAN_POINT('Ctrl Pts',(1.25983531011894,-1.,1.43734919180719));
#26967=CARTESIAN_POINT('Ctrl Pts',(1.26273903323723,-1.,1.44236470511145));
#26968=CARTESIAN_POINT('Ctrl Pts',(1.26570925118767,-1.,1.44761985001544));
#26969=CARTESIAN_POINT('Ctrl Pts',(1.26867786804854,-1.,1.45301422764205));
#26970=CARTESIAN_POINT('Ctrl Pts',(1.27156805265312,-1.,1.45843906294725));
#26971=CARTESIAN_POINT('Ctrl Pts',(1.27433119897877,-1.,1.4638243133254));
#26972=CARTESIAN_POINT('Ctrl Pts',(1.27696414831144,-1.,1.46916035917197));
#26973=CARTESIAN_POINT('Ctrl Pts',(1.27948918248524,-1.,1.4744717526711));
#26974=CARTESIAN_POINT('Ctrl Pts',(1.28194158939522,-1.,1.47980070347102));
#26975=CARTESIAN_POINT('Ctrl Pts',(1.28435533880184,-1.,1.48518817118891));
#26976=CARTESIAN_POINT('Ctrl Pts',(1.28674676116415,-1.,1.4906522831275));
#26977=CARTESIAN_POINT('Ctrl Pts',(1.28911506584232,-1.,1.49618896881729));
#26978=CARTESIAN_POINT('Ctrl Pts',(1.29145022885171,-1.,1.50178230149764));
#26979=CARTESIAN_POINT('Ctrl Pts',(1.29373841372843,-1.,1.50741159078367));
#26980=CARTESIAN_POINT('Ctrl Pts',(1.29596850710518,-1.,1.51305994241412));
#26981=CARTESIAN_POINT('Ctrl Pts',(1.29813791800757,-1.,1.51872184912735));
#26982=CARTESIAN_POINT('Ctrl Pts',(1.30024984366334,-1.,1.5243995786107));
#26983=CARTESIAN_POINT('Ctrl Pts',(1.3023106439557,-1.,1.53009970283893));
#26984=CARTESIAN_POINT('Ctrl Pts',(1.30432735639487,-1.,1.53582981268976));
#26985=CARTESIAN_POINT('Ctrl Pts',(1.30630475189553,-1.,1.54159462645428));
#26986=CARTESIAN_POINT('Ctrl Pts',(1.30824393907471,-1.,1.54739413957183));
#26987=CARTESIAN_POINT('Ctrl Pts',(1.31014393684221,-1.,1.55322568759481));
#26988=CARTESIAN_POINT('Ctrl Pts',(1.31200264341696,-1.,1.55908521254822));
#26989=CARTESIAN_POINT('Ctrl Pts',(1.31381795281002,-1.,1.56496872402352));
#26990=CARTESIAN_POINT('Ctrl Pts',(1.31558903860015,-1.,1.57087397835721));
#26991=CARTESIAN_POINT('Ctrl Pts',(1.31731642317183,-1.,1.57680056505585));
#26992=CARTESIAN_POINT('Ctrl Pts',(1.31900135021428,-1.,1.58274907898829));
#26993=CARTESIAN_POINT('Ctrl Pts',(1.32064537110891,-1.,1.58872057258244));
#26994=CARTESIAN_POINT('Ctrl Pts',(1.32224985747686,-1.,1.59471591079408));
#26995=CARTESIAN_POINT('Ctrl Pts',(1.32381550858266,-1.,1.600735118587));
#26996=CARTESIAN_POINT('Ctrl Pts',(1.32534250785794,-1.,1.6067775829097));
#26997=CARTESIAN_POINT('Ctrl Pts',(1.32683074483365,-1.,1.61284234015762));
#26998=CARTESIAN_POINT('Ctrl Pts',(1.32828000610448,-1.,1.61892832270723));
#26999=CARTESIAN_POINT('Ctrl Pts',(1.32969019505665,-1.,1.62503464209777));
#27000=CARTESIAN_POINT('Ctrl Pts',(1.33106149345618,-1.,1.63116079730887));
#27001=CARTESIAN_POINT('Ctrl Pts',(1.33239425103694,-1.,1.6373065347505));
#27002=CARTESIAN_POINT('Ctrl Pts',(1.33368890676554,-1.,1.64347174856007));
#27003=CARTESIAN_POINT('Ctrl Pts',(1.33494590468003,-1.,1.64965637286843));
#27004=CARTESIAN_POINT('Ctrl Pts',(1.33616559745217,-1.,1.65586025952651));
#27005=CARTESIAN_POINT('Ctrl Pts',(1.33734820885331,-1.,1.66208312542073));
#27006=CARTESIAN_POINT('Ctrl Pts',(1.33849388654458,-1.,1.66832460784078));
#27007=CARTESIAN_POINT('Ctrl Pts',(1.33960273470372,-1.,1.67458429426126));
#27008=CARTESIAN_POINT('Ctrl Pts',(1.3406748518516,-1.,1.68086176030308));
#27009=CARTESIAN_POINT('Ctrl Pts',(1.34171037484673,-1.,1.68715660868602));
#27010=CARTESIAN_POINT('Ctrl Pts',(1.34270948206139,-1.,1.6934684849664));
#27011=CARTESIAN_POINT('Ctrl Pts',(1.34367237124322,-1.,1.69979707754221));
#27012=CARTESIAN_POINT('Ctrl Pts',(1.34459924533783,-1.,1.70614212266676));
#27013=CARTESIAN_POINT('Ctrl Pts',(1.34549029589563,-1.,1.71250340687011));
#27014=CARTESIAN_POINT('Ctrl Pts',(1.34634568653586,-1.,1.7188807715095));
#27015=CARTESIAN_POINT('Ctrl Pts',(1.34716554820013,-1.,1.72527410681298));
#27016=CARTESIAN_POINT('Ctrl Pts',(1.3477930915247,-1.,1.73040149654497));
#27017=CARTESIAN_POINT('Ctrl Pts',(1.34824783113158,-1.,1.73425417886255));
#27018=CARTESIAN_POINT('Ctrl Pts',(1.34854391898145,-1.,1.73682580585819));
#27019=CARTESIAN_POINT('Ctrl Pts',(1.34869019493419,-1.,1.73811241238545));
#27020=CARTESIAN_POINT('',(1.23627494547115,-1.,1.81978687191668));
#27021=CARTESIAN_POINT('',(1.34869019493419,-1.,1.73811241238545));
#27022=CARTESIAN_POINT('',(0.892032620296855,-1.,1.5055822144029));
#27023=CARTESIAN_POINT('Ctrl Pts',(1.23627494547115,-1.,1.81978687191668));
#27024=CARTESIAN_POINT('Ctrl Pts',(1.23509651170384,-1.,1.81925017193531));
#27025=CARTESIAN_POINT('Ctrl Pts',(1.23274224526804,-1.,1.81817389920914));
#27026=CARTESIAN_POINT('Ctrl Pts',(1.22921864890975,-1.,1.81655087183054));
#27027=CARTESIAN_POINT('Ctrl Pts',(1.22453613304507,-1.,1.81436959209778));
#27028=CARTESIAN_POINT('Ctrl Pts',(1.2187090610323,-1.,1.81161420806172));
#27029=CARTESIAN_POINT('Ctrl Pts',(1.2129081570818,-1.,1.80882996916931));
#27030=CARTESIAN_POINT('Ctrl Pts',(1.20713356605519,-1.,1.80601678480772));
#27031=CARTESIAN_POINT('Ctrl Pts',(1.2013854893912,-1.,1.8031745483882));
#27032=CARTESIAN_POINT('Ctrl Pts',(1.19566418930405,-1.,1.80030314370121));
#27033=CARTESIAN_POINT('Ctrl Pts',(1.1899699793456,-1.,1.79740245923649));
#27034=CARTESIAN_POINT('Ctrl Pts',(1.18430321697471,-1.,1.79447240321572));
#27035=CARTESIAN_POINT('Ctrl Pts',(1.17866429440781,-1.,1.79151291552646));
#27036=CARTESIAN_POINT('Ctrl Pts',(1.17305363177265,-1.,1.78852398877523));
#27037=CARTESIAN_POINT('Ctrl Pts',(1.16747166312239,-1.,1.78550566040349));
#27038=CARTESIAN_POINT('Ctrl Pts',(1.16191881298458,-1.,1.78245795880949));
#27039=CARTESIAN_POINT('Ctrl Pts',(1.15639547194689,-1.,1.77938085564261));
#27040=CARTESIAN_POINT('Ctrl Pts',(1.15090197841531,-1.,1.77627422557034));
#27041=CARTESIAN_POINT('Ctrl Pts',(1.14543858226948,-1.,1.77313777896234));
#27042=CARTESIAN_POINT('Ctrl Pts',(1.14000548337,-1.,1.76997111386806));
#27043=CARTESIAN_POINT('Ctrl Pts',(1.13460291804634,-1.,1.76677384551883));
#27044=CARTESIAN_POINT('Ctrl Pts',(1.12923123555076,-1.,1.76354571966171));
#27045=CARTESIAN_POINT('Ctrl Pts',(1.12389096855078,-1.,1.76028671825084));
#27046=CARTESIAN_POINT('Ctrl Pts',(1.11858293216752,-1.,1.75699720772089));
#27047=CARTESIAN_POINT('Ctrl Pts',(1.11330807582542,-1.,1.75367772094617));
#27048=CARTESIAN_POINT('Ctrl Pts',(1.10806728183003,-1.,1.75032866075914));
#27049=CARTESIAN_POINT('Ctrl Pts',(1.10286118991144,-1.,1.74695004214924));
#27050=CARTESIAN_POINT('Ctrl Pts',(1.09768999241229,-1.,1.74354119236212));
#27051=CARTESIAN_POINT('Ctrl Pts',(1.09255329056496,-1.,1.74010053962252));
#27052=CARTESIAN_POINT('Ctrl Pts',(1.08745056285429,-1.,1.73662628326093));
#27053=CARTESIAN_POINT('Ctrl Pts',(1.08238162784749,-1.,1.73311705663407));
#27054=CARTESIAN_POINT('Ctrl Pts',(1.0773470373727,-1.,1.72957248977424));
#27055=CARTESIAN_POINT('Ctrl Pts',(1.07234866990252,-1.,1.72599406198489));
#27056=CARTESIAN_POINT('Ctrl Pts',(1.06738966975463,-1.,1.72238500928456));
#27057=CARTESIAN_POINT('Ctrl Pts',(1.06247324680649,-1.,1.71874858456908));
#27058=CARTESIAN_POINT('Ctrl Pts',(1.05760163192481,-1.,1.71508654427022));
#27059=CARTESIAN_POINT('Ctrl Pts',(1.05277517202853,-1.,1.71139783543986));
#27060=CARTESIAN_POINT('Ctrl Pts',(1.0479908540499,-1.,1.70767646263641));
#27061=CARTESIAN_POINT('Ctrl Pts',(1.04324363334546,-1.,1.70391338707969));
#27062=CARTESIAN_POINT('Ctrl Pts',(1.03852922490782,-1.,1.70010052930951));
#27063=CARTESIAN_POINT('Ctrl Pts',(1.03384646003587,-1.,1.69623414782769));
#27064=CARTESIAN_POINT('Ctrl Pts',(1.02919977579155,-1.,1.69231840863471));
#27065=CARTESIAN_POINT('Ctrl Pts',(1.02460180535272,-1.,1.68836910178475));
#27066=CARTESIAN_POINT('Ctrl Pts',(1.02006795074222,-1.,1.68440578021739));
#27067=CARTESIAN_POINT('Ctrl Pts',(1.01561026162786,-1.,1.6804428989482));
#27068=CARTESIAN_POINT('Ctrl Pts',(1.01123236493507,-1.,1.67648246776457));
#27069=CARTESIAN_POINT('Ctrl Pts',(1.00692206696387,-1.,1.67250335383248));
#27070=CARTESIAN_POINT('Ctrl Pts',(1.00265091003682,-1.,1.66846059277231));
#27071=CARTESIAN_POINT('Ctrl Pts',(0.998389654952317,-1.,1.66430758030304));
#27072=CARTESIAN_POINT('Ctrl Pts',(0.994121836661115,-1.,1.66001553809916));
#27073=CARTESIAN_POINT('Ctrl Pts',(0.98985562785445,-1.,1.65559044289746));
#27074=CARTESIAN_POINT('Ctrl Pts',(0.985642622921626,-1.,1.6511001661277));
#27075=CARTESIAN_POINT('Ctrl Pts',(0.981562530940574,-1.,1.64665139190834));
#27076=CARTESIAN_POINT('Ctrl Pts',(0.977689794120296,-1.,1.64233990826831));
#27077=CARTESIAN_POINT('Ctrl Pts',(0.974066058287501,-1.,1.63820952658157));
#27078=CARTESIAN_POINT('Ctrl Pts',(0.970669715996356,-1.,1.63420665729609));
#27079=CARTESIAN_POINT('Ctrl Pts',(0.967387853228041,-1.,1.63013849959083));
#27080=CARTESIAN_POINT('Ctrl Pts',(0.964046107037821,-1.,1.6257193066974));
#27081=CARTESIAN_POINT('Ctrl Pts',(0.960438326099958,-1.,1.62061638139929));
#27082=CARTESIAN_POINT('Ctrl Pts',(0.956354422921572,-1.,1.61449324337233));
#27083=CARTESIAN_POINT('Ctrl Pts',(0.951613284361247,-1.,1.60706069897794));
#27084=CARTESIAN_POINT('Ctrl Pts',(0.946078063325795,-1.,1.59810042045408));
#27085=CARTESIAN_POINT('Ctrl Pts',(0.939646377909319,-1.,1.58744937489796));
#27086=CARTESIAN_POINT('Ctrl Pts',(0.932246680128848,-1.,1.57499388385561));
#27087=CARTESIAN_POINT('Ctrl Pts',(0.923832188966322,-1.,1.56065988582509));
#27088=CARTESIAN_POINT('Ctrl Pts',(0.914375919046579,-1.,1.54440491152808));
#27089=CARTESIAN_POINT('Ctrl Pts',(0.905967409640498,-1.,1.52984849890434));
#27090=CARTESIAN_POINT('Ctrl Pts',(0.89918504749193,-1.,1.51805569591479));
#27091=CARTESIAN_POINT('Ctrl Pts',(0.894452006967538,-1.,1.50980486807181));
#27092=CARTESIAN_POINT('Ctrl Pts',(0.892032620296855,-1.,1.5055822144029));
#27093=CARTESIAN_POINT('',(0.693717979106305,-1.,1.60662857109684));
#27094=CARTESIAN_POINT('Origin',(0.,-1.,0.));
#27095=CARTESIAN_POINT('',(0.7455743247944,-1.,2.0698113262342));
#27096=CARTESIAN_POINT('Ctrl Pts',(0.693717979106305,-1.,1.60662857109684));
#27097=CARTESIAN_POINT('Ctrl Pts',(0.69571209787897,-1.,1.61106790957619));
#27098=CARTESIAN_POINT('Ctrl Pts',(0.699605146398836,-1.,1.61974673471117));
#27099=CARTESIAN_POINT('Ctrl Pts',(0.705159151977294,-1.,1.6321654166204));
#27100=CARTESIAN_POINT('Ctrl Pts',(0.711993139340447,-1.,1.64752408828442));
#27101=CARTESIAN_POINT('Ctrl Pts',(0.719585433787949,-1.,1.66472880551777));
#27102=CARTESIAN_POINT('Ctrl Pts',(0.726235967982445,-1.,1.67996158451922));
#27103=CARTESIAN_POINT('Ctrl Pts',(0.731963238685357,-1.,1.69326921972915));
#27104=CARTESIAN_POINT('Ctrl Pts',(0.736799665716932,-1.,1.70473309004249));
#27105=CARTESIAN_POINT('Ctrl Pts',(0.74079516202821,-1.,1.71447789751001));
#27106=CARTESIAN_POINT('Ctrl Pts',(0.744021445433093,-1.,1.72268229916769));
#27107=CARTESIAN_POINT('Ctrl Pts',(0.746574710097752,-1.,1.72958533647714));
#27108=CARTESIAN_POINT('Ctrl Pts',(0.74858246295687,-1.,1.7355035168033));
#27109=CARTESIAN_POINT('Ctrl Pts',(0.750193435981249,-1.,1.74080458267114));
#27110=CARTESIAN_POINT('Ctrl Pts',(0.751555614164482,-1.,1.74585086852502));
#27111=CARTESIAN_POINT('Ctrl Pts',(0.752797683531314,-1.,1.75095139468794));
#27112=CARTESIAN_POINT('Ctrl Pts',(0.754009254027828,-1.,1.75631083600019));
#27113=CARTESIAN_POINT('Ctrl Pts',(0.755220979974461,-1.,1.76197817240128));
#27114=CARTESIAN_POINT('Ctrl Pts',(0.75642189602781,-1.,1.76789396002998));
#27115=CARTESIAN_POINT('Ctrl Pts',(0.757578264077028,-1.,1.77394167108292));
#27116=CARTESIAN_POINT('Ctrl Pts',(0.758650626677518,-1.,1.77999411220945));
#27117=CARTESIAN_POINT('Ctrl Pts',(0.759614401110189,-1.,1.78596964884604));
#27118=CARTESIAN_POINT('Ctrl Pts',(0.760469555880749,-1.,1.7918581561088));
#27119=CARTESIAN_POINT('Ctrl Pts',(0.761229695230558,-1.,1.79768986997783));
#27120=CARTESIAN_POINT('Ctrl Pts',(0.761915336443547,-1.,1.80351583877342));
#27121=CARTESIAN_POINT('Ctrl Pts',(0.762546129463938,-1.,1.80938551463965));
#27122=CARTESIAN_POINT('Ctrl Pts',(0.763132003836634,-1.,1.8153211840553));
#27123=CARTESIAN_POINT('Ctrl Pts',(0.763673465462726,-1.,1.82131873145266));
#27124=CARTESIAN_POINT('Ctrl Pts',(0.764165902605995,-1.,1.82735991200065));
#27125=CARTESIAN_POINT('Ctrl Pts',(0.764602549687853,-1.,1.83342077227142));
#27126=CARTESIAN_POINT('Ctrl Pts',(0.764978057881737,-1.,1.83948181064835));
#27127=CARTESIAN_POINT('Ctrl Pts',(0.765291664862029,-1.,1.84553698875924));
#27128=CARTESIAN_POINT('Ctrl Pts',(0.765545710619062,-1.,1.85158945130063));
#27129=CARTESIAN_POINT('Ctrl Pts',(0.765744212909318,-1.,1.85764741390394));
#27130=CARTESIAN_POINT('Ctrl Pts',(0.765891519092547,-1.,1.86372027063312));
#27131=CARTESIAN_POINT('Ctrl Pts',(0.765990708546091,-1.,1.86981398314341));
#27132=CARTESIAN_POINT('Ctrl Pts',(0.766042837036744,-1.,1.87592888967883));
#27133=CARTESIAN_POINT('Ctrl Pts',(0.766047794851864,-1.,1.88206215302561));
#27134=CARTESIAN_POINT('Ctrl Pts',(0.766004837062091,-1.,1.88820926433409));
#27135=CARTESIAN_POINT('Ctrl Pts',(0.765913193856978,-1.,1.89436577771388));
#27136=CARTESIAN_POINT('Ctrl Pts',(0.765772772593386,-1.,1.90052930393596));
#27137=CARTESIAN_POINT('Ctrl Pts',(0.765584196937919,-1.,1.90669961402356));
#27138=CARTESIAN_POINT('Ctrl Pts',(0.765348465884722,-1.,1.91287765805169));
#27139=CARTESIAN_POINT('Ctrl Pts',(0.765066729667088,-1.,1.91906491634196));
#27140=CARTESIAN_POINT('Ctrl Pts',(0.764740025488211,-1.,1.92526263537048));
#27141=CARTESIAN_POINT('Ctrl Pts',(0.76436901067394,-1.,1.93147105496382));
#27142=CARTESIAN_POINT('Ctrl Pts',(0.763954049121458,-1.,1.93768964875886));
#27143=CARTESIAN_POINT('Ctrl Pts',(0.763495333538629,-1.,1.9439174661764));
#27144=CARTESIAN_POINT('Ctrl Pts',(0.762992990878769,-1.,1.95015342590024));
#27145=CARTESIAN_POINT('Ctrl Pts',(0.762447203806178,-1.,1.95639665309869));
#27146=CARTESIAN_POINT('Ctrl Pts',(0.761858300014423,-1.,1.96264672744186));
#27147=CARTESIAN_POINT('Ctrl Pts',(0.76122669048382,-1.,1.96890351582499));
#27148=CARTESIAN_POINT('Ctrl Pts',(0.760552825409757,-1.,1.97516705321494));
#27149=CARTESIAN_POINT('Ctrl Pts',(0.75983714745219,-1.,1.98143741418172));
#27150=CARTESIAN_POINT('Ctrl Pts',(0.759080037802488,-1.,1.98771456680874));
#27151=CARTESIAN_POINT('Ctrl Pts',(0.758281796766761,-1.,1.99399831098817));
#27152=CARTESIAN_POINT('Ctrl Pts',(0.757442676862724,-1.,2.00028834739178));
#27153=CARTESIAN_POINT('Ctrl Pts',(0.75656290464667,-1.,2.0065843158773));
#27154=CARTESIAN_POINT('Ctrl Pts',(0.755642704957865,-1.,2.01288584328084));
#27155=CARTESIAN_POINT('Ctrl Pts',(0.754682330722816,-1.,2.01919259405809));
#27156=CARTESIAN_POINT('Ctrl Pts',(0.753682061112768,-1.,2.02550428623313));
#27157=CARTESIAN_POINT('Ctrl Pts',(0.75264218048721,-1.,2.03182068456221));
#27158=CARTESIAN_POINT('Ctrl Pts',(0.751562963361115,-1.,2.03814160092099));
#27159=CARTESIAN_POINT('Ctrl Pts',(0.750444657875575,-1.,2.04446689147979));
#27160=CARTESIAN_POINT('Ctrl Pts',(0.749287468665046,-1.,2.05079645592154));
#27161=CARTESIAN_POINT('Ctrl Pts',(0.748091554183802,-1.,2.05713023031007));
#27162=CARTESIAN_POINT('Ctrl Pts',(0.747103932787919,-1.,2.06220058927826));
#27163=CARTESIAN_POINT('Ctrl Pts',(0.7463458715442,-1.,2.06600523016815));
#27164=CARTESIAN_POINT('Ctrl Pts',(0.745832791378367,-1.,2.06854248895728));
#27165=CARTESIAN_POINT('Ctrl Pts',(0.7455743247944,-1.,2.0698113262342));
#27166=CARTESIAN_POINT('',(0.61342227326009,-1.,2.11275013067528));
#27167=CARTESIAN_POINT('',(0.7455743247944,-1.,2.0698113262342));
#27168=CARTESIAN_POINT('',(0.383122945602004,-1.,1.7075470150345));
#27169=CARTESIAN_POINT('Ctrl Pts',(0.61342227326009,-1.,2.11275013067528));
#27170=CARTESIAN_POINT('Ctrl Pts',(0.6124673655618,-1.,2.11187554259986));
#27171=CARTESIAN_POINT('Ctrl Pts',(0.610560911689898,-1.,2.11012443807238));
#27172=CARTESIAN_POINT('Ctrl Pts',(0.607711315454876,-1.,2.1074919961518));
#27173=CARTESIAN_POINT('Ctrl Pts',(0.60393203073603,-1.,2.10397049886949));
#27174=CARTESIAN_POINT('Ctrl Pts',(0.599241616420533,-1.,2.0995493086477));
#27175=CARTESIAN_POINT('Ctrl Pts',(0.594585006052162,-1.,2.0951087622027));
#27176=CARTESIAN_POINT('Ctrl Pts',(0.589962365403406,-1.,2.09064881812129));
#27177=CARTESIAN_POINT('Ctrl Pts',(0.585373918991617,-1.,2.08616943727951));
#27178=CARTESIAN_POINT('Ctrl Pts',(0.580819952108063,-1.,2.08167059018418));
#27179=CARTESIAN_POINT('Ctrl Pts',(0.576300797416844,-1.,2.07715226767559));
#27180=CARTESIAN_POINT('Ctrl Pts',(0.571816823242602,-1.,2.07261449292824));
#27181=CARTESIAN_POINT('Ctrl Pts',(0.567368421181087,-1.,2.06805732997334));
#27182=CARTESIAN_POINT('Ctrl Pts',(0.562955993082261,-1.,2.06348090160589));
#27183=CARTESIAN_POINT('Ctrl Pts',(0.558579940185151,-1.,2.05888537756462));
#27184=CARTESIAN_POINT('Ctrl Pts',(0.554240657463906,-1.,2.05427091604413));
#27185=CARTESIAN_POINT('Ctrl Pts',(0.549938525150295,-1.,2.04963761077958));
#27186=CARTESIAN_POINT('Ctrl Pts',(0.54567390381743,-1.,2.04498544714588));
#27187=CARTESIAN_POINT('Ctrl Pts',(0.541447120615659,-1.,2.04031422690527));
#27188=CARTESIAN_POINT('Ctrl Pts',(0.537258489833262,-1.,2.03562362954037));
#27189=CARTESIAN_POINT('Ctrl Pts',(0.533108355132976,-1.,2.03091336214426));
#27190=CARTESIAN_POINT('Ctrl Pts',(0.528997127241914,-1.,2.0261832908329));
#27191=CARTESIAN_POINT('Ctrl Pts',(0.524925318333476,-1.,2.02143356304698));
#27192=CARTESIAN_POINT('Ctrl Pts',(0.52089359039937,-1.,2.01666477917286));
#27193=CARTESIAN_POINT('Ctrl Pts',(0.516902681728687,-1.,2.01187773939242));
#27194=CARTESIAN_POINT('Ctrl Pts',(0.512953306961792,-1.,2.00707309946949));
#27195=CARTESIAN_POINT('Ctrl Pts',(0.509046069886157,-1.,2.00225107134734));
#27196=CARTESIAN_POINT('Ctrl Pts',(0.505181361323026,-1.,1.99741107463572));
#27197=CARTESIAN_POINT('Ctrl Pts',(0.501359287727146,-1.,1.99255149126155));
#27198=CARTESIAN_POINT('Ctrl Pts',(0.497579909545574,-1.,1.98767044752932));
#27199=CARTESIAN_POINT('Ctrl Pts',(0.493843476541494,-1.,1.98276658761821));
#27200=CARTESIAN_POINT('Ctrl Pts',(0.490150627860952,-1.,1.97783973019229));
#27201=CARTESIAN_POINT('Ctrl Pts',(0.486502692907658,-1.,1.97289186263272));
#27202=CARTESIAN_POINT('Ctrl Pts',(0.48290166212069,-1.,1.96792703422362));
#27203=CARTESIAN_POINT('Ctrl Pts',(0.479349583074855,-1.,1.96294933055943));
#27204=CARTESIAN_POINT('Ctrl Pts',(0.475848034683176,-1.,1.95796111148177));
#27205=CARTESIAN_POINT('Ctrl Pts',(0.472397672264072,-1.,1.95296148278133));
#27206=CARTESIAN_POINT('Ctrl Pts',(0.468997482913135,-1.,1.94794381136514));
#27207=CARTESIAN_POINT('Ctrl Pts',(0.46564546202603,-1.,1.9428979419619));
#27208=CARTESIAN_POINT('Ctrl Pts',(0.462340031009056,-1.,1.93781486640821));
#27209=CARTESIAN_POINT('Ctrl Pts',(0.459081234547926,-1.,1.93269066517934));
#27210=CARTESIAN_POINT('Ctrl Pts',(0.45587200517437,-1.,1.92753067150476));
#27211=CARTESIAN_POINT('Ctrl Pts',(0.452719478359432,-1.,1.92235380648502));
#27212=CARTESIAN_POINT('Ctrl Pts',(0.449632260106662,-1.,1.91718342555755));
#27213=CARTESIAN_POINT('Ctrl Pts',(0.446617343485711,-1.,1.9120369998112));
#27214=CARTESIAN_POINT('Ctrl Pts',(0.44367755684915,-1.,1.90691756144898));
#27215=CARTESIAN_POINT('Ctrl Pts',(0.440807833704038,-1.,1.90180124389086));
#27216=CARTESIAN_POINT('Ctrl Pts',(0.437995003948244,-1.,1.89663648956466));
#27217=CARTESIAN_POINT('Ctrl Pts',(0.435225660963383,-1.,1.89136993975504));
#27218=CARTESIAN_POINT('Ctrl Pts',(0.432493038548748,-1.,1.88596913666793));
#27219=CARTESIAN_POINT('Ctrl Pts',(0.429803062482344,-1.,1.88044229001832));
#27220=CARTESIAN_POINT('Ctrl Pts',(0.427183828519102,-1.,1.87486989291484));
#27221=CARTESIAN_POINT('Ctrl Pts',(0.424678177291358,-1.,1.86937803944323));
#27222=CARTESIAN_POINT('Ctrl Pts',(0.422327307418275,-1.,1.86408083334028));
#27223=CARTESIAN_POINT('Ctrl Pts',(0.420157287975619,-1.,1.85903281096686));
#27224=CARTESIAN_POINT('Ctrl Pts',(0.418164129143534,-1.,1.85417632856234));
#27225=CARTESIAN_POINT('Ctrl Pts',(0.416300022038864,-1.,1.84929312929882));
#27226=CARTESIAN_POINT('Ctrl Pts',(0.41448743825434,-1.,1.8440575707371));
#27227=CARTESIAN_POINT('Ctrl Pts',(0.412633125322161,-1.,1.83808953475839));
#27228=CARTESIAN_POINT('Ctrl Pts',(0.410641256301674,-1.,1.83100408895216));
#27229=CARTESIAN_POINT('Ctrl Pts',(0.408428948108533,-1.,1.8224702267854));
#27230=CARTESIAN_POINT('Ctrl Pts',(0.405933518411838,-1.,1.81223801813988));
#27231=CARTESIAN_POINT('Ctrl Pts',(0.403107976170441,-1.,1.80012077176221));
#27232=CARTESIAN_POINT('Ctrl Pts',(0.39991940378308,-1.,1.78598826347533));
#27233=CARTESIAN_POINT('Ctrl Pts',(0.39634619612042,-1.,1.7697556004756));
#27234=CARTESIAN_POINT('Ctrl Pts',(0.392375812294307,-1.,1.75137405313962));
#27235=CARTESIAN_POINT('Ctrl Pts',(0.388877023509191,-1.,1.7349317097561));
#27236=CARTESIAN_POINT('Ctrl Pts',(0.38607079032701,-1.,1.72162022246158));
#27237=CARTESIAN_POINT('Ctrl Pts',(0.384119047315541,-1.,1.71231062891958));
#27238=CARTESIAN_POINT('Ctrl Pts',(0.383122945602004,-1.,1.7075470150345));
#27239=CARTESIAN_POINT('',(0.163289472382896,-1.,1.74236521665491));
#27240=CARTESIAN_POINT('Origin',(0.,-1.,0.));
#27241=CARTESIAN_POINT('',(0.0694764450219578,-1.,2.19890268624765));
#27242=CARTESIAN_POINT('Ctrl Pts',(0.163289472382896,-1.,1.74236521665491));
#27243=CARTESIAN_POINT('Ctrl Pts',(0.163814161002002,-1.,1.7472034950333));
#27244=CARTESIAN_POINT('Ctrl Pts',(0.164834765707158,-1.,1.75666056638427));
#27245=CARTESIAN_POINT('Ctrl Pts',(0.1662793551464,-1.,1.77018771684844));
#27246=CARTESIAN_POINT('Ctrl Pts',(0.168032772805197,-1.,1.7869064998507));
#27247=CARTESIAN_POINT('Ctrl Pts',(0.169936923904608,-1.,1.80561530629706));
#27248=CARTESIAN_POINT('Ctrl Pts',(0.171554770204119,-1.,1.82215766811545));
#27249=CARTESIAN_POINT('Ctrl Pts',(0.1728894428919,-1.,1.83658380527692));
#27250=CARTESIAN_POINT('Ctrl Pts',(0.173946627587731,-1.,1.8489811319852));
#27251=CARTESIAN_POINT('Ctrl Pts',(0.17473525927603,-1.,1.85948367088837));
#27252=CARTESIAN_POINT('Ctrl Pts',(0.175268337590757,-1.,1.86828349694799));
#27253=CARTESIAN_POINT('Ctrl Pts',(0.175563480746485,-1.,1.87563767773588));
#27254=CARTESIAN_POINT('Ctrl Pts',(0.175644148889698,-1.,1.88188663145367));
#27255=CARTESIAN_POINT('Ctrl Pts',(0.175538155840648,-1.,1.88742606273259));
#27256=CARTESIAN_POINT('Ctrl Pts',(0.175274276190844,-1.,1.892646301985));
#27257=CARTESIAN_POINT('Ctrl Pts',(0.174879405091263,-1.,1.89788101117132));
#27258=CARTESIAN_POINT('Ctrl Pts',(0.174375518661085,-1.,1.90335253862834));
#27259=CARTESIAN_POINT('Ctrl Pts',(0.173776635257816,-1.,1.90911693975267));
#27260=CARTESIAN_POINT('Ctrl Pts',(0.173090695383496,-1.,1.91511429159527));
#27261=CARTESIAN_POINT('Ctrl Pts',(0.172321621259513,-1.,1.9212233439798));
#27262=CARTESIAN_POINT('Ctrl Pts',(0.171471191532988,-1.,1.92731093582036));
#27263=CARTESIAN_POINT('Ctrl Pts',(0.170541253116201,-1.,1.93329183155539));
#27264=CARTESIAN_POINT('Ctrl Pts',(0.16953490481749,-1.,1.93915639211581));
#27265=CARTESIAN_POINT('Ctrl Pts',(0.168455741607556,-1.,1.94493757756931));
#27266=CARTESIAN_POINT('Ctrl Pts',(0.167307501784475,-1.,1.95069027794294));
#27267=CARTESIAN_POINT('Ctrl Pts',(0.166093592002812,-1.,1.9564675971873));
#27268=CARTESIAN_POINT('Ctrl Pts',(0.164816568920269,-1.,1.96229379940136));
#27269=CARTESIAN_POINT('Ctrl Pts',(0.163478185457734,-1.,1.96816512677967));
#27270=CARTESIAN_POINT('Ctrl Pts',(0.162079693556288,-1.,1.97406280235188));
#27271=CARTESIAN_POINT('Ctrl Pts',(0.160622060784611,-1.,1.97996195437559));
#27272=CARTESIAN_POINT('Ctrl Pts',(0.159106226437299,-1.,1.98584238283292));
#27273=CARTESIAN_POINT('Ctrl Pts',(0.157533331459227,-1.,1.99169810931908));
#27274=CARTESIAN_POINT('Ctrl Pts',(0.155904629548783,-1.,1.99753284771497));
#27275=CARTESIAN_POINT('Ctrl Pts',(0.154221403049722,-1.,2.00335565310543));
#27276=CARTESIAN_POINT('Ctrl Pts',(0.152484883621449,-1.,2.00917680318424));
#27277=CARTESIAN_POINT('Ctrl Pts',(0.150696157673078,-1.,2.01500291940238));
#27278=CARTESIAN_POINT('Ctrl Pts',(0.148856124775337,-1.,2.02083464969894));
#27279=CARTESIAN_POINT('Ctrl Pts',(0.146965557332583,-1.,2.02666926182017));
#27280=CARTESIAN_POINT('Ctrl Pts',(0.145025140186057,-1.,2.03250223739942));
#27281=CARTESIAN_POINT('Ctrl Pts',(0.143035515058208,-1.,2.03832911025912));
#27282=CARTESIAN_POINT('Ctrl Pts',(0.140997332152546,-1.,2.04414757947916));
#27283=CARTESIAN_POINT('Ctrl Pts',(0.138911255368966,-1.,2.04995762001328));
#27284=CARTESIAN_POINT('Ctrl Pts',(0.136777941218043,-1.,2.05576044414264));
#27285=CARTESIAN_POINT('Ctrl Pts',(0.134598026192106,-1.,2.06155781517842));
#27286=CARTESIAN_POINT('Ctrl Pts',(0.13237211154771,-1.,2.06735123910326));
#27287=CARTESIAN_POINT('Ctrl Pts',(0.130100748328403,-1.,2.07314114713063));
#27288=CARTESIAN_POINT('Ctrl Pts',(0.12778444527612,-1.,2.07892715110987));
#27289=CARTESIAN_POINT('Ctrl Pts',(0.125423679412061,-1.,2.08470840653643));
#27290=CARTESIAN_POINT('Ctrl Pts',(0.123018905621083,-1.,2.09048392424825));
#27291=CARTESIAN_POINT('Ctrl Pts',(0.120570567965122,-1.,2.0962529286773));
#27292=CARTESIAN_POINT('Ctrl Pts',(0.118079107988355,-1.,2.102015121329));
#27293=CARTESIAN_POINT('Ctrl Pts',(0.115544957687926,-1.,2.10777050261309));
#27294=CARTESIAN_POINT('Ctrl Pts',(0.112968534419737,-1.,2.11351924490306));
#27295=CARTESIAN_POINT('Ctrl Pts',(0.110350236135025,-1.,2.11926155590865));
#27296=CARTESIAN_POINT('Ctrl Pts',(0.10769043523109,-1.,2.12499752307));
#27297=CARTESIAN_POINT('Ctrl Pts',(0.104989479152739,-1.,2.13072704887293));
#27298=CARTESIAN_POINT('Ctrl Pts',(0.1022477005561,-1.,2.13644992667165));
#27299=CARTESIAN_POINT('Ctrl Pts',(0.0994654261990913,-1.,2.14216588396025));
#27300=CARTESIAN_POINT('Ctrl Pts',(0.0966429852305456,-1.,2.14787463531795));
#27301=CARTESIAN_POINT('Ctrl Pts',(0.0937807218867641,-1.,2.1535759397817));
#27302=CARTESIAN_POINT('Ctrl Pts',(0.0908789888107263,-1.,2.15926961544516));
#27303=CARTESIAN_POINT('Ctrl Pts',(0.087938129138692,-1.,2.16495552645014));
#27304=CARTESIAN_POINT('Ctrl Pts',(0.084958462083537,-1.,2.17063357870952));
#27305=CARTESIAN_POINT('Ctrl Pts',(0.0819402680872763,-1.,2.176303712113));
#27306=CARTESIAN_POINT('Ctrl Pts',(0.078883772768524,-1.,2.18196589448887));
#27307=CARTESIAN_POINT('Ctrl Pts',(0.0757891465836145,-1.,2.1876201139953));
#27308=CARTESIAN_POINT('Ctrl Pts',(0.0732830357306722,-1.,2.19213712013662));
#27309=CARTESIAN_POINT('Ctrl Pts',(0.0713863779526151,-1.,2.19552129484002));
#27310=CARTESIAN_POINT('Ctrl Pts',(0.0701143536325487,-1.,2.19777582085423));
#27311=CARTESIAN_POINT('Ctrl Pts',(0.0694764450219578,-1.,2.19890268624765));
#27312=CARTESIAN_POINT('',(-0.0694764450219586,-1.,2.19890268624765));
#27313=CARTESIAN_POINT('',(0.0694764450219578,-1.,2.19890268624765));
#27314=CARTESIAN_POINT('',(-0.163289472382896,-1.,1.74236521665491));
#27315=CARTESIAN_POINT('Ctrl Pts',(-0.0694764450219586,-1.,2.19890268624765));
#27316=CARTESIAN_POINT('Ctrl Pts',(-0.0701143536324929,-1.,2.19777582085261));
#27317=CARTESIAN_POINT('Ctrl Pts',(-0.071386377952463,-1.,2.19552129483562));
#27318=CARTESIAN_POINT('Ctrl Pts',(-0.0732830357304279,-1.,2.19213712012956));
#27319=CARTESIAN_POINT('Ctrl Pts',(-0.0757891465833414,-1.,2.1876201139874));
#27320=CARTESIAN_POINT('Ctrl Pts',(-0.078883772768323,-1.,2.18196589448304));
#27321=CARTESIAN_POINT('Ctrl Pts',(-0.0819402680871942,-1.,2.1763037121106));
#27322=CARTESIAN_POINT('Ctrl Pts',(-0.0849584620835646,-1.,2.17063357871031));
#27323=CARTESIAN_POINT('Ctrl Pts',(-0.0879381291387825,-1.,2.16495552645275));
#27324=CARTESIAN_POINT('Ctrl Pts',(-0.0908789888108269,-1.,2.15926961544808));
#27325=CARTESIAN_POINT('Ctrl Pts',(-0.0937807218868348,-1.,2.15357593978377));
#27326=CARTESIAN_POINT('Ctrl Pts',(-0.0966429852305691,-1.,2.14787463531864));
#27327=CARTESIAN_POINT('Ctrl Pts',(-0.0994654261990745,-1.,2.14216588395974));
#27328=CARTESIAN_POINT('Ctrl Pts',(-0.102247700556064,-1.,2.13644992667052));
#27329=CARTESIAN_POINT('Ctrl Pts',(-0.104989479152703,-1.,2.1307270488718));
#27330=CARTESIAN_POINT('Ctrl Pts',(-0.107690435231068,-1.,2.12499752306927));
#27331=CARTESIAN_POINT('Ctrl Pts',(-0.11035023613502,-1.,2.11926155590849));
#27332=CARTESIAN_POINT('Ctrl Pts',(-0.112968534419746,-1.,2.11351924490335));
#27333=CARTESIAN_POINT('Ctrl Pts',(-0.115544957687941,-1.,2.10777050261359));
#27334=CARTESIAN_POINT('Ctrl Pts',(-0.118079107988368,-1.,2.10201512132945));
#27335=CARTESIAN_POINT('Ctrl Pts',(-0.120570567965129,-1.,2.09625292867756));
#27336=CARTESIAN_POINT('Ctrl Pts',(-0.123018905621083,-1.,2.09048392424826));
#27337=CARTESIAN_POINT('Ctrl Pts',(-0.125423679412058,-1.,2.08470840653628));
#27338=CARTESIAN_POINT('Ctrl Pts',(-0.127784445276116,-1.,2.07892715110967));
#27339=CARTESIAN_POINT('Ctrl Pts',(-0.130100748328401,-1.,2.07314114713047));
#27340=CARTESIAN_POINT('Ctrl Pts',(-0.13237211154771,-1.,2.06735123910319));
#27341=CARTESIAN_POINT('Ctrl Pts',(-0.134598026192107,-1.,2.06155781517844));
#27342=CARTESIAN_POINT('Ctrl Pts',(-0.136777941218044,-1.,2.0557604441427));
#27343=CARTESIAN_POINT('Ctrl Pts',(-0.138911255368966,-1.,2.04995762001333));
#27344=CARTESIAN_POINT('Ctrl Pts',(-0.140997332152546,-1.,2.04414757947919));
#27345=CARTESIAN_POINT('Ctrl Pts',(-0.143035515058208,-1.,2.03832911025913));
#27346=CARTESIAN_POINT('Ctrl Pts',(-0.145025140186058,-1.,2.03250223739941));
#27347=CARTESIAN_POINT('Ctrl Pts',(-0.146965557332586,-1.,2.02666926182017));
#27348=CARTESIAN_POINT('Ctrl Pts',(-0.148856124775343,-1.,2.02083464969897));
#27349=CARTESIAN_POINT('Ctrl Pts',(-0.150696157673084,-1.,2.01500291940243));
#27350=CARTESIAN_POINT('Ctrl Pts',(-0.152484883621452,-1.,2.00917680318426));
#27351=CARTESIAN_POINT('Ctrl Pts',(-0.154221403049719,-1.,2.00335565310539));
#27352=CARTESIAN_POINT('Ctrl Pts',(-0.155904629548775,-1.,1.99753284771487));
#27353=CARTESIAN_POINT('Ctrl Pts',(-0.157533331459215,-1.,1.99169810931893));
#27354=CARTESIAN_POINT('Ctrl Pts',(-0.159106226437289,-1.,1.98584238283279));
#27355=CARTESIAN_POINT('Ctrl Pts',(-0.16062206078461,-1.,1.97996195437557));
#27356=CARTESIAN_POINT('Ctrl Pts',(-0.162079693556302,-1.,1.97406280235204));
#27357=CARTESIAN_POINT('Ctrl Pts',(-0.16347818545776,-1.,1.96816512678));
#27358=CARTESIAN_POINT('Ctrl Pts',(-0.1648165689203,-1.,1.96229379940174));
#27359=CARTESIAN_POINT('Ctrl Pts',(-0.166093592002833,-1.,1.95646759718755));
#27360=CARTESIAN_POINT('Ctrl Pts',(-0.167307501784469,-1.,1.95069027794286));
#27361=CARTESIAN_POINT('Ctrl Pts',(-0.168455741607516,-1.,1.94493757756879));
#27362=CARTESIAN_POINT('Ctrl Pts',(-0.169534904817425,-1.,1.93915639211497));
#27363=CARTESIAN_POINT('Ctrl Pts',(-0.170541253116136,-1.,1.93329183155455));
#27364=CARTESIAN_POINT('Ctrl Pts',(-0.17147119153296,-1.,1.92731093582));
#27365=CARTESIAN_POINT('Ctrl Pts',(-0.172321621259557,-1.,1.92122334398034));
#27366=CARTESIAN_POINT('Ctrl Pts',(-0.173090695383619,-1.,1.91511429159681));
#27367=CARTESIAN_POINT('Ctrl Pts',(-0.173776635257984,-1.,1.90911693975475));
#27368=CARTESIAN_POINT('Ctrl Pts',(-0.174375518661222,-1.,1.90335253863003));
#27369=CARTESIAN_POINT('Ctrl Pts',(-0.174879405091277,-1.,1.89788101117148));
#27370=CARTESIAN_POINT('Ctrl Pts',(-0.175274276190664,-1.,1.89264630198279));
#27371=CARTESIAN_POINT('Ctrl Pts',(-0.175538155840286,-1.,1.88742606272818));
#27372=CARTESIAN_POINT('Ctrl Pts',(-0.175644148889271,-1.,1.88188663144846));
#27373=CARTESIAN_POINT('Ctrl Pts',(-0.175563480746206,-1.,1.87563767773249));
#27374=CARTESIAN_POINT('Ctrl Pts',(-0.175268337590901,-1.,1.86828349694972));
#27375=CARTESIAN_POINT('Ctrl Pts',(-0.174735259276856,-1.,1.85948367089838));
#27376=CARTESIAN_POINT('Ctrl Pts',(-0.173946627589401,-1.,1.84898113200543));
#27377=CARTESIAN_POINT('Ctrl Pts',(-0.17288944289442,-1.,1.83658380530747));
#27378=CARTESIAN_POINT('Ctrl Pts',(-0.171554770207306,-1.,1.82215766815414));
#27379=CARTESIAN_POINT('Ctrl Pts',(-0.169936923908078,-1.,1.80561530633924));
#27380=CARTESIAN_POINT('Ctrl Pts',(-0.16803277280837,-1.,1.78690649988931));
#27381=CARTESIAN_POINT('Ctrl Pts',(-0.166279355148738,-1.,1.77018771687692));
#27382=CARTESIAN_POINT('Ctrl Pts',(-0.164834765708484,-1.,1.75666056640041));
#27383=CARTESIAN_POINT('Ctrl Pts',(-0.163814161002474,-1.,1.74720349503904));
#27384=CARTESIAN_POINT('Ctrl Pts',(-0.163289472382896,-1.,1.74236521665491));
#27385=CARTESIAN_POINT('',(-0.383122945602004,-1.,1.7075470150345));
#27386=CARTESIAN_POINT('Origin',(0.,-1.,0.));
#27387=CARTESIAN_POINT('',(-0.61342227326009,-1.,2.11275013067528));
#27388=CARTESIAN_POINT('Ctrl Pts',(-0.383122945602004,-1.,1.7075470150345));
#27389=CARTESIAN_POINT('Ctrl Pts',(-0.384119047314215,-1.,1.71231062891398));
#27390=CARTESIAN_POINT('Ctrl Pts',(-0.386070790323281,-1.,1.72162022244582));
#27391=CARTESIAN_POINT('Ctrl Pts',(-0.388877023502615,-1.,1.73493170972829));
#27392=CARTESIAN_POINT('Ctrl Pts',(-0.392375812285395,-1.,1.75137405310193));
#27393=CARTESIAN_POINT('Ctrl Pts',(-0.396346196110688,-1.,1.76975560043442));
#27394=CARTESIAN_POINT('Ctrl Pts',(-0.399919403774155,-1.,1.78598826343754));
#27395=CARTESIAN_POINT('Ctrl Pts',(-0.403107976163396,-1.,1.80012077173238));
#27396=CARTESIAN_POINT('Ctrl Pts',(-0.405933518407175,-1.,1.81223801812013));
#27397=CARTESIAN_POINT('Ctrl Pts',(-0.408428948106227,-1.,1.82247022677562));
#27398=CARTESIAN_POINT('Ctrl Pts',(-0.410641256301276,-1.,1.83100408895047));
#27399=CARTESIAN_POINT('Ctrl Pts',(-0.412633125322945,-1.,1.8380895347617));
#27400=CARTESIAN_POINT('Ctrl Pts',(-0.414487438255542,-1.,1.84405757074218));
#27401=CARTESIAN_POINT('Ctrl Pts',(-0.416300022039885,-1.,1.84929312930314));
#27402=CARTESIAN_POINT('Ctrl Pts',(-0.418164129144045,-1.,1.8541763285645));
#27403=CARTESIAN_POINT('Ctrl Pts',(-0.420157287975583,-1.,1.8590328109667));
#27404=CARTESIAN_POINT('Ctrl Pts',(-0.422327307417885,-1.,1.86408083333863));
#27405=CARTESIAN_POINT('Ctrl Pts',(-0.424678177290876,-1.,1.8693780394412));
#27406=CARTESIAN_POINT('Ctrl Pts',(-0.427183828518743,-1.,1.87486989291333));
#27407=CARTESIAN_POINT('Ctrl Pts',(-0.429803062482217,-1.,1.88044229001778));
#27408=CARTESIAN_POINT('Ctrl Pts',(-0.432493038548833,-1.,1.88596913666828));
#27409=CARTESIAN_POINT('Ctrl Pts',(-0.43522566096358,-1.,1.89136993975585));
#27410=CARTESIAN_POINT('Ctrl Pts',(-0.437995003948443,-1.,1.89663648956549));
#27411=CARTESIAN_POINT('Ctrl Pts',(-0.440807833704161,-1.,1.90180124389137));
#27412=CARTESIAN_POINT('Ctrl Pts',(-0.44367755684917,-1.,1.90691756144906));
#27413=CARTESIAN_POINT('Ctrl Pts',(-0.446617343485651,-1.,1.91203699981095));
#27414=CARTESIAN_POINT('Ctrl Pts',(-0.449632260106572,-1.,1.91718342555717));
#27415=CARTESIAN_POINT('Ctrl Pts',(-0.452719478359356,-1.,1.9223538064847));
#27416=CARTESIAN_POINT('Ctrl Pts',(-0.455872005174335,-1.,1.92753067150461));
#27417=CARTESIAN_POINT('Ctrl Pts',(-0.459081234547931,-1.,1.93269066517936));
#27418=CARTESIAN_POINT('Ctrl Pts',(-0.462340031009087,-1.,1.93781486640834));
#27419=CARTESIAN_POINT('Ctrl Pts',(-0.465645462026065,-1.,1.94289794196205));
#27420=CARTESIAN_POINT('Ctrl Pts',(-0.468997482913158,-1.,1.94794381136524));
#27421=CARTESIAN_POINT('Ctrl Pts',(-0.47239767226408,-1.,1.95296148278136));
#27422=CARTESIAN_POINT('Ctrl Pts',(-0.475848034683172,-1.,1.95796111148175));
#27423=CARTESIAN_POINT('Ctrl Pts',(-0.479349583074846,-1.,1.96294933055938));
#27424=CARTESIAN_POINT('Ctrl Pts',(-0.482901662120687,-1.,1.96792703422358));
#27425=CARTESIAN_POINT('Ctrl Pts',(-0.486502692907661,-1.,1.97289186263272));
#27426=CARTESIAN_POINT('Ctrl Pts',(-0.490150627860955,-1.,1.97783973019229));
#27427=CARTESIAN_POINT('Ctrl Pts',(-0.493843476541492,-1.,1.9827665876182));
#27428=CARTESIAN_POINT('Ctrl Pts',(-0.497579909545564,-1.,1.98767044752929));
#27429=CARTESIAN_POINT('Ctrl Pts',(-0.501359287727129,-1.,1.9925514912615));
#27430=CARTESIAN_POINT('Ctrl Pts',(-0.505181361323011,-1.,1.99741107463567));
#27431=CARTESIAN_POINT('Ctrl Pts',(-0.509046069886152,-1.,2.00225107134733));
#27432=CARTESIAN_POINT('Ctrl Pts',(-0.512953306961814,-1.,2.00707309946955));
#27433=CARTESIAN_POINT('Ctrl Pts',(-0.516902681728733,-1.,2.01187773939257));
#27434=CARTESIAN_POINT('Ctrl Pts',(-0.520893590399428,-1.,2.01666477917305));
#27435=CARTESIAN_POINT('Ctrl Pts',(-0.524925318333518,-1.,2.02143356304712));
#27436=CARTESIAN_POINT('Ctrl Pts',(-0.528997127241911,-1.,2.02618329083289));
#27437=CARTESIAN_POINT('Ctrl Pts',(-0.533108355132905,-1.,2.03091336214401));
#27438=CARTESIAN_POINT('Ctrl Pts',(-0.537258489833134,-1.,2.03562362953993));
#27439=CARTESIAN_POINT('Ctrl Pts',(-0.54144712061552,-1.,2.0403142269048));
#27440=CARTESIAN_POINT('Ctrl Pts',(-0.545673903817348,-1.,2.0449854471456));
#27441=CARTESIAN_POINT('Ctrl Pts',(-0.549938525150342,-1.,2.04963761077974));
#27442=CARTESIAN_POINT('Ctrl Pts',(-0.55424065746411,-1.,2.05427091604482));
#27443=CARTESIAN_POINT('Ctrl Pts',(-0.558579940185467,-1.,2.05888537756571));
#27444=CARTESIAN_POINT('Ctrl Pts',(-0.562955993082574,-1.,2.06348090160697));
#27445=CARTESIAN_POINT('Ctrl Pts',(-0.567368421181229,-1.,2.06805732997383));
#27446=CARTESIAN_POINT('Ctrl Pts',(-0.571816823242411,-1.,2.07261449292757));
#27447=CARTESIAN_POINT('Ctrl Pts',(-0.576300797416275,-1.,2.07715226767361));
#27448=CARTESIAN_POINT('Ctrl Pts',(-0.580819952107257,-1.,2.08167059018138));
#27449=CARTESIAN_POINT('Ctrl Pts',(-0.585373918990895,-1.,2.086169437277));
#27450=CARTESIAN_POINT('Ctrl Pts',(-0.589962365403189,-1.,2.09064881812053));
#27451=CARTESIAN_POINT('Ctrl Pts',(-0.594585006052824,-1.,2.09510876220501));
#27452=CARTESIAN_POINT('Ctrl Pts',(-0.599241616422144,-1.,2.09954930865331));
#27453=CARTESIAN_POINT('Ctrl Pts',(-0.603932030738212,-1.,2.10397049887709));
#27454=CARTESIAN_POINT('Ctrl Pts',(-0.607711315456826,-1.,2.10749199615859));
#27455=CARTESIAN_POINT('Ctrl Pts',(-0.610560911691113,-1.,2.11012443807661));
#27456=CARTESIAN_POINT('Ctrl Pts',(-0.61246736556225,-1.,2.11187554260142));
#27457=CARTESIAN_POINT('Ctrl Pts',(-0.61342227326009,-1.,2.11275013067528));
#27458=CARTESIAN_POINT('',(-0.745574324794401,-1.,2.0698113262342));
#27459=CARTESIAN_POINT('',(-0.61342227326009,-1.,2.11275013067528));
#27460=CARTESIAN_POINT('',(-0.693717979106306,-1.,1.60662857109684));
#27461=CARTESIAN_POINT('Ctrl Pts',(-0.745574324794401,-1.,2.0698113262342));
#27462=CARTESIAN_POINT('Ctrl Pts',(-0.74583279137781,-1.,2.06854248895575));
#27463=CARTESIAN_POINT('Ctrl Pts',(-0.746345871542696,-1.,2.06600523016401));
#27464=CARTESIAN_POINT('Ctrl Pts',(-0.747103932785504,-1.,2.06220058927162));
#27465=CARTESIAN_POINT('Ctrl Pts',(-0.748091554181101,-1.,2.05713023030263));
#27466=CARTESIAN_POINT('Ctrl Pts',(-0.749287468663053,-1.,2.05079645591606));
#27467=CARTESIAN_POINT('Ctrl Pts',(-0.750444657874758,-1.,2.04446689147754));
#27468=CARTESIAN_POINT('Ctrl Pts',(-0.751562963361384,-1.,2.03814160092173));
#27469=CARTESIAN_POINT('Ctrl Pts',(-0.752642180488104,-1.,2.03182068456467));
#27470=CARTESIAN_POINT('Ctrl Pts',(-0.753682061113766,-1.,2.02550428623587));
#27471=CARTESIAN_POINT('Ctrl Pts',(-0.75468233072352,-1.,2.01919259406003));
#27472=CARTESIAN_POINT('Ctrl Pts',(-0.7556427049581,-1.,2.01288584328149));
#27473=CARTESIAN_POINT('Ctrl Pts',(-0.756562904646496,-1.,2.00658431587682));
#27474=CARTESIAN_POINT('Ctrl Pts',(-0.757442676862341,-1.,2.00028834739072));
#27475=CARTESIAN_POINT('Ctrl Pts',(-0.758281796766377,-1.,1.9939983109871));
#27476=CARTESIAN_POINT('Ctrl Pts',(-0.759080037802243,-1.,1.98771456680806));
#27477=CARTESIAN_POINT('Ctrl Pts',(-0.759837147452135,-1.,1.98143741418156));
#27478=CARTESIAN_POINT('Ctrl Pts',(-0.760552825409855,-1.,1.97516705321521));
#27479=CARTESIAN_POINT('Ctrl Pts',(-0.761226690483986,-1.,1.96890351582545));
#27480=CARTESIAN_POINT('Ctrl Pts',(-0.761858300014575,-1.,1.96264672744229));
#27481=CARTESIAN_POINT('Ctrl Pts',(-0.762447203806263,-1.,1.95639665309893));
#27482=CARTESIAN_POINT('Ctrl Pts',(-0.762992990878774,-1.,1.95015342590025));
#27483=CARTESIAN_POINT('Ctrl Pts',(-0.76349533353858,-1.,1.94391746617626));
#27484=CARTESIAN_POINT('Ctrl Pts',(-0.763954049121393,-1.,1.93768964875867));
#27485=CARTESIAN_POINT('Ctrl Pts',(-0.764369010673889,-1.,1.93147105496367));
#27486=CARTESIAN_POINT('Ctrl Pts',(-0.764740025488189,-1.,1.92526263537041));
#27487=CARTESIAN_POINT('Ctrl Pts',(-0.765066729667095,-1.,1.91906491634197));
#27488=CARTESIAN_POINT('Ctrl Pts',(-0.765348465884739,-1.,1.91287765805174));
#27489=CARTESIAN_POINT('Ctrl Pts',(-0.765584196937936,-1.,1.90669961402362));
#27490=CARTESIAN_POINT('Ctrl Pts',(-0.765772772593395,-1.,1.90052930393599));
#27491=CARTESIAN_POINT('Ctrl Pts',(-0.765913193856979,-1.,1.89436577771389));
#27492=CARTESIAN_POINT('Ctrl Pts',(-0.76600483706209,-1.,1.88820926433409));
#27493=CARTESIAN_POINT('Ctrl Pts',(-0.766047794851869,-1.,1.88206215302561));
#27494=CARTESIAN_POINT('Ctrl Pts',(-0.766042837036759,-1.,1.87592888967886));
#27495=CARTESIAN_POINT('Ctrl Pts',(-0.765990708546111,-1.,1.86981398314345));
#27496=CARTESIAN_POINT('Ctrl Pts',(-0.765891519092557,-1.,1.86372027063314));
#27497=CARTESIAN_POINT('Ctrl Pts',(-0.765744212909305,-1.,1.85764741390391));
#27498=CARTESIAN_POINT('Ctrl Pts',(-0.765545710619023,-1.,1.85158945130054));
#27499=CARTESIAN_POINT('Ctrl Pts',(-0.765291664861971,-1.,1.8455369887591));
#27500=CARTESIAN_POINT('Ctrl Pts',(-0.764978057881687,-1.,1.83948181064823));
#27501=CARTESIAN_POINT('Ctrl Pts',(-0.764602549687845,-1.,1.8334207722714));
#27502=CARTESIAN_POINT('Ctrl Pts',(-0.764165902606055,-1.,1.8273599120008));
#27503=CARTESIAN_POINT('Ctrl Pts',(-0.763673465462854,-1.,1.82131873145297));
#27504=CARTESIAN_POINT('Ctrl Pts',(-0.763132003836783,-1.,1.81532118405566));
#27505=CARTESIAN_POINT('Ctrl Pts',(-0.762546129464036,-1.,1.80938551463989));
#27506=CARTESIAN_POINT('Ctrl Pts',(-0.761915336443516,-1.,1.80351583877334));
#27507=CARTESIAN_POINT('Ctrl Pts',(-0.761229695230359,-1.,1.79768986997735));
#27508=CARTESIAN_POINT('Ctrl Pts',(-0.760469555880425,-1.,1.79185815610802));
#27509=CARTESIAN_POINT('Ctrl Pts',(-0.759614401109868,-1.,1.78596964884526));
#27510=CARTESIAN_POINT('Ctrl Pts',(-0.75865062667738,-1.,1.77999411220912));
#27511=CARTESIAN_POINT('Ctrl Pts',(-0.757578264077238,-1.,1.77394167108342));
#27512=CARTESIAN_POINT('Ctrl Pts',(-0.756421896028403,-1.,1.76789396003141));
#27513=CARTESIAN_POINT('Ctrl Pts',(-0.755220979975262,-1.,1.7619781724032));
#27514=CARTESIAN_POINT('Ctrl Pts',(-0.75400925402848,-1.,1.75631083600175));
#27515=CARTESIAN_POINT('Ctrl Pts',(-0.752797683531377,-1.,1.75095139468809));
#27516=CARTESIAN_POINT('Ctrl Pts',(-0.751555614163629,-1.,1.74585086852298));
#27517=CARTESIAN_POINT('Ctrl Pts',(-0.75019343597954,-1.,1.74080458266705));
#27518=CARTESIAN_POINT('Ctrl Pts',(-0.748582462954855,-1.,1.73550351679848));
#27519=CARTESIAN_POINT('Ctrl Pts',(-0.746574710096436,-1.,1.72958533647399));
#27520=CARTESIAN_POINT('Ctrl Pts',(-0.744021445433764,-1.,1.7226822991693));
#27521=CARTESIAN_POINT('Ctrl Pts',(-0.740795162032088,-1.,1.71447789751927));
#27522=CARTESIAN_POINT('Ctrl Pts',(-0.736799665724771,-1.,1.70473309006121));
#27523=CARTESIAN_POINT('Ctrl Pts',(-0.731963238697195,-1.,1.69326921975743));
#27524=CARTESIAN_POINT('Ctrl Pts',(-0.726235967997433,-1.,1.67996158455503));
#27525=CARTESIAN_POINT('Ctrl Pts',(-0.719585433804282,-1.,1.6647288055568));
#27526=CARTESIAN_POINT('Ctrl Pts',(-0.711993139355394,-1.,1.64752408832016));
#27527=CARTESIAN_POINT('Ctrl Pts',(-0.705159151988319,-1.,1.63216541664676));
#27528=CARTESIAN_POINT('Ctrl Pts',(-0.699605146405088,-1.,1.61974673472612));
#27529=CARTESIAN_POINT('Ctrl Pts',(-0.695712097881194,-1.,1.61106790958151));
#27530=CARTESIAN_POINT('Ctrl Pts',(-0.693717979106306,-1.,1.60662857109684));
#27531=CARTESIAN_POINT('',(-0.892032620296855,-1.,1.5055822144029));
#27532=CARTESIAN_POINT('Origin',(0.,-1.,0.));
#27533=CARTESIAN_POINT('',(-1.23627494547115,-1.,1.81978687191668));
#27534=CARTESIAN_POINT('Ctrl Pts',(-0.892032620296855,-1.,1.5055822144029));
#27535=CARTESIAN_POINT('Ctrl Pts',(-0.894452006964543,-1.,1.50980486806688));
#27536=CARTESIAN_POINT('Ctrl Pts',(-0.899185047483511,-1.,1.51805569590094));
#27537=CARTESIAN_POINT('Ctrl Pts',(-0.905967409625651,-1.,1.52984849887993));
#27538=CARTESIAN_POINT('Ctrl Pts',(-0.914375919026456,-1.,1.54440491149498));
#27539=CARTESIAN_POINT('Ctrl Pts',(-0.923832188944341,-1.,1.56065988578893));
#27540=CARTESIAN_POINT('Ctrl Pts',(-0.932246680108685,-1.,1.57499388382243));
#27541=CARTESIAN_POINT('Ctrl Pts',(-0.939646377893399,-1.,1.58744937487176));
#27542=CARTESIAN_POINT('Ctrl Pts',(-0.946078063315257,-1.,1.59810042043673));
#27543=CARTESIAN_POINT('Ctrl Pts',(-0.951613284356035,-1.,1.60706069896936));
#27544=CARTESIAN_POINT('Ctrl Pts',(-0.956354422920671,-1.,1.61449324337085));
#27545=CARTESIAN_POINT('Ctrl Pts',(-0.960438326101729,-1.,1.62061638140221));
#27546=CARTESIAN_POINT('Ctrl Pts',(-0.964046107040536,-1.,1.62571930670187));
#27547=CARTESIAN_POINT('Ctrl Pts',(-0.967387853230345,-1.,1.63013849959461));
#27548=CARTESIAN_POINT('Ctrl Pts',(-0.970669715997509,-1.,1.63420665729798));
#27549=CARTESIAN_POINT('Ctrl Pts',(-0.974066058287418,-1.,1.63820952658144));
#27550=CARTESIAN_POINT('Ctrl Pts',(-0.977689794119416,-1.,1.64233990826687));
#27551=CARTESIAN_POINT('Ctrl Pts',(-0.981562530939489,-1.,1.64665139190656));
#27552=CARTESIAN_POINT('Ctrl Pts',(-0.985642622920821,-1.,1.65110016612638));
#27553=CARTESIAN_POINT('Ctrl Pts',(-0.989855627854165,-1.,1.65559044289699));
#27554=CARTESIAN_POINT('Ctrl Pts',(-0.994121836661306,-1.,1.66001553809947));
#27555=CARTESIAN_POINT('Ctrl Pts',(-0.998389654952758,-1.,1.66430758030376));
#27556=CARTESIAN_POINT('Ctrl Pts',(-1.00265091003727,-1.,1.66846059277303));
#27557=CARTESIAN_POINT('Ctrl Pts',(-1.00692206696414,-1.,1.67250335383293));
#27558=CARTESIAN_POINT('Ctrl Pts',(-1.01123236493511,-1.,1.67648246776464));
#27559=CARTESIAN_POINT('Ctrl Pts',(-1.01561026162773,-1.,1.68044289894798));
#27560=CARTESIAN_POINT('Ctrl Pts',(-1.02006795074201,-1.,1.68440578021706));
#27561=CARTESIAN_POINT('Ctrl Pts',(-1.02460180535255,-1.,1.68836910178447));
#27562=CARTESIAN_POINT('Ctrl Pts',(-1.02919977579147,-1.,1.69231840863458));
#27563=CARTESIAN_POINT('Ctrl Pts',(-1.03384646003588,-1.,1.69623414782771));
#27564=CARTESIAN_POINT('Ctrl Pts',(-1.03852922490789,-1.,1.70010052930962));
#27565=CARTESIAN_POINT('Ctrl Pts',(-1.04324363334554,-1.,1.70391338707982));
#27566=CARTESIAN_POINT('Ctrl Pts',(-1.04799085404995,-1.,1.70767646263649));
#27567=CARTESIAN_POINT('Ctrl Pts',(-1.05277517202855,-1.,1.71139783543989));
#27568=CARTESIAN_POINT('Ctrl Pts',(-1.05760163192479,-1.,1.7150865442702));
#27569=CARTESIAN_POINT('Ctrl Pts',(-1.06247324680647,-1.,1.71874858456904));
#27570=CARTESIAN_POINT('Ctrl Pts',(-1.06738966975462,-1.,1.72238500928453));
#27571=CARTESIAN_POINT('Ctrl Pts',(-1.07234866990252,-1.,1.72599406198488));
#27572=CARTESIAN_POINT('Ctrl Pts',(-1.0773470373727,-1.,1.72957248977424));
#27573=CARTESIAN_POINT('Ctrl Pts',(-1.08238162784749,-1.,1.73311705663407));
#27574=CARTESIAN_POINT('Ctrl Pts',(-1.08745056285427,-1.,1.73662628326091));
#27575=CARTESIAN_POINT('Ctrl Pts',(-1.09255329056493,-1.,1.74010053962247));
#27576=CARTESIAN_POINT('Ctrl Pts',(-1.09768999241225,-1.,1.74354119236208));
#27577=CARTESIAN_POINT('Ctrl Pts',(-1.10286118991143,-1.,1.74695004214923));
#27578=CARTESIAN_POINT('Ctrl Pts',(-1.10806728183007,-1.,1.7503286607592));
#27579=CARTESIAN_POINT('Ctrl Pts',(-1.11330807582551,-1.,1.7536777209463));
#27580=CARTESIAN_POINT('Ctrl Pts',(-1.11858293216763,-1.,1.75699720772105));
#27581=CARTESIAN_POINT('Ctrl Pts',(-1.12389096855086,-1.,1.76028671825096));
#27582=CARTESIAN_POINT('Ctrl Pts',(-1.12923123555075,-1.,1.7635457196617));
#27583=CARTESIAN_POINT('Ctrl Pts',(-1.1346029180462,-1.,1.76677384551862));
#27584=CARTESIAN_POINT('Ctrl Pts',(-1.14000548336975,-1.,1.76997111386769));
#27585=CARTESIAN_POINT('Ctrl Pts',(-1.1454385822692,-1.,1.77313777896194));
#27586=CARTESIAN_POINT('Ctrl Pts',(-1.15090197841515,-1.,1.7762742255701));
#27587=CARTESIAN_POINT('Ctrl Pts',(-1.15639547194698,-1.,1.77938085564275));
#27588=CARTESIAN_POINT('Ctrl Pts',(-1.16191881298499,-1.,1.78245795881009));
#27589=CARTESIAN_POINT('Ctrl Pts',(-1.16747166312303,-1.,1.78550566040443));
#27590=CARTESIAN_POINT('Ctrl Pts',(-1.17305363177328,-1.,1.78852398877616));
#27591=CARTESIAN_POINT('Ctrl Pts',(-1.17866429440809,-1.,1.79151291552689));
#27592=CARTESIAN_POINT('Ctrl Pts',(-1.18430321697432,-1.,1.79447240321515));
#27593=CARTESIAN_POINT('Ctrl Pts',(-1.18996997934445,-1.,1.79740245923478));
#27594=CARTESIAN_POINT('Ctrl Pts',(-1.19566418930242,-1.,1.80030314369879));
#27595=CARTESIAN_POINT('Ctrl Pts',(-1.20138548938974,-1.,1.80317454838603));
#27596=CARTESIAN_POINT('Ctrl Pts',(-1.20713356605475,-1.,1.80601678480707));
#27597=CARTESIAN_POINT('Ctrl Pts',(-1.21290815708314,-1.,1.80882996917129));
#27598=CARTESIAN_POINT('Ctrl Pts',(-1.21870906103557,-1.,1.81161420806656));
#27599=CARTESIAN_POINT('Ctrl Pts',(-1.2245361330495,-1.,1.81436959210434));
#27600=CARTESIAN_POINT('Ctrl Pts',(-1.2292186489137,-1.,1.8165508718364));
#27601=CARTESIAN_POINT('Ctrl Pts',(-1.2327422452705,-1.,1.81817389921279));
#27602=CARTESIAN_POINT('Ctrl Pts',(-1.23509651170476,-1.,1.81925017193666));
#27603=CARTESIAN_POINT('Ctrl Pts',(-1.23627494547115,-1.,1.81978687191668));
#27604=CARTESIAN_POINT('',(-1.34869019493419,-1.,1.73811241238545));
#27605=CARTESIAN_POINT('',(-1.23627494547115,-1.,1.81978687191668));
#27606=CARTESIAN_POINT('',(-1.15624053661742,-1.,1.31362392696032));
#27607=CARTESIAN_POINT('Ctrl Pts',(-1.34869019493419,-1.,1.73811241238545));
#27608=CARTESIAN_POINT('Ctrl Pts',(-1.34854391898045,-1.,1.73682580585691));
#27609=CARTESIAN_POINT('Ctrl Pts',(-1.34824783112887,-1.,1.73425417885907));
#27610=CARTESIAN_POINT('Ctrl Pts',(-1.34779309152035,-1.,1.7304014965394));
#27611=CARTESIAN_POINT('Ctrl Pts',(-1.34716554819527,-1.,1.72527410680674));
#27612=CARTESIAN_POINT('Ctrl Pts',(-1.34634568653227,-1.,1.7188807715049));
#27613=CARTESIAN_POINT('Ctrl Pts',(-1.34549029589416,-1.,1.71250340686822));
#27614=CARTESIAN_POINT('Ctrl Pts',(-1.34459924533831,-1.,1.70614212266738));
#27615=CARTESIAN_POINT('Ctrl Pts',(-1.34367237124483,-1.,1.69979707754427));
#27616=CARTESIAN_POINT('Ctrl Pts',(-1.34270948206319,-1.,1.6934684849687));
#27617=CARTESIAN_POINT('Ctrl Pts',(-1.341710374848,-1.,1.68715660868764));
#27618=CARTESIAN_POINT('Ctrl Pts',(-1.34067485185203,-1.,1.68086176030362));
#27619=CARTESIAN_POINT('Ctrl Pts',(-1.3396027347034,-1.,1.67458429426086));
#27620=CARTESIAN_POINT('Ctrl Pts',(-1.33849388654388,-1.,1.66832460783989));
#27621=CARTESIAN_POINT('Ctrl Pts',(-1.33734820885262,-1.,1.66208312541983));
#27622=CARTESIAN_POINT('Ctrl Pts',(-1.33616559745172,-1.,1.65586025952593));
#27623=CARTESIAN_POINT('Ctrl Pts',(-1.33494590467993,-1.,1.6496563728683));
#27624=CARTESIAN_POINT('Ctrl Pts',(-1.33368890676572,-1.,1.6434717485603));
#27625=CARTESIAN_POINT('Ctrl Pts',(-1.33239425103724,-1.,1.63730653475089));
#27626=CARTESIAN_POINT('Ctrl Pts',(-1.33106149345645,-1.,1.63116079730923));
#27627=CARTESIAN_POINT('Ctrl Pts',(-1.3296901950568,-1.,1.62503464209797));
#27628=CARTESIAN_POINT('Ctrl Pts',(-1.32828000610449,-1.,1.61892832270724));
#27629=CARTESIAN_POINT('Ctrl Pts',(-1.32683074483356,-1.,1.6128423401575));
#27630=CARTESIAN_POINT('Ctrl Pts',(-1.32534250785782,-1.,1.60677758290954));
#27631=CARTESIAN_POINT('Ctrl Pts',(-1.32381550858256,-1.,1.60073511858687));
#27632=CARTESIAN_POINT('Ctrl Pts',(-1.32224985747682,-1.,1.59471591079403));
#27633=CARTESIAN_POINT('Ctrl Pts',(-1.32064537110892,-1.,1.58872057258245));
#27634=CARTESIAN_POINT('Ctrl Pts',(-1.31900135021432,-1.,1.58274907898834));
#27635=CARTESIAN_POINT('Ctrl Pts',(-1.31731642317187,-1.,1.5768005650559));
#27636=CARTESIAN_POINT('Ctrl Pts',(-1.31558903860016,-1.,1.57087397835723));
#27637=CARTESIAN_POINT('Ctrl Pts',(-1.31381795281002,-1.,1.56496872402353));
#27638=CARTESIAN_POINT('Ctrl Pts',(-1.31200264341696,-1.,1.55908521254821));
#27639=CARTESIAN_POINT('Ctrl Pts',(-1.31014393684222,-1.,1.55322568759481));
#27640=CARTESIAN_POINT('Ctrl Pts',(-1.30824393907473,-1.,1.54739413957185));
#27641=CARTESIAN_POINT('Ctrl Pts',(-1.30630475189556,-1.,1.54159462645432));
#27642=CARTESIAN_POINT('Ctrl Pts',(-1.30432735639489,-1.,1.53582981268977));
#27643=CARTESIAN_POINT('Ctrl Pts',(-1.30231064395568,-1.,1.53009970283891));
#27644=CARTESIAN_POINT('Ctrl Pts',(-1.30024984366328,-1.,1.52439957861062));
#27645=CARTESIAN_POINT('Ctrl Pts',(-1.29813791800747,-1.,1.51872184912724));
#27646=CARTESIAN_POINT('Ctrl Pts',(-1.29596850710509,-1.,1.51305994241402));
#27647=CARTESIAN_POINT('Ctrl Pts',(-1.29373841372842,-1.,1.50741159078365));
#27648=CARTESIAN_POINT('Ctrl Pts',(-1.29145022885181,-1.,1.50178230149776));
#27649=CARTESIAN_POINT('Ctrl Pts',(-1.28911506584254,-1.,1.49618896881754));
#27650=CARTESIAN_POINT('Ctrl Pts',(-1.2867467611644,-1.,1.4906522831278));
#27651=CARTESIAN_POINT('Ctrl Pts',(-1.28435533880201,-1.,1.4851881711891));
#27652=CARTESIAN_POINT('Ctrl Pts',(-1.28194158939517,-1.,1.47980070347095));
#27653=CARTESIAN_POINT('Ctrl Pts',(-1.2794891824849,-1.,1.4744717526707));
#27654=CARTESIAN_POINT('Ctrl Pts',(-1.27696414831089,-1.,1.46916035917133));
#27655=CARTESIAN_POINT('Ctrl Pts',(-1.27433119897822,-1.,1.46382431332476));
#27656=CARTESIAN_POINT('Ctrl Pts',(-1.27156805265289,-1.,1.45843906294697));
#27657=CARTESIAN_POINT('Ctrl Pts',(-1.2686778680489,-1.,1.45301422764247));
#27658=CARTESIAN_POINT('Ctrl Pts',(-1.26570925118868,-1.,1.44761985001662));
#27659=CARTESIAN_POINT('Ctrl Pts',(-1.26273903323859,-1.,1.44236470511303));
#27660=CARTESIAN_POINT('Ctrl Pts',(-1.25983531012005,-1.,1.43734919180848));
#27661=CARTESIAN_POINT('Ctrl Pts',(-1.25702687965755,-1.,1.43262645609691));
#27662=CARTESIAN_POINT('Ctrl Pts',(-1.25426945222639,-1.,1.42815938799387));
#27663=CARTESIAN_POINT('Ctrl Pts',(-1.2514145557001,-1.,1.42378102115575));
#27664=CARTESIAN_POINT('Ctrl Pts',(-1.24824430986571,-1.,1.41923722596025));
#27665=CARTESIAN_POINT('Ctrl Pts',(-1.24450600513056,-1.,1.41422913175179));
#27666=CARTESIAN_POINT('Ctrl Pts',(-1.23994455029534,-1.,1.40845295531283));
#27667=CARTESIAN_POINT('Ctrl Pts',(-1.23434087290423,-1.,1.40164708206106));
#27668=CARTESIAN_POINT('Ctrl Pts',(-1.22752961899387,-1.,1.39361389568796));
#27669=CARTESIAN_POINT('Ctrl Pts',(-1.21938737280852,-1.,1.38420564527715));
#27670=CARTESIAN_POINT('Ctrl Pts',(-1.20982812925645,-1.,1.37331915607905));
#27671=CARTESIAN_POINT('Ctrl Pts',(-1.1987959077932,-1.,1.36088705043885));
#27672=CARTESIAN_POINT('Ctrl Pts',(-1.18625865667441,-1.,1.34687054001093));
#27673=CARTESIAN_POINT('Ctrl Pts',(-1.17501305789857,-1.,1.33437539347008));
#27674=CARTESIAN_POINT('Ctrl Pts',(-1.16589330093588,-1.,1.32428080721772));
#27675=CARTESIAN_POINT('Ctrl Pts',(-1.15950888730809,-1.,1.31722977216397));
#27676=CARTESIAN_POINT('Ctrl Pts',(-1.15624053661742,-1.,1.31362392696032));
#27677=CARTESIAN_POINT('',(-1.31362392696033,-1.,1.15624053661742));
#27678=CARTESIAN_POINT('Origin',(0.,-1.,0.));
#27679=CARTESIAN_POINT('',(-1.73811241238545,-1.,1.34869019493419));
#27680=CARTESIAN_POINT('Ctrl Pts',(-1.31362392696033,-1.,1.15624053661742));
#27681=CARTESIAN_POINT('Ctrl Pts',(-1.3172297721596,-1.,1.15950888730433));
#27682=CARTESIAN_POINT('Ctrl Pts',(-1.32428080720544,-1.,1.16589330092532));
#27683=CARTESIAN_POINT('Ctrl Pts',(-1.33437539344842,-1.,1.17501305787994));
#27684=CARTESIAN_POINT('Ctrl Pts',(-1.34687053998157,-1.,1.18625865664915));
#27685=CARTESIAN_POINT('Ctrl Pts',(-1.36088705040677,-1.,1.1987959077656));
#27686=CARTESIAN_POINT('Ctrl Pts',(-1.37331915604962,-1.,1.20982812923113));
#27687=CARTESIAN_POINT('Ctrl Pts',(-1.38420564525391,-1.,1.21938737278853));
#27688=CARTESIAN_POINT('Ctrl Pts',(-1.39361389567257,-1.,1.22752961898063));
#27689=CARTESIAN_POINT('Ctrl Pts',(-1.40164708205345,-1.,1.23434087289768));
#27690=CARTESIAN_POINT('Ctrl Pts',(-1.40845295531151,-1.,1.23994455029421));
#27691=CARTESIAN_POINT('Ctrl Pts',(-1.41422913175437,-1.,1.24450600513278));
#27692=CARTESIAN_POINT('Ctrl Pts',(-1.41923722596421,-1.,1.24824430986911));
#27693=CARTESIAN_POINT('Ctrl Pts',(-1.42378102115911,-1.,1.25141455570299));
#27694=CARTESIAN_POINT('Ctrl Pts',(-1.42815938799555,-1.,1.25426945222783));
#27695=CARTESIAN_POINT('Ctrl Pts',(-1.43262645609679,-1.,1.25702687965744));
#27696=CARTESIAN_POINT('Ctrl Pts',(-1.43734919180719,-1.,1.25983531011894));
#27697=CARTESIAN_POINT('Ctrl Pts',(-1.44236470511145,-1.,1.26273903323723));
#27698=CARTESIAN_POINT('Ctrl Pts',(-1.44761985001544,-1.,1.26570925118767));
#27699=CARTESIAN_POINT('Ctrl Pts',(-1.45301422764205,-1.,1.26867786804854));
#27700=CARTESIAN_POINT('Ctrl Pts',(-1.45843906294725,-1.,1.27156805265312));
#27701=CARTESIAN_POINT('Ctrl Pts',(-1.4638243133254,-1.,1.27433119897877));
#27702=CARTESIAN_POINT('Ctrl Pts',(-1.46916035917197,-1.,1.27696414831144));
#27703=CARTESIAN_POINT('Ctrl Pts',(-1.4744717526711,-1.,1.27948918248524));
#27704=CARTESIAN_POINT('Ctrl Pts',(-1.47980070347102,-1.,1.28194158939522));
#27705=CARTESIAN_POINT('Ctrl Pts',(-1.48518817118891,-1.,1.28435533880184));
#27706=CARTESIAN_POINT('Ctrl Pts',(-1.4906522831275,-1.,1.28674676116415));
#27707=CARTESIAN_POINT('Ctrl Pts',(-1.49618896881729,-1.,1.28911506584232));
#27708=CARTESIAN_POINT('Ctrl Pts',(-1.50178230149764,-1.,1.29145022885171));
#27709=CARTESIAN_POINT('Ctrl Pts',(-1.50741159078367,-1.,1.29373841372843));
#27710=CARTESIAN_POINT('Ctrl Pts',(-1.51305994241412,-1.,1.29596850710518));
#27711=CARTESIAN_POINT('Ctrl Pts',(-1.51872184912735,-1.,1.29813791800757));
#27712=CARTESIAN_POINT('Ctrl Pts',(-1.5243995786107,-1.,1.30024984366334));
#27713=CARTESIAN_POINT('Ctrl Pts',(-1.53009970283893,-1.,1.3023106439557));
#27714=CARTESIAN_POINT('Ctrl Pts',(-1.53582981268976,-1.,1.30432735639487));
#27715=CARTESIAN_POINT('Ctrl Pts',(-1.54159462645428,-1.,1.30630475189553));
#27716=CARTESIAN_POINT('Ctrl Pts',(-1.54739413957183,-1.,1.30824393907471));
#27717=CARTESIAN_POINT('Ctrl Pts',(-1.55322568759481,-1.,1.31014393684221));
#27718=CARTESIAN_POINT('Ctrl Pts',(-1.55908521254822,-1.,1.31200264341696));
#27719=CARTESIAN_POINT('Ctrl Pts',(-1.56496872402352,-1.,1.31381795281002));
#27720=CARTESIAN_POINT('Ctrl Pts',(-1.57087397835721,-1.,1.31558903860015));
#27721=CARTESIAN_POINT('Ctrl Pts',(-1.57680056505585,-1.,1.31731642317183));
#27722=CARTESIAN_POINT('Ctrl Pts',(-1.58274907898829,-1.,1.31900135021428));
#27723=CARTESIAN_POINT('Ctrl Pts',(-1.58872057258244,-1.,1.32064537110891));
#27724=CARTESIAN_POINT('Ctrl Pts',(-1.59471591079408,-1.,1.32224985747686));
#27725=CARTESIAN_POINT('Ctrl Pts',(-1.600735118587,-1.,1.32381550858266));
#27726=CARTESIAN_POINT('Ctrl Pts',(-1.6067775829097,-1.,1.32534250785794));
#27727=CARTESIAN_POINT('Ctrl Pts',(-1.61284234015762,-1.,1.32683074483365));
#27728=CARTESIAN_POINT('Ctrl Pts',(-1.61892832270723,-1.,1.32828000610448));
#27729=CARTESIAN_POINT('Ctrl Pts',(-1.62503464209777,-1.,1.32969019505665));
#27730=CARTESIAN_POINT('Ctrl Pts',(-1.63116079730887,-1.,1.33106149345618));
#27731=CARTESIAN_POINT('Ctrl Pts',(-1.6373065347505,-1.,1.33239425103694));
#27732=CARTESIAN_POINT('Ctrl Pts',(-1.64347174856007,-1.,1.33368890676554));
#27733=CARTESIAN_POINT('Ctrl Pts',(-1.64965637286843,-1.,1.33494590468003));
#27734=CARTESIAN_POINT('Ctrl Pts',(-1.65586025952651,-1.,1.33616559745217));
#27735=CARTESIAN_POINT('Ctrl Pts',(-1.66208312542073,-1.,1.33734820885331));
#27736=CARTESIAN_POINT('Ctrl Pts',(-1.66832460784078,-1.,1.33849388654458));
#27737=CARTESIAN_POINT('Ctrl Pts',(-1.67458429426126,-1.,1.33960273470372));
#27738=CARTESIAN_POINT('Ctrl Pts',(-1.68086176030308,-1.,1.3406748518516));
#27739=CARTESIAN_POINT('Ctrl Pts',(-1.68715660868602,-1.,1.34171037484673));
#27740=CARTESIAN_POINT('Ctrl Pts',(-1.6934684849664,-1.,1.34270948206139));
#27741=CARTESIAN_POINT('Ctrl Pts',(-1.69979707754221,-1.,1.34367237124322));
#27742=CARTESIAN_POINT('Ctrl Pts',(-1.70614212266676,-1.,1.34459924533783));
#27743=CARTESIAN_POINT('Ctrl Pts',(-1.71250340687011,-1.,1.34549029589563));
#27744=CARTESIAN_POINT('Ctrl Pts',(-1.7188807715095,-1.,1.34634568653586));
#27745=CARTESIAN_POINT('Ctrl Pts',(-1.72527410681298,-1.,1.34716554820013));
#27746=CARTESIAN_POINT('Ctrl Pts',(-1.73040149654497,-1.,1.3477930915247));
#27747=CARTESIAN_POINT('Ctrl Pts',(-1.73425417886255,-1.,1.34824783113158));
#27748=CARTESIAN_POINT('Ctrl Pts',(-1.73682580585819,-1.,1.34854391898145));
#27749=CARTESIAN_POINT('Ctrl Pts',(-1.73811241238545,-1.,1.34869019493419));
#27750=CARTESIAN_POINT('',(-1.81978687191668,-1.,1.23627494547115));
#27751=CARTESIAN_POINT('',(-1.73811241238545,-1.,1.34869019493419));
#27752=CARTESIAN_POINT('',(-1.5055822144029,-1.,0.892032620296855));
#27753=CARTESIAN_POINT('Ctrl Pts',(-1.81978687191668,-1.,1.23627494547115));
#27754=CARTESIAN_POINT('Ctrl Pts',(-1.81925017193531,-1.,1.23509651170384));
#27755=CARTESIAN_POINT('Ctrl Pts',(-1.81817389920914,-1.,1.23274224526804));
#27756=CARTESIAN_POINT('Ctrl Pts',(-1.81655087183054,-1.,1.22921864890975));
#27757=CARTESIAN_POINT('Ctrl Pts',(-1.81436959209778,-1.,1.22453613304507));
#27758=CARTESIAN_POINT('Ctrl Pts',(-1.81161420806172,-1.,1.2187090610323));
#27759=CARTESIAN_POINT('Ctrl Pts',(-1.80882996916931,-1.,1.2129081570818));
#27760=CARTESIAN_POINT('Ctrl Pts',(-1.80601678480772,-1.,1.20713356605519));
#27761=CARTESIAN_POINT('Ctrl Pts',(-1.8031745483882,-1.,1.2013854893912));
#27762=CARTESIAN_POINT('Ctrl Pts',(-1.80030314370121,-1.,1.19566418930405));
#27763=CARTESIAN_POINT('Ctrl Pts',(-1.79740245923649,-1.,1.1899699793456));
#27764=CARTESIAN_POINT('Ctrl Pts',(-1.79447240321572,-1.,1.18430321697471));
#27765=CARTESIAN_POINT('Ctrl Pts',(-1.79151291552646,-1.,1.17866429440781));
#27766=CARTESIAN_POINT('Ctrl Pts',(-1.78852398877523,-1.,1.17305363177265));
#27767=CARTESIAN_POINT('Ctrl Pts',(-1.78550566040349,-1.,1.16747166312239));
#27768=CARTESIAN_POINT('Ctrl Pts',(-1.78245795880949,-1.,1.16191881298458));
#27769=CARTESIAN_POINT('Ctrl Pts',(-1.77938085564261,-1.,1.15639547194689));
#27770=CARTESIAN_POINT('Ctrl Pts',(-1.77627422557034,-1.,1.15090197841531));
#27771=CARTESIAN_POINT('Ctrl Pts',(-1.77313777896234,-1.,1.14543858226948));
#27772=CARTESIAN_POINT('Ctrl Pts',(-1.76997111386806,-1.,1.14000548337));
#27773=CARTESIAN_POINT('Ctrl Pts',(-1.76677384551883,-1.,1.13460291804635));
#27774=CARTESIAN_POINT('Ctrl Pts',(-1.76354571966171,-1.,1.12923123555076));
#27775=CARTESIAN_POINT('Ctrl Pts',(-1.76028671825084,-1.,1.12389096855078));
#27776=CARTESIAN_POINT('Ctrl Pts',(-1.75699720772089,-1.,1.11858293216752));
#27777=CARTESIAN_POINT('Ctrl Pts',(-1.75367772094617,-1.,1.11330807582542));
#27778=CARTESIAN_POINT('Ctrl Pts',(-1.75032866075914,-1.,1.10806728183003));
#27779=CARTESIAN_POINT('Ctrl Pts',(-1.74695004214924,-1.,1.10286118991144));
#27780=CARTESIAN_POINT('Ctrl Pts',(-1.74354119236212,-1.,1.09768999241229));
#27781=CARTESIAN_POINT('Ctrl Pts',(-1.74010053962252,-1.,1.09255329056496));
#27782=CARTESIAN_POINT('Ctrl Pts',(-1.73662628326093,-1.,1.08745056285429));
#27783=CARTESIAN_POINT('Ctrl Pts',(-1.73311705663407,-1.,1.08238162784749));
#27784=CARTESIAN_POINT('Ctrl Pts',(-1.72957248977424,-1.,1.0773470373727));
#27785=CARTESIAN_POINT('Ctrl Pts',(-1.72599406198489,-1.,1.07234866990252));
#27786=CARTESIAN_POINT('Ctrl Pts',(-1.72238500928456,-1.,1.06738966975463));
#27787=CARTESIAN_POINT('Ctrl Pts',(-1.71874858456908,-1.,1.0624732468065));
#27788=CARTESIAN_POINT('Ctrl Pts',(-1.71508654427022,-1.,1.05760163192481));
#27789=CARTESIAN_POINT('Ctrl Pts',(-1.71139783543986,-1.,1.05277517202854));
#27790=CARTESIAN_POINT('Ctrl Pts',(-1.70767646263641,-1.,1.0479908540499));
#27791=CARTESIAN_POINT('Ctrl Pts',(-1.70391338707969,-1.,1.04324363334546));
#27792=CARTESIAN_POINT('Ctrl Pts',(-1.70010052930951,-1.,1.03852922490782));
#27793=CARTESIAN_POINT('Ctrl Pts',(-1.69623414782769,-1.,1.03384646003587));
#27794=CARTESIAN_POINT('Ctrl Pts',(-1.69231840863471,-1.,1.02919977579155));
#27795=CARTESIAN_POINT('Ctrl Pts',(-1.68836910178475,-1.,1.02460180535272));
#27796=CARTESIAN_POINT('Ctrl Pts',(-1.68440578021739,-1.,1.02006795074222));
#27797=CARTESIAN_POINT('Ctrl Pts',(-1.6804428989482,-1.,1.01561026162787));
#27798=CARTESIAN_POINT('Ctrl Pts',(-1.67648246776457,-1.,1.01123236493507));
#27799=CARTESIAN_POINT('Ctrl Pts',(-1.67250335383248,-1.,1.00692206696387));
#27800=CARTESIAN_POINT('Ctrl Pts',(-1.66846059277231,-1.,1.00265091003682));
#27801=CARTESIAN_POINT('Ctrl Pts',(-1.66430758030304,-1.,0.998389654952317));
#27802=CARTESIAN_POINT('Ctrl Pts',(-1.66001553809916,-1.,0.994121836661116));
#27803=CARTESIAN_POINT('Ctrl Pts',(-1.65559044289746,-1.,0.98985562785445));
#27804=CARTESIAN_POINT('Ctrl Pts',(-1.6511001661277,-1.,0.985642622921626));
#27805=CARTESIAN_POINT('Ctrl Pts',(-1.64665139190834,-1.,0.981562530940574));
#27806=CARTESIAN_POINT('Ctrl Pts',(-1.64233990826831,-1.,0.977689794120297));
#27807=CARTESIAN_POINT('Ctrl Pts',(-1.63820952658157,-1.,0.974066058287501));
#27808=CARTESIAN_POINT('Ctrl Pts',(-1.63420665729609,-1.,0.970669715996356));
#27809=CARTESIAN_POINT('Ctrl Pts',(-1.63013849959083,-1.,0.967387853228041));
#27810=CARTESIAN_POINT('Ctrl Pts',(-1.6257193066974,-1.,0.964046107037821));
#27811=CARTESIAN_POINT('Ctrl Pts',(-1.62061638139929,-1.,0.960438326099958));
#27812=CARTESIAN_POINT('Ctrl Pts',(-1.61449324337233,-1.,0.956354422921573));
#27813=CARTESIAN_POINT('Ctrl Pts',(-1.60706069897794,-1.,0.951613284361248));
#27814=CARTESIAN_POINT('Ctrl Pts',(-1.59810042045408,-1.,0.946078063325796));
#27815=CARTESIAN_POINT('Ctrl Pts',(-1.58744937489796,-1.,0.939646377909319));
#27816=CARTESIAN_POINT('Ctrl Pts',(-1.57499388385561,-1.,0.932246680128849));
#27817=CARTESIAN_POINT('Ctrl Pts',(-1.56065988582509,-1.,0.923832188966322));
#27818=CARTESIAN_POINT('Ctrl Pts',(-1.54440491152808,-1.,0.91437591904658));
#27819=CARTESIAN_POINT('Ctrl Pts',(-1.52984849890434,-1.,0.905967409640499));
#27820=CARTESIAN_POINT('Ctrl Pts',(-1.51805569591479,-1.,0.89918504749193));
#27821=CARTESIAN_POINT('Ctrl Pts',(-1.50980486807181,-1.,0.894452006967538));
#27822=CARTESIAN_POINT('Ctrl Pts',(-1.5055822144029,-1.,0.892032620296855));
#27823=CARTESIAN_POINT('',(-1.60662857109684,-1.,0.693717979106305));
#27824=CARTESIAN_POINT('Origin',(0.,-1.,0.));
#27825=CARTESIAN_POINT('',(-2.0698113262342,-1.,0.7455743247944));
#27826=CARTESIAN_POINT('Ctrl Pts',(-1.60662857109684,-1.,0.693717979106305));
#27827=CARTESIAN_POINT('Ctrl Pts',(-1.61106790957619,-1.,0.69571209787897));
#27828=CARTESIAN_POINT('Ctrl Pts',(-1.61974673471117,-1.,0.699605146398837));
#27829=CARTESIAN_POINT('Ctrl Pts',(-1.6321654166204,-1.,0.705159151977294));
#27830=CARTESIAN_POINT('Ctrl Pts',(-1.64752408828442,-1.,0.711993139340447));
#27831=CARTESIAN_POINT('Ctrl Pts',(-1.66472880551777,-1.,0.71958543378795));
#27832=CARTESIAN_POINT('Ctrl Pts',(-1.67996158451922,-1.,0.726235967982445));
#27833=CARTESIAN_POINT('Ctrl Pts',(-1.69326921972915,-1.,0.731963238685357));
#27834=CARTESIAN_POINT('Ctrl Pts',(-1.70473309004249,-1.,0.736799665716932));
#27835=CARTESIAN_POINT('Ctrl Pts',(-1.71447789751001,-1.,0.74079516202821));
#27836=CARTESIAN_POINT('Ctrl Pts',(-1.72268229916769,-1.,0.744021445433093));
#27837=CARTESIAN_POINT('Ctrl Pts',(-1.72958533647714,-1.,0.746574710097752));
#27838=CARTESIAN_POINT('Ctrl Pts',(-1.7355035168033,-1.,0.74858246295687));
#27839=CARTESIAN_POINT('Ctrl Pts',(-1.74080458267114,-1.,0.750193435981249));
#27840=CARTESIAN_POINT('Ctrl Pts',(-1.74585086852502,-1.,0.751555614164482));
#27841=CARTESIAN_POINT('Ctrl Pts',(-1.75095139468794,-1.,0.752797683531314));
#27842=CARTESIAN_POINT('Ctrl Pts',(-1.75631083600019,-1.,0.754009254027829));
#27843=CARTESIAN_POINT('Ctrl Pts',(-1.76197817240128,-1.,0.755220979974461));
#27844=CARTESIAN_POINT('Ctrl Pts',(-1.76789396002998,-1.,0.75642189602781));
#27845=CARTESIAN_POINT('Ctrl Pts',(-1.77394167108292,-1.,0.757578264077029));
#27846=CARTESIAN_POINT('Ctrl Pts',(-1.77999411220945,-1.,0.758650626677518));
#27847=CARTESIAN_POINT('Ctrl Pts',(-1.78596964884604,-1.,0.759614401110189));
#27848=CARTESIAN_POINT('Ctrl Pts',(-1.7918581561088,-1.,0.760469555880749));
#27849=CARTESIAN_POINT('Ctrl Pts',(-1.79768986997783,-1.,0.761229695230558));
#27850=CARTESIAN_POINT('Ctrl Pts',(-1.80351583877342,-1.,0.761915336443547));
#27851=CARTESIAN_POINT('Ctrl Pts',(-1.80938551463965,-1.,0.762546129463938));
#27852=CARTESIAN_POINT('Ctrl Pts',(-1.8153211840553,-1.,0.763132003836634));
#27853=CARTESIAN_POINT('Ctrl Pts',(-1.82131873145266,-1.,0.763673465462726));
#27854=CARTESIAN_POINT('Ctrl Pts',(-1.82735991200065,-1.,0.764165902605995));
#27855=CARTESIAN_POINT('Ctrl Pts',(-1.83342077227142,-1.,0.764602549687853));
#27856=CARTESIAN_POINT('Ctrl Pts',(-1.83948181064835,-1.,0.764978057881737));
#27857=CARTESIAN_POINT('Ctrl Pts',(-1.84553698875924,-1.,0.765291664862029));
#27858=CARTESIAN_POINT('Ctrl Pts',(-1.85158945130063,-1.,0.765545710619062));
#27859=CARTESIAN_POINT('Ctrl Pts',(-1.85764741390394,-1.,0.765744212909318));
#27860=CARTESIAN_POINT('Ctrl Pts',(-1.86372027063312,-1.,0.765891519092547));
#27861=CARTESIAN_POINT('Ctrl Pts',(-1.86981398314341,-1.,0.765990708546091));
#27862=CARTESIAN_POINT('Ctrl Pts',(-1.87592888967883,-1.,0.766042837036744));
#27863=CARTESIAN_POINT('Ctrl Pts',(-1.88206215302561,-1.,0.766047794851864));
#27864=CARTESIAN_POINT('Ctrl Pts',(-1.88820926433409,-1.,0.766004837062091));
#27865=CARTESIAN_POINT('Ctrl Pts',(-1.89436577771388,-1.,0.765913193856978));
#27866=CARTESIAN_POINT('Ctrl Pts',(-1.90052930393596,-1.,0.765772772593386));
#27867=CARTESIAN_POINT('Ctrl Pts',(-1.90669961402356,-1.,0.765584196937919));
#27868=CARTESIAN_POINT('Ctrl Pts',(-1.91287765805169,-1.,0.765348465884722));
#27869=CARTESIAN_POINT('Ctrl Pts',(-1.91906491634196,-1.,0.765066729667088));
#27870=CARTESIAN_POINT('Ctrl Pts',(-1.92526263537048,-1.,0.764740025488211));
#27871=CARTESIAN_POINT('Ctrl Pts',(-1.93147105496382,-1.,0.76436901067394));
#27872=CARTESIAN_POINT('Ctrl Pts',(-1.93768964875886,-1.,0.763954049121458));
#27873=CARTESIAN_POINT('Ctrl Pts',(-1.9439174661764,-1.,0.763495333538629));
#27874=CARTESIAN_POINT('Ctrl Pts',(-1.95015342590024,-1.,0.762992990878769));
#27875=CARTESIAN_POINT('Ctrl Pts',(-1.95639665309869,-1.,0.762447203806179));
#27876=CARTESIAN_POINT('Ctrl Pts',(-1.96264672744186,-1.,0.761858300014423));
#27877=CARTESIAN_POINT('Ctrl Pts',(-1.96890351582499,-1.,0.76122669048382));
#27878=CARTESIAN_POINT('Ctrl Pts',(-1.97516705321494,-1.,0.760552825409757));
#27879=CARTESIAN_POINT('Ctrl Pts',(-1.98143741418172,-1.,0.75983714745219));
#27880=CARTESIAN_POINT('Ctrl Pts',(-1.98771456680874,-1.,0.759080037802488));
#27881=CARTESIAN_POINT('Ctrl Pts',(-1.99399831098817,-1.,0.758281796766761));
#27882=CARTESIAN_POINT('Ctrl Pts',(-2.00028834739178,-1.,0.757442676862724));
#27883=CARTESIAN_POINT('Ctrl Pts',(-2.0065843158773,-1.,0.75656290464667));
#27884=CARTESIAN_POINT('Ctrl Pts',(-2.01288584328084,-1.,0.755642704957865));
#27885=CARTESIAN_POINT('Ctrl Pts',(-2.01919259405809,-1.,0.754682330722816));
#27886=CARTESIAN_POINT('Ctrl Pts',(-2.02550428623313,-1.,0.753682061112768));
#27887=CARTESIAN_POINT('Ctrl Pts',(-2.03182068456221,-1.,0.752642180487211));
#27888=CARTESIAN_POINT('Ctrl Pts',(-2.03814160092099,-1.,0.751562963361115));
#27889=CARTESIAN_POINT('Ctrl Pts',(-2.04446689147979,-1.,0.750444657875576));
#27890=CARTESIAN_POINT('Ctrl Pts',(-2.05079645592154,-1.,0.749287468665046));
#27891=CARTESIAN_POINT('Ctrl Pts',(-2.05713023031006,-1.,0.748091554183802));
#27892=CARTESIAN_POINT('Ctrl Pts',(-2.06220058927826,-1.,0.747103932787919));
#27893=CARTESIAN_POINT('Ctrl Pts',(-2.06600523016815,-1.,0.7463458715442));
#27894=CARTESIAN_POINT('Ctrl Pts',(-2.06854248895728,-1.,0.745832791378367));
#27895=CARTESIAN_POINT('Ctrl Pts',(-2.0698113262342,-1.,0.7455743247944));
#27896=CARTESIAN_POINT('',(-2.11275013067528,-1.,0.61342227326009));
#27897=CARTESIAN_POINT('',(-2.0698113262342,-1.,0.7455743247944));
#27898=CARTESIAN_POINT('',(-1.7075470150345,-1.,0.383122945602004));
#27899=CARTESIAN_POINT('Ctrl Pts',(-2.11275013067528,-1.,0.61342227326009));
#27900=CARTESIAN_POINT('Ctrl Pts',(-2.11187554259986,-1.,0.6124673655618));
#27901=CARTESIAN_POINT('Ctrl Pts',(-2.11012443807238,-1.,0.610560911689899));
#27902=CARTESIAN_POINT('Ctrl Pts',(-2.1074919961518,-1.,0.607711315454876));
#27903=CARTESIAN_POINT('Ctrl Pts',(-2.10397049886949,-1.,0.60393203073603));
#27904=CARTESIAN_POINT('Ctrl Pts',(-2.0995493086477,-1.,0.599241616420533));
#27905=CARTESIAN_POINT('Ctrl Pts',(-2.0951087622027,-1.,0.594585006052162));
#27906=CARTESIAN_POINT('Ctrl Pts',(-2.09064881812129,-1.,0.589962365403406));
#27907=CARTESIAN_POINT('Ctrl Pts',(-2.08616943727951,-1.,0.585373918991617));
#27908=CARTESIAN_POINT('Ctrl Pts',(-2.08167059018418,-1.,0.580819952108063));
#27909=CARTESIAN_POINT('Ctrl Pts',(-2.07715226767559,-1.,0.576300797416844));
#27910=CARTESIAN_POINT('Ctrl Pts',(-2.07261449292824,-1.,0.571816823242603));
#27911=CARTESIAN_POINT('Ctrl Pts',(-2.06805732997334,-1.,0.567368421181087));
#27912=CARTESIAN_POINT('Ctrl Pts',(-2.06348090160589,-1.,0.562955993082261));
#27913=CARTESIAN_POINT('Ctrl Pts',(-2.05888537756462,-1.,0.558579940185151));
#27914=CARTESIAN_POINT('Ctrl Pts',(-2.05427091604413,-1.,0.554240657463906));
#27915=CARTESIAN_POINT('Ctrl Pts',(-2.04963761077958,-1.,0.549938525150295));
#27916=CARTESIAN_POINT('Ctrl Pts',(-2.04498544714588,-1.,0.54567390381743));
#27917=CARTESIAN_POINT('Ctrl Pts',(-2.04031422690527,-1.,0.541447120615659));
#27918=CARTESIAN_POINT('Ctrl Pts',(-2.03562362954037,-1.,0.537258489833262));
#27919=CARTESIAN_POINT('Ctrl Pts',(-2.03091336214426,-1.,0.533108355132976));
#27920=CARTESIAN_POINT('Ctrl Pts',(-2.0261832908329,-1.,0.528997127241914));
#27921=CARTESIAN_POINT('Ctrl Pts',(-2.02143356304698,-1.,0.524925318333476));
#27922=CARTESIAN_POINT('Ctrl Pts',(-2.01666477917286,-1.,0.52089359039937));
#27923=CARTESIAN_POINT('Ctrl Pts',(-2.01187773939242,-1.,0.516902681728687));
#27924=CARTESIAN_POINT('Ctrl Pts',(-2.00707309946949,-1.,0.512953306961792));
#27925=CARTESIAN_POINT('Ctrl Pts',(-2.00225107134734,-1.,0.509046069886157));
#27926=CARTESIAN_POINT('Ctrl Pts',(-1.99741107463572,-1.,0.505181361323026));
#27927=CARTESIAN_POINT('Ctrl Pts',(-1.99255149126155,-1.,0.501359287727146));
#27928=CARTESIAN_POINT('Ctrl Pts',(-1.98767044752932,-1.,0.497579909545574));
#27929=CARTESIAN_POINT('Ctrl Pts',(-1.98276658761821,-1.,0.493843476541494));
#27930=CARTESIAN_POINT('Ctrl Pts',(-1.97783973019229,-1.,0.490150627860952));
#27931=CARTESIAN_POINT('Ctrl Pts',(-1.97289186263272,-1.,0.486502692907659));
#27932=CARTESIAN_POINT('Ctrl Pts',(-1.96792703422362,-1.,0.48290166212069));
#27933=CARTESIAN_POINT('Ctrl Pts',(-1.96294933055943,-1.,0.479349583074855));
#27934=CARTESIAN_POINT('Ctrl Pts',(-1.95796111148177,-1.,0.475848034683176));
#27935=CARTESIAN_POINT('Ctrl Pts',(-1.95296148278133,-1.,0.472397672264072));
#27936=CARTESIAN_POINT('Ctrl Pts',(-1.94794381136514,-1.,0.468997482913135));
#27937=CARTESIAN_POINT('Ctrl Pts',(-1.9428979419619,-1.,0.46564546202603));
#27938=CARTESIAN_POINT('Ctrl Pts',(-1.93781486640821,-1.,0.462340031009056));
#27939=CARTESIAN_POINT('Ctrl Pts',(-1.93269066517934,-1.,0.459081234547926));
#27940=CARTESIAN_POINT('Ctrl Pts',(-1.92753067150476,-1.,0.455872005174371));
#27941=CARTESIAN_POINT('Ctrl Pts',(-1.92235380648502,-1.,0.452719478359432));
#27942=CARTESIAN_POINT('Ctrl Pts',(-1.91718342555755,-1.,0.449632260106662));
#27943=CARTESIAN_POINT('Ctrl Pts',(-1.9120369998112,-1.,0.446617343485711));
#27944=CARTESIAN_POINT('Ctrl Pts',(-1.90691756144898,-1.,0.44367755684915));
#27945=CARTESIAN_POINT('Ctrl Pts',(-1.90180124389086,-1.,0.440807833704038));
#27946=CARTESIAN_POINT('Ctrl Pts',(-1.89663648956466,-1.,0.437995003948244));
#27947=CARTESIAN_POINT('Ctrl Pts',(-1.89136993975504,-1.,0.435225660963383));
#27948=CARTESIAN_POINT('Ctrl Pts',(-1.88596913666793,-1.,0.432493038548748));
#27949=CARTESIAN_POINT('Ctrl Pts',(-1.88044229001832,-1.,0.429803062482344));
#27950=CARTESIAN_POINT('Ctrl Pts',(-1.87486989291484,-1.,0.427183828519102));
#27951=CARTESIAN_POINT('Ctrl Pts',(-1.86937803944323,-1.,0.424678177291359));
#27952=CARTESIAN_POINT('Ctrl Pts',(-1.86408083334028,-1.,0.422327307418275));
#27953=CARTESIAN_POINT('Ctrl Pts',(-1.85903281096686,-1.,0.420157287975619));
#27954=CARTESIAN_POINT('Ctrl Pts',(-1.85417632856234,-1.,0.418164129143534));
#27955=CARTESIAN_POINT('Ctrl Pts',(-1.84929312929882,-1.,0.416300022038864));
#27956=CARTESIAN_POINT('Ctrl Pts',(-1.8440575707371,-1.,0.41448743825434));
#27957=CARTESIAN_POINT('Ctrl Pts',(-1.83808953475839,-1.,0.412633125322161));
#27958=CARTESIAN_POINT('Ctrl Pts',(-1.83100408895216,-1.,0.410641256301675));
#27959=CARTESIAN_POINT('Ctrl Pts',(-1.8224702267854,-1.,0.408428948108533));
#27960=CARTESIAN_POINT('Ctrl Pts',(-1.81223801813988,-1.,0.405933518411838));
#27961=CARTESIAN_POINT('Ctrl Pts',(-1.80012077176221,-1.,0.403107976170441));
#27962=CARTESIAN_POINT('Ctrl Pts',(-1.78598826347533,-1.,0.39991940378308));
#27963=CARTESIAN_POINT('Ctrl Pts',(-1.7697556004756,-1.,0.39634619612042));
#27964=CARTESIAN_POINT('Ctrl Pts',(-1.75137405313962,-1.,0.392375812294307));
#27965=CARTESIAN_POINT('Ctrl Pts',(-1.7349317097561,-1.,0.388877023509191));
#27966=CARTESIAN_POINT('Ctrl Pts',(-1.72162022246158,-1.,0.38607079032701));
#27967=CARTESIAN_POINT('Ctrl Pts',(-1.71231062891958,-1.,0.384119047315542));
#27968=CARTESIAN_POINT('Ctrl Pts',(-1.7075470150345,-1.,0.383122945602004));
#27969=CARTESIAN_POINT('',(-1.74236521665491,-1.,0.163289472382896));
#27970=CARTESIAN_POINT('Origin',(0.,-1.,0.));
#27971=CARTESIAN_POINT('',(-2.19890268624765,-1.,0.069476445021958));
#27972=CARTESIAN_POINT('Ctrl Pts',(-1.74236521665491,-1.,0.163289472382896));
#27973=CARTESIAN_POINT('Ctrl Pts',(-1.7472034950333,-1.,0.163814161002002));
#27974=CARTESIAN_POINT('Ctrl Pts',(-1.75666056638427,-1.,0.164834765707158));
#27975=CARTESIAN_POINT('Ctrl Pts',(-1.77018771684844,-1.,0.1662793551464));
#27976=CARTESIAN_POINT('Ctrl Pts',(-1.7869064998507,-1.,0.168032772805197));
#27977=CARTESIAN_POINT('Ctrl Pts',(-1.80561530629706,-1.,0.169936923904608));
#27978=CARTESIAN_POINT('Ctrl Pts',(-1.82215766811545,-1.,0.171554770204119));
#27979=CARTESIAN_POINT('Ctrl Pts',(-1.83658380527692,-1.,0.1728894428919));
#27980=CARTESIAN_POINT('Ctrl Pts',(-1.8489811319852,-1.,0.173946627587731));
#27981=CARTESIAN_POINT('Ctrl Pts',(-1.85948367088837,-1.,0.17473525927603));
#27982=CARTESIAN_POINT('Ctrl Pts',(-1.86828349694799,-1.,0.175268337590758));
#27983=CARTESIAN_POINT('Ctrl Pts',(-1.87563767773588,-1.,0.175563480746485));
#27984=CARTESIAN_POINT('Ctrl Pts',(-1.88188663145367,-1.,0.175644148889698));
#27985=CARTESIAN_POINT('Ctrl Pts',(-1.88742606273259,-1.,0.175538155840648));
#27986=CARTESIAN_POINT('Ctrl Pts',(-1.892646301985,-1.,0.175274276190844));
#27987=CARTESIAN_POINT('Ctrl Pts',(-1.89788101117132,-1.,0.174879405091263));
#27988=CARTESIAN_POINT('Ctrl Pts',(-1.90335253862834,-1.,0.174375518661085));
#27989=CARTESIAN_POINT('Ctrl Pts',(-1.90911693975267,-1.,0.173776635257817));
#27990=CARTESIAN_POINT('Ctrl Pts',(-1.91511429159527,-1.,0.173090695383496));
#27991=CARTESIAN_POINT('Ctrl Pts',(-1.9212233439798,-1.,0.172321621259514));
#27992=CARTESIAN_POINT('Ctrl Pts',(-1.92731093582036,-1.,0.171471191532988));
#27993=CARTESIAN_POINT('Ctrl Pts',(-1.93329183155539,-1.,0.170541253116201));
#27994=CARTESIAN_POINT('Ctrl Pts',(-1.93915639211581,-1.,0.169534904817491));
#27995=CARTESIAN_POINT('Ctrl Pts',(-1.94493757756931,-1.,0.168455741607556));
#27996=CARTESIAN_POINT('Ctrl Pts',(-1.95069027794294,-1.,0.167307501784475));
#27997=CARTESIAN_POINT('Ctrl Pts',(-1.9564675971873,-1.,0.166093592002812));
#27998=CARTESIAN_POINT('Ctrl Pts',(-1.96229379940136,-1.,0.164816568920269));
#27999=CARTESIAN_POINT('Ctrl Pts',(-1.96816512677967,-1.,0.163478185457734));
#28000=CARTESIAN_POINT('Ctrl Pts',(-1.97406280235188,-1.,0.162079693556288));
#28001=CARTESIAN_POINT('Ctrl Pts',(-1.97996195437559,-1.,0.160622060784611));
#28002=CARTESIAN_POINT('Ctrl Pts',(-1.98584238283292,-1.,0.159106226437299));
#28003=CARTESIAN_POINT('Ctrl Pts',(-1.99169810931908,-1.,0.157533331459227));
#28004=CARTESIAN_POINT('Ctrl Pts',(-1.99753284771497,-1.,0.155904629548783));
#28005=CARTESIAN_POINT('Ctrl Pts',(-2.00335565310543,-1.,0.154221403049722));
#28006=CARTESIAN_POINT('Ctrl Pts',(-2.00917680318424,-1.,0.15248488362145));
#28007=CARTESIAN_POINT('Ctrl Pts',(-2.01500291940238,-1.,0.150696157673078));
#28008=CARTESIAN_POINT('Ctrl Pts',(-2.02083464969894,-1.,0.148856124775337));
#28009=CARTESIAN_POINT('Ctrl Pts',(-2.02666926182017,-1.,0.146965557332583));
#28010=CARTESIAN_POINT('Ctrl Pts',(-2.03250223739942,-1.,0.145025140186057));
#28011=CARTESIAN_POINT('Ctrl Pts',(-2.03832911025912,-1.,0.143035515058209));
#28012=CARTESIAN_POINT('Ctrl Pts',(-2.04414757947916,-1.,0.140997332152546));
#28013=CARTESIAN_POINT('Ctrl Pts',(-2.04995762001328,-1.,0.138911255368966));
#28014=CARTESIAN_POINT('Ctrl Pts',(-2.05576044414264,-1.,0.136777941218043));
#28015=CARTESIAN_POINT('Ctrl Pts',(-2.06155781517842,-1.,0.134598026192106));
#28016=CARTESIAN_POINT('Ctrl Pts',(-2.06735123910326,-1.,0.13237211154771));
#28017=CARTESIAN_POINT('Ctrl Pts',(-2.07314114713063,-1.,0.130100748328403));
#28018=CARTESIAN_POINT('Ctrl Pts',(-2.07892715110987,-1.,0.12778444527612));
#28019=CARTESIAN_POINT('Ctrl Pts',(-2.08470840653643,-1.,0.125423679412061));
#28020=CARTESIAN_POINT('Ctrl Pts',(-2.09048392424825,-1.,0.123018905621083));
#28021=CARTESIAN_POINT('Ctrl Pts',(-2.0962529286773,-1.,0.120570567965122));
#28022=CARTESIAN_POINT('Ctrl Pts',(-2.102015121329,-1.,0.118079107988355));
#28023=CARTESIAN_POINT('Ctrl Pts',(-2.10777050261309,-1.,0.115544957687926));
#28024=CARTESIAN_POINT('Ctrl Pts',(-2.11351924490306,-1.,0.112968534419737));
#28025=CARTESIAN_POINT('Ctrl Pts',(-2.11926155590865,-1.,0.110350236135025));
#28026=CARTESIAN_POINT('Ctrl Pts',(-2.12499752307,-1.,0.10769043523109));
#28027=CARTESIAN_POINT('Ctrl Pts',(-2.13072704887293,-1.,0.104989479152739));
#28028=CARTESIAN_POINT('Ctrl Pts',(-2.13644992667165,-1.,0.1022477005561));
#28029=CARTESIAN_POINT('Ctrl Pts',(-2.14216588396025,-1.,0.0994654261990914));
#28030=CARTESIAN_POINT('Ctrl Pts',(-2.14787463531795,-1.,0.0966429852305457));
#28031=CARTESIAN_POINT('Ctrl Pts',(-2.1535759397817,-1.,0.0937807218867642));
#28032=CARTESIAN_POINT('Ctrl Pts',(-2.15926961544516,-1.,0.0908789888107264));
#28033=CARTESIAN_POINT('Ctrl Pts',(-2.16495552645014,-1.,0.0879381291386921));
#28034=CARTESIAN_POINT('Ctrl Pts',(-2.17063357870952,-1.,0.0849584620835371));
#28035=CARTESIAN_POINT('Ctrl Pts',(-2.176303712113,-1.,0.0819402680872764));
#28036=CARTESIAN_POINT('Ctrl Pts',(-2.18196589448887,-1.,0.0788837727685241));
#28037=CARTESIAN_POINT('Ctrl Pts',(-2.1876201139953,-1.,0.0757891465836146));
#28038=CARTESIAN_POINT('Ctrl Pts',(-2.19213712013662,-1.,0.0732830357306724));
#28039=CARTESIAN_POINT('Ctrl Pts',(-2.19552129484002,-1.,0.0713863779526153));
#28040=CARTESIAN_POINT('Ctrl Pts',(-2.19777582085423,-1.,0.0701143536325489));
#28041=CARTESIAN_POINT('Ctrl Pts',(-2.19890268624765,-1.,0.069476445021958));
#28042=CARTESIAN_POINT('',(-2.19890268624765,-1.,-0.0694764450219585));
#28043=CARTESIAN_POINT('',(-2.19890268624765,-1.,0.069476445021958));
#28044=CARTESIAN_POINT('',(-1.74236521665491,-1.,-0.163289472382896));
#28045=CARTESIAN_POINT('Ctrl Pts',(-2.19890268624765,-1.,-0.0694764450219585));
#28046=CARTESIAN_POINT('Ctrl Pts',(-2.19777582085261,-1.,-0.0701143536324927));
#28047=CARTESIAN_POINT('Ctrl Pts',(-2.19552129483562,-1.,-0.0713863779524629));
#28048=CARTESIAN_POINT('Ctrl Pts',(-2.19213712012956,-1.,-0.0732830357304277));
#28049=CARTESIAN_POINT('Ctrl Pts',(-2.1876201139874,-1.,-0.0757891465833413));
#28050=CARTESIAN_POINT('Ctrl Pts',(-2.18196589448304,-1.,-0.0788837727683229));
#28051=CARTESIAN_POINT('Ctrl Pts',(-2.1763037121106,-1.,-0.0819402680871941));
#28052=CARTESIAN_POINT('Ctrl Pts',(-2.17063357871031,-1.,-0.0849584620835644));
#28053=CARTESIAN_POINT('Ctrl Pts',(-2.16495552645275,-1.,-0.0879381291387824));
#28054=CARTESIAN_POINT('Ctrl Pts',(-2.15926961544808,-1.,-0.0908789888108267));
#28055=CARTESIAN_POINT('Ctrl Pts',(-2.15357593978377,-1.,-0.0937807218868346));
#28056=CARTESIAN_POINT('Ctrl Pts',(-2.14787463531864,-1.,-0.096642985230569));
#28057=CARTESIAN_POINT('Ctrl Pts',(-2.14216588395974,-1.,-0.0994654261990744));
#28058=CARTESIAN_POINT('Ctrl Pts',(-2.13644992667052,-1.,-0.102247700556064));
#28059=CARTESIAN_POINT('Ctrl Pts',(-2.1307270488718,-1.,-0.104989479152703));
#28060=CARTESIAN_POINT('Ctrl Pts',(-2.12499752306927,-1.,-0.107690435231068));
#28061=CARTESIAN_POINT('Ctrl Pts',(-2.11926155590849,-1.,-0.11035023613502));
#28062=CARTESIAN_POINT('Ctrl Pts',(-2.11351924490335,-1.,-0.112968534419746));
#28063=CARTESIAN_POINT('Ctrl Pts',(-2.10777050261359,-1.,-0.11554495768794));
#28064=CARTESIAN_POINT('Ctrl Pts',(-2.10201512132945,-1.,-0.118079107988368));
#28065=CARTESIAN_POINT('Ctrl Pts',(-2.09625292867756,-1.,-0.120570567965129));
#28066=CARTESIAN_POINT('Ctrl Pts',(-2.09048392424826,-1.,-0.123018905621083));
#28067=CARTESIAN_POINT('Ctrl Pts',(-2.08470840653628,-1.,-0.125423679412058));
#28068=CARTESIAN_POINT('Ctrl Pts',(-2.07892715110967,-1.,-0.127784445276116));
#28069=CARTESIAN_POINT('Ctrl Pts',(-2.07314114713047,-1.,-0.130100748328401));
#28070=CARTESIAN_POINT('Ctrl Pts',(-2.06735123910319,-1.,-0.13237211154771));
#28071=CARTESIAN_POINT('Ctrl Pts',(-2.06155781517844,-1.,-0.134598026192107));
#28072=CARTESIAN_POINT('Ctrl Pts',(-2.0557604441427,-1.,-0.136777941218044));
#28073=CARTESIAN_POINT('Ctrl Pts',(-2.04995762001333,-1.,-0.138911255368966));
#28074=CARTESIAN_POINT('Ctrl Pts',(-2.04414757947919,-1.,-0.140997332152545));
#28075=CARTESIAN_POINT('Ctrl Pts',(-2.03832911025913,-1.,-0.143035515058208));
#28076=CARTESIAN_POINT('Ctrl Pts',(-2.03250223739941,-1.,-0.145025140186058));
#28077=CARTESIAN_POINT('Ctrl Pts',(-2.02666926182017,-1.,-0.146965557332586));
#28078=CARTESIAN_POINT('Ctrl Pts',(-2.02083464969897,-1.,-0.148856124775343));
#28079=CARTESIAN_POINT('Ctrl Pts',(-2.01500291940243,-1.,-0.150696157673084));
#28080=CARTESIAN_POINT('Ctrl Pts',(-2.00917680318426,-1.,-0.152484883621452));
#28081=CARTESIAN_POINT('Ctrl Pts',(-2.00335565310539,-1.,-0.154221403049719));
#28082=CARTESIAN_POINT('Ctrl Pts',(-1.99753284771487,-1.,-0.155904629548775));
#28083=CARTESIAN_POINT('Ctrl Pts',(-1.99169810931893,-1.,-0.157533331459215));
#28084=CARTESIAN_POINT('Ctrl Pts',(-1.98584238283279,-1.,-0.159106226437289));
#28085=CARTESIAN_POINT('Ctrl Pts',(-1.97996195437557,-1.,-0.16062206078461));
#28086=CARTESIAN_POINT('Ctrl Pts',(-1.97406280235204,-1.,-0.162079693556302));
#28087=CARTESIAN_POINT('Ctrl Pts',(-1.96816512678,-1.,-0.16347818545776));
#28088=CARTESIAN_POINT('Ctrl Pts',(-1.96229379940174,-1.,-0.1648165689203));
#28089=CARTESIAN_POINT('Ctrl Pts',(-1.95646759718755,-1.,-0.166093592002833));
#28090=CARTESIAN_POINT('Ctrl Pts',(-1.95069027794286,-1.,-0.167307501784469));
#28091=CARTESIAN_POINT('Ctrl Pts',(-1.94493757756879,-1.,-0.168455741607516));
#28092=CARTESIAN_POINT('Ctrl Pts',(-1.93915639211497,-1.,-0.169534904817425));
#28093=CARTESIAN_POINT('Ctrl Pts',(-1.93329183155455,-1.,-0.170541253116136));
#28094=CARTESIAN_POINT('Ctrl Pts',(-1.92731093582,-1.,-0.17147119153296));
#28095=CARTESIAN_POINT('Ctrl Pts',(-1.92122334398034,-1.,-0.172321621259557));
#28096=CARTESIAN_POINT('Ctrl Pts',(-1.91511429159681,-1.,-0.173090695383619));
#28097=CARTESIAN_POINT('Ctrl Pts',(-1.90911693975475,-1.,-0.173776635257984));
#28098=CARTESIAN_POINT('Ctrl Pts',(-1.90335253863003,-1.,-0.174375518661222));
#28099=CARTESIAN_POINT('Ctrl Pts',(-1.89788101117148,-1.,-0.174879405091277));
#28100=CARTESIAN_POINT('Ctrl Pts',(-1.89264630198279,-1.,-0.175274276190664));
#28101=CARTESIAN_POINT('Ctrl Pts',(-1.88742606272818,-1.,-0.175538155840286));
#28102=CARTESIAN_POINT('Ctrl Pts',(-1.88188663144846,-1.,-0.175644148889271));
#28103=CARTESIAN_POINT('Ctrl Pts',(-1.87563767773249,-1.,-0.175563480746205));
#28104=CARTESIAN_POINT('Ctrl Pts',(-1.86828349694972,-1.,-0.175268337590901));
#28105=CARTESIAN_POINT('Ctrl Pts',(-1.85948367089838,-1.,-0.174735259276856));
#28106=CARTESIAN_POINT('Ctrl Pts',(-1.84898113200543,-1.,-0.173946627589401));
#28107=CARTESIAN_POINT('Ctrl Pts',(-1.83658380530747,-1.,-0.17288944289442));
#28108=CARTESIAN_POINT('Ctrl Pts',(-1.82215766815414,-1.,-0.171554770207306));
#28109=CARTESIAN_POINT('Ctrl Pts',(-1.80561530633924,-1.,-0.169936923908078));
#28110=CARTESIAN_POINT('Ctrl Pts',(-1.78690649988931,-1.,-0.16803277280837));
#28111=CARTESIAN_POINT('Ctrl Pts',(-1.77018771687692,-1.,-0.166279355148738));
#28112=CARTESIAN_POINT('Ctrl Pts',(-1.75666056640041,-1.,-0.164834765708484));
#28113=CARTESIAN_POINT('Ctrl Pts',(-1.74720349503904,-1.,-0.163814161002474));
#28114=CARTESIAN_POINT('Ctrl Pts',(-1.74236521665491,-1.,-0.163289472382896));
#28115=CARTESIAN_POINT('',(-1.7075470150345,-1.,-0.383122945602004));
#28116=CARTESIAN_POINT('Origin',(0.,-1.,0.));
#28117=CARTESIAN_POINT('',(-2.11275013067528,-1.,-0.61342227326009));
#28118=CARTESIAN_POINT('Ctrl Pts',(-1.7075470150345,-1.,-0.383122945602004));
#28119=CARTESIAN_POINT('Ctrl Pts',(-1.71231062891398,-1.,-0.384119047314215));
#28120=CARTESIAN_POINT('Ctrl Pts',(-1.72162022244582,-1.,-0.386070790323281));
#28121=CARTESIAN_POINT('Ctrl Pts',(-1.73493170972829,-1.,-0.388877023502615));
#28122=CARTESIAN_POINT('Ctrl Pts',(-1.75137405310193,-1.,-0.392375812285395));
#28123=CARTESIAN_POINT('Ctrl Pts',(-1.76975560043442,-1.,-0.396346196110688));
#28124=CARTESIAN_POINT('Ctrl Pts',(-1.78598826343754,-1.,-0.399919403774155));
#28125=CARTESIAN_POINT('Ctrl Pts',(-1.80012077173238,-1.,-0.403107976163396));
#28126=CARTESIAN_POINT('Ctrl Pts',(-1.81223801812013,-1.,-0.405933518407175));
#28127=CARTESIAN_POINT('Ctrl Pts',(-1.82247022677562,-1.,-0.408428948106227));
#28128=CARTESIAN_POINT('Ctrl Pts',(-1.83100408895047,-1.,-0.410641256301276));
#28129=CARTESIAN_POINT('Ctrl Pts',(-1.8380895347617,-1.,-0.412633125322945));
#28130=CARTESIAN_POINT('Ctrl Pts',(-1.84405757074218,-1.,-0.414487438255542));
#28131=CARTESIAN_POINT('Ctrl Pts',(-1.84929312930314,-1.,-0.416300022039885));
#28132=CARTESIAN_POINT('Ctrl Pts',(-1.8541763285645,-1.,-0.418164129144045));
#28133=CARTESIAN_POINT('Ctrl Pts',(-1.8590328109667,-1.,-0.420157287975583));
#28134=CARTESIAN_POINT('Ctrl Pts',(-1.86408083333863,-1.,-0.422327307417884));
#28135=CARTESIAN_POINT('Ctrl Pts',(-1.8693780394412,-1.,-0.424678177290876));
#28136=CARTESIAN_POINT('Ctrl Pts',(-1.87486989291333,-1.,-0.427183828518743));
#28137=CARTESIAN_POINT('Ctrl Pts',(-1.88044229001778,-1.,-0.429803062482217));
#28138=CARTESIAN_POINT('Ctrl Pts',(-1.88596913666828,-1.,-0.432493038548833));
#28139=CARTESIAN_POINT('Ctrl Pts',(-1.89136993975585,-1.,-0.43522566096358));
#28140=CARTESIAN_POINT('Ctrl Pts',(-1.89663648956549,-1.,-0.437995003948443));
#28141=CARTESIAN_POINT('Ctrl Pts',(-1.90180124389137,-1.,-0.44080783370416));
#28142=CARTESIAN_POINT('Ctrl Pts',(-1.90691756144906,-1.,-0.44367755684917));
#28143=CARTESIAN_POINT('Ctrl Pts',(-1.91203699981095,-1.,-0.446617343485651));
#28144=CARTESIAN_POINT('Ctrl Pts',(-1.91718342555717,-1.,-0.449632260106572));
#28145=CARTESIAN_POINT('Ctrl Pts',(-1.9223538064847,-1.,-0.452719478359356));
#28146=CARTESIAN_POINT('Ctrl Pts',(-1.92753067150461,-1.,-0.455872005174335));
#28147=CARTESIAN_POINT('Ctrl Pts',(-1.93269066517936,-1.,-0.459081234547931));
#28148=CARTESIAN_POINT('Ctrl Pts',(-1.93781486640834,-1.,-0.462340031009087));
#28149=CARTESIAN_POINT('Ctrl Pts',(-1.94289794196205,-1.,-0.465645462026064));
#28150=CARTESIAN_POINT('Ctrl Pts',(-1.94794381136524,-1.,-0.468997482913158));
#28151=CARTESIAN_POINT('Ctrl Pts',(-1.95296148278136,-1.,-0.472397672264079));
#28152=CARTESIAN_POINT('Ctrl Pts',(-1.95796111148175,-1.,-0.475848034683171));
#28153=CARTESIAN_POINT('Ctrl Pts',(-1.96294933055938,-1.,-0.479349583074846));
#28154=CARTESIAN_POINT('Ctrl Pts',(-1.96792703422358,-1.,-0.482901662120686));
#28155=CARTESIAN_POINT('Ctrl Pts',(-1.97289186263272,-1.,-0.486502692907661));
#28156=CARTESIAN_POINT('Ctrl Pts',(-1.97783973019229,-1.,-0.490150627860955));
#28157=CARTESIAN_POINT('Ctrl Pts',(-1.9827665876182,-1.,-0.493843476541492));
#28158=CARTESIAN_POINT('Ctrl Pts',(-1.98767044752929,-1.,-0.497579909545564));
#28159=CARTESIAN_POINT('Ctrl Pts',(-1.9925514912615,-1.,-0.501359287727129));
#28160=CARTESIAN_POINT('Ctrl Pts',(-1.99741107463567,-1.,-0.505181361323011));
#28161=CARTESIAN_POINT('Ctrl Pts',(-2.00225107134733,-1.,-0.509046069886152));
#28162=CARTESIAN_POINT('Ctrl Pts',(-2.00707309946955,-1.,-0.512953306961813));
#28163=CARTESIAN_POINT('Ctrl Pts',(-2.01187773939257,-1.,-0.516902681728733));
#28164=CARTESIAN_POINT('Ctrl Pts',(-2.01666477917305,-1.,-0.520893590399428));
#28165=CARTESIAN_POINT('Ctrl Pts',(-2.02143356304712,-1.,-0.524925318333518));
#28166=CARTESIAN_POINT('Ctrl Pts',(-2.02618329083289,-1.,-0.52899712724191));
#28167=CARTESIAN_POINT('Ctrl Pts',(-2.03091336214401,-1.,-0.533108355132905));
#28168=CARTESIAN_POINT('Ctrl Pts',(-2.03562362953993,-1.,-0.537258489833134));
#28169=CARTESIAN_POINT('Ctrl Pts',(-2.0403142269048,-1.,-0.54144712061552));
#28170=CARTESIAN_POINT('Ctrl Pts',(-2.0449854471456,-1.,-0.545673903817348));
#28171=CARTESIAN_POINT('Ctrl Pts',(-2.04963761077974,-1.,-0.549938525150342));
#28172=CARTESIAN_POINT('Ctrl Pts',(-2.05427091604482,-1.,-0.554240657464109));
#28173=CARTESIAN_POINT('Ctrl Pts',(-2.05888537756571,-1.,-0.558579940185467));
#28174=CARTESIAN_POINT('Ctrl Pts',(-2.06348090160697,-1.,-0.562955993082574));
#28175=CARTESIAN_POINT('Ctrl Pts',(-2.06805732997383,-1.,-0.567368421181229));
#28176=CARTESIAN_POINT('Ctrl Pts',(-2.07261449292757,-1.,-0.571816823242411));
#28177=CARTESIAN_POINT('Ctrl Pts',(-2.07715226767361,-1.,-0.576300797416274));
#28178=CARTESIAN_POINT('Ctrl Pts',(-2.08167059018138,-1.,-0.580819952107257));
#28179=CARTESIAN_POINT('Ctrl Pts',(-2.086169437277,-1.,-0.585373918990895));
#28180=CARTESIAN_POINT('Ctrl Pts',(-2.09064881812053,-1.,-0.589962365403189));
#28181=CARTESIAN_POINT('Ctrl Pts',(-2.09510876220501,-1.,-0.594585006052823));
#28182=CARTESIAN_POINT('Ctrl Pts',(-2.09954930865331,-1.,-0.599241616422144));
#28183=CARTESIAN_POINT('Ctrl Pts',(-2.10397049887709,-1.,-0.603932030738212));
#28184=CARTESIAN_POINT('Ctrl Pts',(-2.10749199615859,-1.,-0.607711315456826));
#28185=CARTESIAN_POINT('Ctrl Pts',(-2.11012443807661,-1.,-0.610560911691113));
#28186=CARTESIAN_POINT('Ctrl Pts',(-2.11187554260142,-1.,-0.61246736556225));
#28187=CARTESIAN_POINT('Ctrl Pts',(-2.11275013067528,-1.,-0.61342227326009));
#28188=CARTESIAN_POINT('',(-2.0698113262342,-1.,-0.745574324794401));
#28189=CARTESIAN_POINT('',(-2.11275013067528,-1.,-0.61342227326009));
#28190=CARTESIAN_POINT('',(-1.60662857109684,-1.,-0.693717979106306));
#28191=CARTESIAN_POINT('Ctrl Pts',(-2.0698113262342,-1.,-0.745574324794401));
#28192=CARTESIAN_POINT('Ctrl Pts',(-2.06854248895575,-1.,-0.74583279137781));
#28193=CARTESIAN_POINT('Ctrl Pts',(-2.06600523016401,-1.,-0.746345871542695));
#28194=CARTESIAN_POINT('Ctrl Pts',(-2.06220058927162,-1.,-0.747103932785504));
#28195=CARTESIAN_POINT('Ctrl Pts',(-2.05713023030263,-1.,-0.748091554181101));
#28196=CARTESIAN_POINT('Ctrl Pts',(-2.05079645591606,-1.,-0.749287468663053));
#28197=CARTESIAN_POINT('Ctrl Pts',(-2.04446689147754,-1.,-0.750444657874758));
#28198=CARTESIAN_POINT('Ctrl Pts',(-2.03814160092173,-1.,-0.751562963361383));
#28199=CARTESIAN_POINT('Ctrl Pts',(-2.03182068456467,-1.,-0.752642180488104));
#28200=CARTESIAN_POINT('Ctrl Pts',(-2.02550428623587,-1.,-0.753682061113765));
#28201=CARTESIAN_POINT('Ctrl Pts',(-2.01919259406003,-1.,-0.75468233072352));
#28202=CARTESIAN_POINT('Ctrl Pts',(-2.01288584328149,-1.,-0.7556427049581));
#28203=CARTESIAN_POINT('Ctrl Pts',(-2.00658431587682,-1.,-0.756562904646496));
#28204=CARTESIAN_POINT('Ctrl Pts',(-2.00028834739072,-1.,-0.757442676862341));
#28205=CARTESIAN_POINT('Ctrl Pts',(-1.9939983109871,-1.,-0.758281796766377));
#28206=CARTESIAN_POINT('Ctrl Pts',(-1.98771456680806,-1.,-0.759080037802242));
#28207=CARTESIAN_POINT('Ctrl Pts',(-1.98143741418156,-1.,-0.759837147452135));
#28208=CARTESIAN_POINT('Ctrl Pts',(-1.97516705321521,-1.,-0.760552825409855));
#28209=CARTESIAN_POINT('Ctrl Pts',(-1.96890351582545,-1.,-0.761226690483986));
#28210=CARTESIAN_POINT('Ctrl Pts',(-1.96264672744229,-1.,-0.761858300014575));
#28211=CARTESIAN_POINT('Ctrl Pts',(-1.95639665309893,-1.,-0.762447203806263));
#28212=CARTESIAN_POINT('Ctrl Pts',(-1.95015342590025,-1.,-0.762992990878774));
#28213=CARTESIAN_POINT('Ctrl Pts',(-1.94391746617626,-1.,-0.76349533353858));
#28214=CARTESIAN_POINT('Ctrl Pts',(-1.93768964875867,-1.,-0.763954049121393));
#28215=CARTESIAN_POINT('Ctrl Pts',(-1.93147105496367,-1.,-0.764369010673889));
#28216=CARTESIAN_POINT('Ctrl Pts',(-1.92526263537041,-1.,-0.764740025488189));
#28217=CARTESIAN_POINT('Ctrl Pts',(-1.91906491634197,-1.,-0.765066729667095));
#28218=CARTESIAN_POINT('Ctrl Pts',(-1.91287765805174,-1.,-0.765348465884739));
#28219=CARTESIAN_POINT('Ctrl Pts',(-1.90669961402362,-1.,-0.765584196937936));
#28220=CARTESIAN_POINT('Ctrl Pts',(-1.90052930393599,-1.,-0.765772772593395));
#28221=CARTESIAN_POINT('Ctrl Pts',(-1.89436577771389,-1.,-0.765913193856979));
#28222=CARTESIAN_POINT('Ctrl Pts',(-1.88820926433409,-1.,-0.76600483706209));
#28223=CARTESIAN_POINT('Ctrl Pts',(-1.88206215302561,-1.,-0.766047794851868));
#28224=CARTESIAN_POINT('Ctrl Pts',(-1.87592888967886,-1.,-0.766042837036759));
#28225=CARTESIAN_POINT('Ctrl Pts',(-1.86981398314345,-1.,-0.765990708546111));
#28226=CARTESIAN_POINT('Ctrl Pts',(-1.86372027063314,-1.,-0.765891519092557));
#28227=CARTESIAN_POINT('Ctrl Pts',(-1.85764741390391,-1.,-0.765744212909305));
#28228=CARTESIAN_POINT('Ctrl Pts',(-1.85158945130054,-1.,-0.765545710619023));
#28229=CARTESIAN_POINT('Ctrl Pts',(-1.8455369887591,-1.,-0.765291664861971));
#28230=CARTESIAN_POINT('Ctrl Pts',(-1.83948181064823,-1.,-0.764978057881687));
#28231=CARTESIAN_POINT('Ctrl Pts',(-1.8334207722714,-1.,-0.764602549687845));
#28232=CARTESIAN_POINT('Ctrl Pts',(-1.8273599120008,-1.,-0.764165902606055));
#28233=CARTESIAN_POINT('Ctrl Pts',(-1.82131873145297,-1.,-0.763673465462854));
#28234=CARTESIAN_POINT('Ctrl Pts',(-1.81532118405566,-1.,-0.763132003836783));
#28235=CARTESIAN_POINT('Ctrl Pts',(-1.80938551463989,-1.,-0.762546129464036));
#28236=CARTESIAN_POINT('Ctrl Pts',(-1.80351583877334,-1.,-0.761915336443515));
#28237=CARTESIAN_POINT('Ctrl Pts',(-1.79768986997735,-1.,-0.761229695230359));
#28238=CARTESIAN_POINT('Ctrl Pts',(-1.79185815610802,-1.,-0.760469555880425));
#28239=CARTESIAN_POINT('Ctrl Pts',(-1.78596964884526,-1.,-0.759614401109868));
#28240=CARTESIAN_POINT('Ctrl Pts',(-1.77999411220912,-1.,-0.75865062667738));
#28241=CARTESIAN_POINT('Ctrl Pts',(-1.77394167108342,-1.,-0.757578264077238));
#28242=CARTESIAN_POINT('Ctrl Pts',(-1.76789396003141,-1.,-0.756421896028403));
#28243=CARTESIAN_POINT('Ctrl Pts',(-1.7619781724032,-1.,-0.755220979975262));
#28244=CARTESIAN_POINT('Ctrl Pts',(-1.75631083600175,-1.,-0.75400925402848));
#28245=CARTESIAN_POINT('Ctrl Pts',(-1.75095139468809,-1.,-0.752797683531377));
#28246=CARTESIAN_POINT('Ctrl Pts',(-1.74585086852298,-1.,-0.751555614163629));
#28247=CARTESIAN_POINT('Ctrl Pts',(-1.74080458266705,-1.,-0.75019343597954));
#28248=CARTESIAN_POINT('Ctrl Pts',(-1.73550351679848,-1.,-0.748582462954854));
#28249=CARTESIAN_POINT('Ctrl Pts',(-1.72958533647399,-1.,-0.746574710096436));
#28250=CARTESIAN_POINT('Ctrl Pts',(-1.7226822991693,-1.,-0.744021445433764));
#28251=CARTESIAN_POINT('Ctrl Pts',(-1.71447789751927,-1.,-0.740795162032087));
#28252=CARTESIAN_POINT('Ctrl Pts',(-1.70473309006121,-1.,-0.736799665724771));
#28253=CARTESIAN_POINT('Ctrl Pts',(-1.69326921975743,-1.,-0.731963238697195));
#28254=CARTESIAN_POINT('Ctrl Pts',(-1.67996158455503,-1.,-0.726235967997433));
#28255=CARTESIAN_POINT('Ctrl Pts',(-1.6647288055568,-1.,-0.719585433804282));
#28256=CARTESIAN_POINT('Ctrl Pts',(-1.64752408832016,-1.,-0.711993139355394));
#28257=CARTESIAN_POINT('Ctrl Pts',(-1.63216541664676,-1.,-0.705159151988319));
#28258=CARTESIAN_POINT('Ctrl Pts',(-1.61974673472612,-1.,-0.699605146405088));
#28259=CARTESIAN_POINT('Ctrl Pts',(-1.61106790958151,-1.,-0.695712097881194));
#28260=CARTESIAN_POINT('Ctrl Pts',(-1.60662857109684,-1.,-0.693717979106306));
#28261=CARTESIAN_POINT('',(-1.5055822144029,-1.,-0.892032620296855));
#28262=CARTESIAN_POINT('Origin',(0.,-1.,0.));
#28263=CARTESIAN_POINT('',(-1.81978687191668,-1.,-1.23627494547115));
#28264=CARTESIAN_POINT('Ctrl Pts',(-1.5055822144029,-1.,-0.892032620296855));
#28265=CARTESIAN_POINT('Ctrl Pts',(-1.50980486806688,-1.,-0.894452006964543));
#28266=CARTESIAN_POINT('Ctrl Pts',(-1.51805569590094,-1.,-0.899185047483511));
#28267=CARTESIAN_POINT('Ctrl Pts',(-1.52984849887993,-1.,-0.905967409625651));
#28268=CARTESIAN_POINT('Ctrl Pts',(-1.54440491149498,-1.,-0.914375919026456));
#28269=CARTESIAN_POINT('Ctrl Pts',(-1.56065988578893,-1.,-0.923832188944341));
#28270=CARTESIAN_POINT('Ctrl Pts',(-1.57499388382243,-1.,-0.932246680108685));
#28271=CARTESIAN_POINT('Ctrl Pts',(-1.58744937487176,-1.,-0.939646377893399));
#28272=CARTESIAN_POINT('Ctrl Pts',(-1.59810042043673,-1.,-0.946078063315257));
#28273=CARTESIAN_POINT('Ctrl Pts',(-1.60706069896936,-1.,-0.951613284356035));
#28274=CARTESIAN_POINT('Ctrl Pts',(-1.61449324337085,-1.,-0.956354422920671));
#28275=CARTESIAN_POINT('Ctrl Pts',(-1.62061638140221,-1.,-0.960438326101729));
#28276=CARTESIAN_POINT('Ctrl Pts',(-1.62571930670187,-1.,-0.964046107040536));
#28277=CARTESIAN_POINT('Ctrl Pts',(-1.63013849959461,-1.,-0.967387853230345));
#28278=CARTESIAN_POINT('Ctrl Pts',(-1.63420665729798,-1.,-0.970669715997509));
#28279=CARTESIAN_POINT('Ctrl Pts',(-1.63820952658144,-1.,-0.974066058287418));
#28280=CARTESIAN_POINT('Ctrl Pts',(-1.64233990826687,-1.,-0.977689794119416));
#28281=CARTESIAN_POINT('Ctrl Pts',(-1.64665139190656,-1.,-0.981562530939489));
#28282=CARTESIAN_POINT('Ctrl Pts',(-1.65110016612638,-1.,-0.985642622920821));
#28283=CARTESIAN_POINT('Ctrl Pts',(-1.65559044289699,-1.,-0.989855627854165));
#28284=CARTESIAN_POINT('Ctrl Pts',(-1.66001553809947,-1.,-0.994121836661306));
#28285=CARTESIAN_POINT('Ctrl Pts',(-1.66430758030376,-1.,-0.998389654952758));
#28286=CARTESIAN_POINT('Ctrl Pts',(-1.66846059277303,-1.,-1.00265091003727));
#28287=CARTESIAN_POINT('Ctrl Pts',(-1.67250335383293,-1.,-1.00692206696414));
#28288=CARTESIAN_POINT('Ctrl Pts',(-1.67648246776464,-1.,-1.01123236493511));
#28289=CARTESIAN_POINT('Ctrl Pts',(-1.68044289894798,-1.,-1.01561026162773));
#28290=CARTESIAN_POINT('Ctrl Pts',(-1.68440578021706,-1.,-1.02006795074201));
#28291=CARTESIAN_POINT('Ctrl Pts',(-1.68836910178447,-1.,-1.02460180535255));
#28292=CARTESIAN_POINT('Ctrl Pts',(-1.69231840863458,-1.,-1.02919977579147));
#28293=CARTESIAN_POINT('Ctrl Pts',(-1.69623414782771,-1.,-1.03384646003588));
#28294=CARTESIAN_POINT('Ctrl Pts',(-1.70010052930962,-1.,-1.03852922490789));
#28295=CARTESIAN_POINT('Ctrl Pts',(-1.70391338707982,-1.,-1.04324363334554));
#28296=CARTESIAN_POINT('Ctrl Pts',(-1.70767646263649,-1.,-1.04799085404995));
#28297=CARTESIAN_POINT('Ctrl Pts',(-1.71139783543989,-1.,-1.05277517202855));
#28298=CARTESIAN_POINT('Ctrl Pts',(-1.7150865442702,-1.,-1.05760163192479));
#28299=CARTESIAN_POINT('Ctrl Pts',(-1.71874858456904,-1.,-1.06247324680647));
#28300=CARTESIAN_POINT('Ctrl Pts',(-1.72238500928453,-1.,-1.06738966975462));
#28301=CARTESIAN_POINT('Ctrl Pts',(-1.72599406198488,-1.,-1.07234866990252));
#28302=CARTESIAN_POINT('Ctrl Pts',(-1.72957248977424,-1.,-1.0773470373727));
#28303=CARTESIAN_POINT('Ctrl Pts',(-1.73311705663407,-1.,-1.08238162784749));
#28304=CARTESIAN_POINT('Ctrl Pts',(-1.73662628326091,-1.,-1.08745056285427));
#28305=CARTESIAN_POINT('Ctrl Pts',(-1.74010053962247,-1.,-1.09255329056493));
#28306=CARTESIAN_POINT('Ctrl Pts',(-1.74354119236208,-1.,-1.09768999241225));
#28307=CARTESIAN_POINT('Ctrl Pts',(-1.74695004214923,-1.,-1.10286118991143));
#28308=CARTESIAN_POINT('Ctrl Pts',(-1.7503286607592,-1.,-1.10806728183007));
#28309=CARTESIAN_POINT('Ctrl Pts',(-1.7536777209463,-1.,-1.11330807582551));
#28310=CARTESIAN_POINT('Ctrl Pts',(-1.75699720772105,-1.,-1.11858293216763));
#28311=CARTESIAN_POINT('Ctrl Pts',(-1.76028671825096,-1.,-1.12389096855086));
#28312=CARTESIAN_POINT('Ctrl Pts',(-1.7635457196617,-1.,-1.12923123555075));
#28313=CARTESIAN_POINT('Ctrl Pts',(-1.76677384551862,-1.,-1.1346029180462));
#28314=CARTESIAN_POINT('Ctrl Pts',(-1.76997111386769,-1.,-1.14000548336975));
#28315=CARTESIAN_POINT('Ctrl Pts',(-1.77313777896194,-1.,-1.1454385822692));
#28316=CARTESIAN_POINT('Ctrl Pts',(-1.7762742255701,-1.,-1.15090197841515));
#28317=CARTESIAN_POINT('Ctrl Pts',(-1.77938085564275,-1.,-1.15639547194698));
#28318=CARTESIAN_POINT('Ctrl Pts',(-1.78245795881009,-1.,-1.16191881298499));
#28319=CARTESIAN_POINT('Ctrl Pts',(-1.78550566040443,-1.,-1.16747166312303));
#28320=CARTESIAN_POINT('Ctrl Pts',(-1.78852398877616,-1.,-1.17305363177328));
#28321=CARTESIAN_POINT('Ctrl Pts',(-1.79151291552689,-1.,-1.17866429440809));
#28322=CARTESIAN_POINT('Ctrl Pts',(-1.79447240321515,-1.,-1.18430321697432));
#28323=CARTESIAN_POINT('Ctrl Pts',(-1.79740245923478,-1.,-1.18996997934445));
#28324=CARTESIAN_POINT('Ctrl Pts',(-1.80030314369879,-1.,-1.19566418930242));
#28325=CARTESIAN_POINT('Ctrl Pts',(-1.80317454838603,-1.,-1.20138548938974));
#28326=CARTESIAN_POINT('Ctrl Pts',(-1.80601678480707,-1.,-1.20713356605475));
#28327=CARTESIAN_POINT('Ctrl Pts',(-1.80882996917129,-1.,-1.21290815708314));
#28328=CARTESIAN_POINT('Ctrl Pts',(-1.81161420806656,-1.,-1.21870906103557));
#28329=CARTESIAN_POINT('Ctrl Pts',(-1.81436959210434,-1.,-1.2245361330495));
#28330=CARTESIAN_POINT('Ctrl Pts',(-1.8165508718364,-1.,-1.2292186489137));
#28331=CARTESIAN_POINT('Ctrl Pts',(-1.81817389921279,-1.,-1.2327422452705));
#28332=CARTESIAN_POINT('Ctrl Pts',(-1.81925017193666,-1.,-1.23509651170476));
#28333=CARTESIAN_POINT('Ctrl Pts',(-1.81978687191668,-1.,-1.23627494547115));
#28334=CARTESIAN_POINT('',(-1.73811241238545,-1.,-1.34869019493419));
#28335=CARTESIAN_POINT('',(-1.81978687191668,-1.,-1.23627494547115));
#28336=CARTESIAN_POINT('',(-1.31362392696032,-1.,-1.15624053661742));
#28337=CARTESIAN_POINT('Ctrl Pts',(-1.73811241238545,-1.,-1.34869019493419));
#28338=CARTESIAN_POINT('Ctrl Pts',(-1.73682580585691,-1.,-1.34854391898045));
#28339=CARTESIAN_POINT('Ctrl Pts',(-1.73425417885907,-1.,-1.34824783112887));
#28340=CARTESIAN_POINT('Ctrl Pts',(-1.7304014965394,-1.,-1.34779309152035));
#28341=CARTESIAN_POINT('Ctrl Pts',(-1.72527410680674,-1.,-1.34716554819527));
#28342=CARTESIAN_POINT('Ctrl Pts',(-1.7188807715049,-1.,-1.34634568653227));
#28343=CARTESIAN_POINT('Ctrl Pts',(-1.71250340686822,-1.,-1.34549029589416));
#28344=CARTESIAN_POINT('Ctrl Pts',(-1.70614212266738,-1.,-1.34459924533831));
#28345=CARTESIAN_POINT('Ctrl Pts',(-1.69979707754427,-1.,-1.34367237124483));
#28346=CARTESIAN_POINT('Ctrl Pts',(-1.6934684849687,-1.,-1.34270948206319));
#28347=CARTESIAN_POINT('Ctrl Pts',(-1.68715660868764,-1.,-1.341710374848));
#28348=CARTESIAN_POINT('Ctrl Pts',(-1.68086176030362,-1.,-1.34067485185203));
#28349=CARTESIAN_POINT('Ctrl Pts',(-1.67458429426086,-1.,-1.3396027347034));
#28350=CARTESIAN_POINT('Ctrl Pts',(-1.66832460783989,-1.,-1.33849388654388));
#28351=CARTESIAN_POINT('Ctrl Pts',(-1.66208312541983,-1.,-1.33734820885262));
#28352=CARTESIAN_POINT('Ctrl Pts',(-1.65586025952593,-1.,-1.33616559745172));
#28353=CARTESIAN_POINT('Ctrl Pts',(-1.6496563728683,-1.,-1.33494590467993));
#28354=CARTESIAN_POINT('Ctrl Pts',(-1.6434717485603,-1.,-1.33368890676572));
#28355=CARTESIAN_POINT('Ctrl Pts',(-1.63730653475089,-1.,-1.33239425103724));
#28356=CARTESIAN_POINT('Ctrl Pts',(-1.63116079730923,-1.,-1.33106149345645));
#28357=CARTESIAN_POINT('Ctrl Pts',(-1.62503464209797,-1.,-1.3296901950568));
#28358=CARTESIAN_POINT('Ctrl Pts',(-1.61892832270724,-1.,-1.32828000610449));
#28359=CARTESIAN_POINT('Ctrl Pts',(-1.6128423401575,-1.,-1.32683074483356));
#28360=CARTESIAN_POINT('Ctrl Pts',(-1.60677758290954,-1.,-1.32534250785782));
#28361=CARTESIAN_POINT('Ctrl Pts',(-1.60073511858687,-1.,-1.32381550858256));
#28362=CARTESIAN_POINT('Ctrl Pts',(-1.59471591079403,-1.,-1.32224985747682));
#28363=CARTESIAN_POINT('Ctrl Pts',(-1.58872057258245,-1.,-1.32064537110892));
#28364=CARTESIAN_POINT('Ctrl Pts',(-1.58274907898834,-1.,-1.31900135021432));
#28365=CARTESIAN_POINT('Ctrl Pts',(-1.5768005650559,-1.,-1.31731642317187));
#28366=CARTESIAN_POINT('Ctrl Pts',(-1.57087397835723,-1.,-1.31558903860016));
#28367=CARTESIAN_POINT('Ctrl Pts',(-1.56496872402353,-1.,-1.31381795281002));
#28368=CARTESIAN_POINT('Ctrl Pts',(-1.55908521254821,-1.,-1.31200264341696));
#28369=CARTESIAN_POINT('Ctrl Pts',(-1.55322568759481,-1.,-1.31014393684222));
#28370=CARTESIAN_POINT('Ctrl Pts',(-1.54739413957185,-1.,-1.30824393907473));
#28371=CARTESIAN_POINT('Ctrl Pts',(-1.54159462645432,-1.,-1.30630475189556));
#28372=CARTESIAN_POINT('Ctrl Pts',(-1.53582981268977,-1.,-1.30432735639489));
#28373=CARTESIAN_POINT('Ctrl Pts',(-1.53009970283891,-1.,-1.30231064395568));
#28374=CARTESIAN_POINT('Ctrl Pts',(-1.52439957861062,-1.,-1.30024984366328));
#28375=CARTESIAN_POINT('Ctrl Pts',(-1.51872184912724,-1.,-1.29813791800747));
#28376=CARTESIAN_POINT('Ctrl Pts',(-1.51305994241402,-1.,-1.29596850710509));
#28377=CARTESIAN_POINT('Ctrl Pts',(-1.50741159078365,-1.,-1.29373841372842));
#28378=CARTESIAN_POINT('Ctrl Pts',(-1.50178230149776,-1.,-1.29145022885181));
#28379=CARTESIAN_POINT('Ctrl Pts',(-1.49618896881754,-1.,-1.28911506584254));
#28380=CARTESIAN_POINT('Ctrl Pts',(-1.4906522831278,-1.,-1.2867467611644));
#28381=CARTESIAN_POINT('Ctrl Pts',(-1.4851881711891,-1.,-1.28435533880201));
#28382=CARTESIAN_POINT('Ctrl Pts',(-1.47980070347095,-1.,-1.28194158939517));
#28383=CARTESIAN_POINT('Ctrl Pts',(-1.4744717526707,-1.,-1.2794891824849));
#28384=CARTESIAN_POINT('Ctrl Pts',(-1.46916035917133,-1.,-1.27696414831089));
#28385=CARTESIAN_POINT('Ctrl Pts',(-1.46382431332476,-1.,-1.27433119897822));
#28386=CARTESIAN_POINT('Ctrl Pts',(-1.45843906294697,-1.,-1.27156805265289));
#28387=CARTESIAN_POINT('Ctrl Pts',(-1.45301422764247,-1.,-1.2686778680489));
#28388=CARTESIAN_POINT('Ctrl Pts',(-1.44761985001662,-1.,-1.26570925118868));
#28389=CARTESIAN_POINT('Ctrl Pts',(-1.44236470511303,-1.,-1.26273903323859));
#28390=CARTESIAN_POINT('Ctrl Pts',(-1.43734919180848,-1.,-1.25983531012005));
#28391=CARTESIAN_POINT('Ctrl Pts',(-1.43262645609691,-1.,-1.25702687965755));
#28392=CARTESIAN_POINT('Ctrl Pts',(-1.42815938799387,-1.,-1.25426945222639));
#28393=CARTESIAN_POINT('Ctrl Pts',(-1.42378102115575,-1.,-1.2514145557001));
#28394=CARTESIAN_POINT('Ctrl Pts',(-1.41923722596025,-1.,-1.24824430986571));
#28395=CARTESIAN_POINT('Ctrl Pts',(-1.41422913175179,-1.,-1.24450600513056));
#28396=CARTESIAN_POINT('Ctrl Pts',(-1.40845295531283,-1.,-1.23994455029534));
#28397=CARTESIAN_POINT('Ctrl Pts',(-1.40164708206106,-1.,-1.23434087290423));
#28398=CARTESIAN_POINT('Ctrl Pts',(-1.39361389568796,-1.,-1.22752961899387));
#28399=CARTESIAN_POINT('Ctrl Pts',(-1.38420564527715,-1.,-1.21938737280852));
#28400=CARTESIAN_POINT('Ctrl Pts',(-1.37331915607905,-1.,-1.20982812925645));
#28401=CARTESIAN_POINT('Ctrl Pts',(-1.36088705043885,-1.,-1.1987959077932));
#28402=CARTESIAN_POINT('Ctrl Pts',(-1.34687054001093,-1.,-1.18625865667441));
#28403=CARTESIAN_POINT('Ctrl Pts',(-1.33437539347008,-1.,-1.17501305789857));
#28404=CARTESIAN_POINT('Ctrl Pts',(-1.32428080721772,-1.,-1.16589330093588));
#28405=CARTESIAN_POINT('Ctrl Pts',(-1.31722977216397,-1.,-1.15950888730809));
#28406=CARTESIAN_POINT('Ctrl Pts',(-1.31362392696032,-1.,-1.15624053661742));
#28407=CARTESIAN_POINT('',(-1.15624053661742,-1.,-1.31362392696033));
#28408=CARTESIAN_POINT('Origin',(0.,-1.,0.));
#28409=CARTESIAN_POINT('',(-1.34869019493419,-1.,-1.73811241238545));
#28410=CARTESIAN_POINT('Ctrl Pts',(-1.15624053661742,-1.,-1.31362392696033));
#28411=CARTESIAN_POINT('Ctrl Pts',(-1.15950888730433,-1.,-1.3172297721596));
#28412=CARTESIAN_POINT('Ctrl Pts',(-1.16589330092532,-1.,-1.32428080720544));
#28413=CARTESIAN_POINT('Ctrl Pts',(-1.17501305787994,-1.,-1.33437539344842));
#28414=CARTESIAN_POINT('Ctrl Pts',(-1.18625865664915,-1.,-1.34687053998157));
#28415=CARTESIAN_POINT('Ctrl Pts',(-1.1987959077656,-1.,-1.36088705040677));
#28416=CARTESIAN_POINT('Ctrl Pts',(-1.20982812923113,-1.,-1.37331915604962));
#28417=CARTESIAN_POINT('Ctrl Pts',(-1.21938737278853,-1.,-1.38420564525391));
#28418=CARTESIAN_POINT('Ctrl Pts',(-1.22752961898063,-1.,-1.39361389567257));
#28419=CARTESIAN_POINT('Ctrl Pts',(-1.23434087289768,-1.,-1.40164708205345));
#28420=CARTESIAN_POINT('Ctrl Pts',(-1.23994455029421,-1.,-1.40845295531151));
#28421=CARTESIAN_POINT('Ctrl Pts',(-1.24450600513278,-1.,-1.41422913175437));
#28422=CARTESIAN_POINT('Ctrl Pts',(-1.24824430986911,-1.,-1.41923722596421));
#28423=CARTESIAN_POINT('Ctrl Pts',(-1.25141455570299,-1.,-1.42378102115911));
#28424=CARTESIAN_POINT('Ctrl Pts',(-1.25426945222783,-1.,-1.42815938799555));
#28425=CARTESIAN_POINT('Ctrl Pts',(-1.25702687965744,-1.,-1.43262645609679));
#28426=CARTESIAN_POINT('Ctrl Pts',(-1.25983531011894,-1.,-1.43734919180719));
#28427=CARTESIAN_POINT('Ctrl Pts',(-1.26273903323723,-1.,-1.44236470511145));
#28428=CARTESIAN_POINT('Ctrl Pts',(-1.26570925118767,-1.,-1.44761985001544));
#28429=CARTESIAN_POINT('Ctrl Pts',(-1.26867786804854,-1.,-1.45301422764205));
#28430=CARTESIAN_POINT('Ctrl Pts',(-1.27156805265312,-1.,-1.45843906294725));
#28431=CARTESIAN_POINT('Ctrl Pts',(-1.27433119897877,-1.,-1.4638243133254));
#28432=CARTESIAN_POINT('Ctrl Pts',(-1.27696414831144,-1.,-1.46916035917197));
#28433=CARTESIAN_POINT('Ctrl Pts',(-1.27948918248524,-1.,-1.4744717526711));
#28434=CARTESIAN_POINT('Ctrl Pts',(-1.28194158939522,-1.,-1.47980070347102));
#28435=CARTESIAN_POINT('Ctrl Pts',(-1.28435533880184,-1.,-1.48518817118891));
#28436=CARTESIAN_POINT('Ctrl Pts',(-1.28674676116415,-1.,-1.4906522831275));
#28437=CARTESIAN_POINT('Ctrl Pts',(-1.28911506584232,-1.,-1.49618896881729));
#28438=CARTESIAN_POINT('Ctrl Pts',(-1.29145022885171,-1.,-1.50178230149764));
#28439=CARTESIAN_POINT('Ctrl Pts',(-1.29373841372843,-1.,-1.50741159078367));
#28440=CARTESIAN_POINT('Ctrl Pts',(-1.29596850710518,-1.,-1.51305994241412));
#28441=CARTESIAN_POINT('Ctrl Pts',(-1.29813791800757,-1.,-1.51872184912735));
#28442=CARTESIAN_POINT('Ctrl Pts',(-1.30024984366334,-1.,-1.5243995786107));
#28443=CARTESIAN_POINT('Ctrl Pts',(-1.3023106439557,-1.,-1.53009970283893));
#28444=CARTESIAN_POINT('Ctrl Pts',(-1.30432735639487,-1.,-1.53582981268976));
#28445=CARTESIAN_POINT('Ctrl Pts',(-1.30630475189553,-1.,-1.54159462645428));
#28446=CARTESIAN_POINT('Ctrl Pts',(-1.30824393907471,-1.,-1.54739413957183));
#28447=CARTESIAN_POINT('Ctrl Pts',(-1.31014393684221,-1.,-1.55322568759481));
#28448=CARTESIAN_POINT('Ctrl Pts',(-1.31200264341696,-1.,-1.55908521254822));
#28449=CARTESIAN_POINT('Ctrl Pts',(-1.31381795281002,-1.,-1.56496872402352));
#28450=CARTESIAN_POINT('Ctrl Pts',(-1.31558903860015,-1.,-1.57087397835721));
#28451=CARTESIAN_POINT('Ctrl Pts',(-1.31731642317183,-1.,-1.57680056505585));
#28452=CARTESIAN_POINT('Ctrl Pts',(-1.31900135021428,-1.,-1.58274907898829));
#28453=CARTESIAN_POINT('Ctrl Pts',(-1.32064537110891,-1.,-1.58872057258244));
#28454=CARTESIAN_POINT('Ctrl Pts',(-1.32224985747686,-1.,-1.59471591079408));
#28455=CARTESIAN_POINT('Ctrl Pts',(-1.32381550858266,-1.,-1.600735118587));
#28456=CARTESIAN_POINT('Ctrl Pts',(-1.32534250785794,-1.,-1.6067775829097));
#28457=CARTESIAN_POINT('Ctrl Pts',(-1.32683074483365,-1.,-1.61284234015762));
#28458=CARTESIAN_POINT('Ctrl Pts',(-1.32828000610448,-1.,-1.61892832270723));
#28459=CARTESIAN_POINT('Ctrl Pts',(-1.32969019505665,-1.,-1.62503464209777));
#28460=CARTESIAN_POINT('Ctrl Pts',(-1.33106149345618,-1.,-1.63116079730887));
#28461=CARTESIAN_POINT('Ctrl Pts',(-1.33239425103694,-1.,-1.6373065347505));
#28462=CARTESIAN_POINT('Ctrl Pts',(-1.33368890676554,-1.,-1.64347174856007));
#28463=CARTESIAN_POINT('Ctrl Pts',(-1.33494590468003,-1.,-1.64965637286843));
#28464=CARTESIAN_POINT('Ctrl Pts',(-1.33616559745217,-1.,-1.65586025952651));
#28465=CARTESIAN_POINT('Ctrl Pts',(-1.33734820885331,-1.,-1.66208312542073));
#28466=CARTESIAN_POINT('Ctrl Pts',(-1.33849388654458,-1.,-1.66832460784078));
#28467=CARTESIAN_POINT('Ctrl Pts',(-1.33960273470372,-1.,-1.67458429426126));
#28468=CARTESIAN_POINT('Ctrl Pts',(-1.3406748518516,-1.,-1.68086176030308));
#28469=CARTESIAN_POINT('Ctrl Pts',(-1.34171037484673,-1.,-1.68715660868602));
#28470=CARTESIAN_POINT('Ctrl Pts',(-1.34270948206139,-1.,-1.6934684849664));
#28471=CARTESIAN_POINT('Ctrl Pts',(-1.34367237124322,-1.,-1.69979707754221));
#28472=CARTESIAN_POINT('Ctrl Pts',(-1.34459924533783,-1.,-1.70614212266676));
#28473=CARTESIAN_POINT('Ctrl Pts',(-1.34549029589563,-1.,-1.71250340687011));
#28474=CARTESIAN_POINT('Ctrl Pts',(-1.34634568653586,-1.,-1.7188807715095));
#28475=CARTESIAN_POINT('Ctrl Pts',(-1.34716554820013,-1.,-1.72527410681298));
#28476=CARTESIAN_POINT('Ctrl Pts',(-1.3477930915247,-1.,-1.73040149654497));
#28477=CARTESIAN_POINT('Ctrl Pts',(-1.34824783113158,-1.,-1.73425417886255));
#28478=CARTESIAN_POINT('Ctrl Pts',(-1.34854391898145,-1.,-1.73682580585819));
#28479=CARTESIAN_POINT('Ctrl Pts',(-1.34869019493419,-1.,-1.73811241238545));
#28480=CARTESIAN_POINT('',(-1.23627494547115,-1.,-1.81978687191668));
#28481=CARTESIAN_POINT('',(-1.34869019493419,-1.,-1.73811241238545));
#28482=CARTESIAN_POINT('',(-0.892032620296855,-1.,-1.5055822144029));
#28483=CARTESIAN_POINT('Ctrl Pts',(-1.23627494547115,-1.,-1.81978687191668));
#28484=CARTESIAN_POINT('Ctrl Pts',(-1.23509651170384,-1.,-1.81925017193531));
#28485=CARTESIAN_POINT('Ctrl Pts',(-1.23274224526804,-1.,-1.81817389920914));
#28486=CARTESIAN_POINT('Ctrl Pts',(-1.22921864890975,-1.,-1.81655087183054));
#28487=CARTESIAN_POINT('Ctrl Pts',(-1.22453613304507,-1.,-1.81436959209778));
#28488=CARTESIAN_POINT('Ctrl Pts',(-1.2187090610323,-1.,-1.81161420806172));
#28489=CARTESIAN_POINT('Ctrl Pts',(-1.2129081570818,-1.,-1.80882996916931));
#28490=CARTESIAN_POINT('Ctrl Pts',(-1.20713356605519,-1.,-1.80601678480772));
#28491=CARTESIAN_POINT('Ctrl Pts',(-1.2013854893912,-1.,-1.8031745483882));
#28492=CARTESIAN_POINT('Ctrl Pts',(-1.19566418930405,-1.,-1.80030314370121));
#28493=CARTESIAN_POINT('Ctrl Pts',(-1.1899699793456,-1.,-1.79740245923649));
#28494=CARTESIAN_POINT('Ctrl Pts',(-1.18430321697471,-1.,-1.79447240321572));
#28495=CARTESIAN_POINT('Ctrl Pts',(-1.17866429440781,-1.,-1.79151291552646));
#28496=CARTESIAN_POINT('Ctrl Pts',(-1.17305363177265,-1.,-1.78852398877523));
#28497=CARTESIAN_POINT('Ctrl Pts',(-1.16747166312239,-1.,-1.78550566040349));
#28498=CARTESIAN_POINT('Ctrl Pts',(-1.16191881298458,-1.,-1.78245795880949));
#28499=CARTESIAN_POINT('Ctrl Pts',(-1.15639547194689,-1.,-1.77938085564261));
#28500=CARTESIAN_POINT('Ctrl Pts',(-1.15090197841531,-1.,-1.77627422557034));
#28501=CARTESIAN_POINT('Ctrl Pts',(-1.14543858226948,-1.,-1.77313777896234));
#28502=CARTESIAN_POINT('Ctrl Pts',(-1.14000548337,-1.,-1.76997111386806));
#28503=CARTESIAN_POINT('Ctrl Pts',(-1.13460291804635,-1.,-1.76677384551883));
#28504=CARTESIAN_POINT('Ctrl Pts',(-1.12923123555076,-1.,-1.76354571966171));
#28505=CARTESIAN_POINT('Ctrl Pts',(-1.12389096855078,-1.,-1.76028671825084));
#28506=CARTESIAN_POINT('Ctrl Pts',(-1.11858293216752,-1.,-1.75699720772089));
#28507=CARTESIAN_POINT('Ctrl Pts',(-1.11330807582542,-1.,-1.75367772094617));
#28508=CARTESIAN_POINT('Ctrl Pts',(-1.10806728183003,-1.,-1.75032866075914));
#28509=CARTESIAN_POINT('Ctrl Pts',(-1.10286118991144,-1.,-1.74695004214924));
#28510=CARTESIAN_POINT('Ctrl Pts',(-1.09768999241229,-1.,-1.74354119236212));
#28511=CARTESIAN_POINT('Ctrl Pts',(-1.09255329056496,-1.,-1.74010053962252));
#28512=CARTESIAN_POINT('Ctrl Pts',(-1.08745056285429,-1.,-1.73662628326093));
#28513=CARTESIAN_POINT('Ctrl Pts',(-1.08238162784749,-1.,-1.73311705663407));
#28514=CARTESIAN_POINT('Ctrl Pts',(-1.0773470373727,-1.,-1.72957248977424));
#28515=CARTESIAN_POINT('Ctrl Pts',(-1.07234866990252,-1.,-1.72599406198489));
#28516=CARTESIAN_POINT('Ctrl Pts',(-1.06738966975463,-1.,-1.72238500928456));
#28517=CARTESIAN_POINT('Ctrl Pts',(-1.0624732468065,-1.,-1.71874858456908));
#28518=CARTESIAN_POINT('Ctrl Pts',(-1.05760163192481,-1.,-1.71508654427022));
#28519=CARTESIAN_POINT('Ctrl Pts',(-1.05277517202854,-1.,-1.71139783543986));
#28520=CARTESIAN_POINT('Ctrl Pts',(-1.0479908540499,-1.,-1.70767646263641));
#28521=CARTESIAN_POINT('Ctrl Pts',(-1.04324363334546,-1.,-1.70391338707969));
#28522=CARTESIAN_POINT('Ctrl Pts',(-1.03852922490782,-1.,-1.70010052930951));
#28523=CARTESIAN_POINT('Ctrl Pts',(-1.03384646003587,-1.,-1.69623414782769));
#28524=CARTESIAN_POINT('Ctrl Pts',(-1.02919977579155,-1.,-1.69231840863471));
#28525=CARTESIAN_POINT('Ctrl Pts',(-1.02460180535272,-1.,-1.68836910178475));
#28526=CARTESIAN_POINT('Ctrl Pts',(-1.02006795074222,-1.,-1.68440578021739));
#28527=CARTESIAN_POINT('Ctrl Pts',(-1.01561026162787,-1.,-1.6804428989482));
#28528=CARTESIAN_POINT('Ctrl Pts',(-1.01123236493507,-1.,-1.67648246776457));
#28529=CARTESIAN_POINT('Ctrl Pts',(-1.00692206696387,-1.,-1.67250335383248));
#28530=CARTESIAN_POINT('Ctrl Pts',(-1.00265091003682,-1.,-1.66846059277231));
#28531=CARTESIAN_POINT('Ctrl Pts',(-0.998389654952317,-1.,-1.66430758030304));
#28532=CARTESIAN_POINT('Ctrl Pts',(-0.994121836661116,-1.,-1.66001553809916));
#28533=CARTESIAN_POINT('Ctrl Pts',(-0.98985562785445,-1.,-1.65559044289746));
#28534=CARTESIAN_POINT('Ctrl Pts',(-0.985642622921626,-1.,-1.6511001661277));
#28535=CARTESIAN_POINT('Ctrl Pts',(-0.981562530940574,-1.,-1.64665139190834));
#28536=CARTESIAN_POINT('Ctrl Pts',(-0.977689794120297,-1.,-1.64233990826831));
#28537=CARTESIAN_POINT('Ctrl Pts',(-0.974066058287501,-1.,-1.63820952658157));
#28538=CARTESIAN_POINT('Ctrl Pts',(-0.970669715996356,-1.,-1.63420665729609));
#28539=CARTESIAN_POINT('Ctrl Pts',(-0.967387853228041,-1.,-1.63013849959083));
#28540=CARTESIAN_POINT('Ctrl Pts',(-0.964046107037821,-1.,-1.6257193066974));
#28541=CARTESIAN_POINT('Ctrl Pts',(-0.960438326099958,-1.,-1.62061638139929));
#28542=CARTESIAN_POINT('Ctrl Pts',(-0.956354422921573,-1.,-1.61449324337233));
#28543=CARTESIAN_POINT('Ctrl Pts',(-0.951613284361248,-1.,-1.60706069897794));
#28544=CARTESIAN_POINT('Ctrl Pts',(-0.946078063325796,-1.,-1.59810042045408));
#28545=CARTESIAN_POINT('Ctrl Pts',(-0.939646377909319,-1.,-1.58744937489796));
#28546=CARTESIAN_POINT('Ctrl Pts',(-0.932246680128849,-1.,-1.57499388385561));
#28547=CARTESIAN_POINT('Ctrl Pts',(-0.923832188966322,-1.,-1.56065988582509));
#28548=CARTESIAN_POINT('Ctrl Pts',(-0.91437591904658,-1.,-1.54440491152808));
#28549=CARTESIAN_POINT('Ctrl Pts',(-0.905967409640499,-1.,-1.52984849890434));
#28550=CARTESIAN_POINT('Ctrl Pts',(-0.89918504749193,-1.,-1.51805569591479));
#28551=CARTESIAN_POINT('Ctrl Pts',(-0.894452006967538,-1.,-1.50980486807181));
#28552=CARTESIAN_POINT('Ctrl Pts',(-0.892032620296855,-1.,-1.5055822144029));
#28553=CARTESIAN_POINT('',(-0.693717979106305,-1.,-1.60662857109684));
#28554=CARTESIAN_POINT('Origin',(0.,-1.,0.));
#28555=CARTESIAN_POINT('',(-0.745574324794401,-1.,-2.0698113262342));
#28556=CARTESIAN_POINT('Ctrl Pts',(-0.693717979106305,-1.,-1.60662857109684));
#28557=CARTESIAN_POINT('Ctrl Pts',(-0.69571209787897,-1.,-1.61106790957619));
#28558=CARTESIAN_POINT('Ctrl Pts',(-0.699605146398837,-1.,-1.61974673471117));
#28559=CARTESIAN_POINT('Ctrl Pts',(-0.705159151977294,-1.,-1.6321654166204));
#28560=CARTESIAN_POINT('Ctrl Pts',(-0.711993139340447,-1.,-1.64752408828442));
#28561=CARTESIAN_POINT('Ctrl Pts',(-0.71958543378795,-1.,-1.66472880551777));
#28562=CARTESIAN_POINT('Ctrl Pts',(-0.726235967982445,-1.,-1.67996158451922));
#28563=CARTESIAN_POINT('Ctrl Pts',(-0.731963238685357,-1.,-1.69326921972915));
#28564=CARTESIAN_POINT('Ctrl Pts',(-0.736799665716932,-1.,-1.70473309004249));
#28565=CARTESIAN_POINT('Ctrl Pts',(-0.74079516202821,-1.,-1.71447789751001));
#28566=CARTESIAN_POINT('Ctrl Pts',(-0.744021445433093,-1.,-1.72268229916769));
#28567=CARTESIAN_POINT('Ctrl Pts',(-0.746574710097752,-1.,-1.72958533647714));
#28568=CARTESIAN_POINT('Ctrl Pts',(-0.74858246295687,-1.,-1.7355035168033));
#28569=CARTESIAN_POINT('Ctrl Pts',(-0.750193435981249,-1.,-1.74080458267114));
#28570=CARTESIAN_POINT('Ctrl Pts',(-0.751555614164482,-1.,-1.74585086852502));
#28571=CARTESIAN_POINT('Ctrl Pts',(-0.752797683531314,-1.,-1.75095139468794));
#28572=CARTESIAN_POINT('Ctrl Pts',(-0.754009254027829,-1.,-1.75631083600019));
#28573=CARTESIAN_POINT('Ctrl Pts',(-0.755220979974461,-1.,-1.76197817240128));
#28574=CARTESIAN_POINT('Ctrl Pts',(-0.75642189602781,-1.,-1.76789396002998));
#28575=CARTESIAN_POINT('Ctrl Pts',(-0.757578264077029,-1.,-1.77394167108292));
#28576=CARTESIAN_POINT('Ctrl Pts',(-0.758650626677518,-1.,-1.77999411220945));
#28577=CARTESIAN_POINT('Ctrl Pts',(-0.759614401110189,-1.,-1.78596964884604));
#28578=CARTESIAN_POINT('Ctrl Pts',(-0.760469555880749,-1.,-1.7918581561088));
#28579=CARTESIAN_POINT('Ctrl Pts',(-0.761229695230558,-1.,-1.79768986997783));
#28580=CARTESIAN_POINT('Ctrl Pts',(-0.761915336443547,-1.,-1.80351583877342));
#28581=CARTESIAN_POINT('Ctrl Pts',(-0.762546129463938,-1.,-1.80938551463965));
#28582=CARTESIAN_POINT('Ctrl Pts',(-0.763132003836634,-1.,-1.8153211840553));
#28583=CARTESIAN_POINT('Ctrl Pts',(-0.763673465462726,-1.,-1.82131873145266));
#28584=CARTESIAN_POINT('Ctrl Pts',(-0.764165902605995,-1.,-1.82735991200065));
#28585=CARTESIAN_POINT('Ctrl Pts',(-0.764602549687853,-1.,-1.83342077227142));
#28586=CARTESIAN_POINT('Ctrl Pts',(-0.764978057881737,-1.,-1.83948181064835));
#28587=CARTESIAN_POINT('Ctrl Pts',(-0.765291664862029,-1.,-1.84553698875924));
#28588=CARTESIAN_POINT('Ctrl Pts',(-0.765545710619062,-1.,-1.85158945130063));
#28589=CARTESIAN_POINT('Ctrl Pts',(-0.765744212909318,-1.,-1.85764741390394));
#28590=CARTESIAN_POINT('Ctrl Pts',(-0.765891519092547,-1.,-1.86372027063312));
#28591=CARTESIAN_POINT('Ctrl Pts',(-0.765990708546091,-1.,-1.86981398314341));
#28592=CARTESIAN_POINT('Ctrl Pts',(-0.766042837036744,-1.,-1.87592888967883));
#28593=CARTESIAN_POINT('Ctrl Pts',(-0.766047794851865,-1.,-1.88206215302561));
#28594=CARTESIAN_POINT('Ctrl Pts',(-0.766004837062091,-1.,-1.88820926433409));
#28595=CARTESIAN_POINT('Ctrl Pts',(-0.765913193856978,-1.,-1.89436577771388));
#28596=CARTESIAN_POINT('Ctrl Pts',(-0.765772772593386,-1.,-1.90052930393596));
#28597=CARTESIAN_POINT('Ctrl Pts',(-0.765584196937919,-1.,-1.90669961402356));
#28598=CARTESIAN_POINT('Ctrl Pts',(-0.765348465884722,-1.,-1.91287765805169));
#28599=CARTESIAN_POINT('Ctrl Pts',(-0.765066729667088,-1.,-1.91906491634196));
#28600=CARTESIAN_POINT('Ctrl Pts',(-0.764740025488211,-1.,-1.92526263537048));
#28601=CARTESIAN_POINT('Ctrl Pts',(-0.764369010673941,-1.,-1.93147105496382));
#28602=CARTESIAN_POINT('Ctrl Pts',(-0.763954049121458,-1.,-1.93768964875886));
#28603=CARTESIAN_POINT('Ctrl Pts',(-0.763495333538629,-1.,-1.9439174661764));
#28604=CARTESIAN_POINT('Ctrl Pts',(-0.762992990878769,-1.,-1.95015342590024));
#28605=CARTESIAN_POINT('Ctrl Pts',(-0.762447203806179,-1.,-1.95639665309869));
#28606=CARTESIAN_POINT('Ctrl Pts',(-0.761858300014423,-1.,-1.96264672744186));
#28607=CARTESIAN_POINT('Ctrl Pts',(-0.76122669048382,-1.,-1.96890351582499));
#28608=CARTESIAN_POINT('Ctrl Pts',(-0.760552825409757,-1.,-1.97516705321494));
#28609=CARTESIAN_POINT('Ctrl Pts',(-0.75983714745219,-1.,-1.98143741418172));
#28610=CARTESIAN_POINT('Ctrl Pts',(-0.759080037802488,-1.,-1.98771456680874));
#28611=CARTESIAN_POINT('Ctrl Pts',(-0.758281796766761,-1.,-1.99399831098817));
#28612=CARTESIAN_POINT('Ctrl Pts',(-0.757442676862724,-1.,-2.00028834739178));
#28613=CARTESIAN_POINT('Ctrl Pts',(-0.75656290464667,-1.,-2.0065843158773));
#28614=CARTESIAN_POINT('Ctrl Pts',(-0.755642704957865,-1.,-2.01288584328084));
#28615=CARTESIAN_POINT('Ctrl Pts',(-0.754682330722816,-1.,-2.01919259405809));
#28616=CARTESIAN_POINT('Ctrl Pts',(-0.753682061112768,-1.,-2.02550428623313));
#28617=CARTESIAN_POINT('Ctrl Pts',(-0.752642180487211,-1.,-2.03182068456221));
#28618=CARTESIAN_POINT('Ctrl Pts',(-0.751562963361115,-1.,-2.03814160092099));
#28619=CARTESIAN_POINT('Ctrl Pts',(-0.750444657875576,-1.,-2.04446689147979));
#28620=CARTESIAN_POINT('Ctrl Pts',(-0.749287468665046,-1.,-2.05079645592154));
#28621=CARTESIAN_POINT('Ctrl Pts',(-0.748091554183802,-1.,-2.05713023031006));
#28622=CARTESIAN_POINT('Ctrl Pts',(-0.747103932787919,-1.,-2.06220058927826));
#28623=CARTESIAN_POINT('Ctrl Pts',(-0.7463458715442,-1.,-2.06600523016815));
#28624=CARTESIAN_POINT('Ctrl Pts',(-0.745832791378367,-1.,-2.06854248895728));
#28625=CARTESIAN_POINT('Ctrl Pts',(-0.745574324794401,-1.,-2.0698113262342));
#28626=CARTESIAN_POINT('',(-0.61342227326009,-1.,-2.11275013067528));
#28627=CARTESIAN_POINT('',(-0.745574324794401,-1.,-2.0698113262342));
#28628=CARTESIAN_POINT('',(-0.383122945602004,-1.,-1.7075470150345));
#28629=CARTESIAN_POINT('Ctrl Pts',(-0.61342227326009,-1.,-2.11275013067528));
#28630=CARTESIAN_POINT('Ctrl Pts',(-0.6124673655618,-1.,-2.11187554259986));
#28631=CARTESIAN_POINT('Ctrl Pts',(-0.610560911689899,-1.,-2.11012443807238));
#28632=CARTESIAN_POINT('Ctrl Pts',(-0.607711315454876,-1.,-2.1074919961518));
#28633=CARTESIAN_POINT('Ctrl Pts',(-0.60393203073603,-1.,-2.10397049886949));
#28634=CARTESIAN_POINT('Ctrl Pts',(-0.599241616420533,-1.,-2.0995493086477));
#28635=CARTESIAN_POINT('Ctrl Pts',(-0.594585006052162,-1.,-2.0951087622027));
#28636=CARTESIAN_POINT('Ctrl Pts',(-0.589962365403406,-1.,-2.09064881812129));
#28637=CARTESIAN_POINT('Ctrl Pts',(-0.585373918991617,-1.,-2.08616943727951));
#28638=CARTESIAN_POINT('Ctrl Pts',(-0.580819952108063,-1.,-2.08167059018418));
#28639=CARTESIAN_POINT('Ctrl Pts',(-0.576300797416844,-1.,-2.07715226767559));
#28640=CARTESIAN_POINT('Ctrl Pts',(-0.571816823242603,-1.,-2.07261449292824));
#28641=CARTESIAN_POINT('Ctrl Pts',(-0.567368421181087,-1.,-2.06805732997334));
#28642=CARTESIAN_POINT('Ctrl Pts',(-0.562955993082261,-1.,-2.06348090160589));
#28643=CARTESIAN_POINT('Ctrl Pts',(-0.558579940185151,-1.,-2.05888537756462));
#28644=CARTESIAN_POINT('Ctrl Pts',(-0.554240657463906,-1.,-2.05427091604413));
#28645=CARTESIAN_POINT('Ctrl Pts',(-0.549938525150295,-1.,-2.04963761077958));
#28646=CARTESIAN_POINT('Ctrl Pts',(-0.54567390381743,-1.,-2.04498544714588));
#28647=CARTESIAN_POINT('Ctrl Pts',(-0.541447120615659,-1.,-2.04031422690527));
#28648=CARTESIAN_POINT('Ctrl Pts',(-0.537258489833262,-1.,-2.03562362954037));
#28649=CARTESIAN_POINT('Ctrl Pts',(-0.533108355132977,-1.,-2.03091336214426));
#28650=CARTESIAN_POINT('Ctrl Pts',(-0.528997127241914,-1.,-2.0261832908329));
#28651=CARTESIAN_POINT('Ctrl Pts',(-0.524925318333476,-1.,-2.02143356304698));
#28652=CARTESIAN_POINT('Ctrl Pts',(-0.52089359039937,-1.,-2.01666477917286));
#28653=CARTESIAN_POINT('Ctrl Pts',(-0.516902681728687,-1.,-2.01187773939242));
#28654=CARTESIAN_POINT('Ctrl Pts',(-0.512953306961792,-1.,-2.00707309946949));
#28655=CARTESIAN_POINT('Ctrl Pts',(-0.509046069886157,-1.,-2.00225107134734));
#28656=CARTESIAN_POINT('Ctrl Pts',(-0.505181361323026,-1.,-1.99741107463572));
#28657=CARTESIAN_POINT('Ctrl Pts',(-0.501359287727146,-1.,-1.99255149126155));
#28658=CARTESIAN_POINT('Ctrl Pts',(-0.497579909545574,-1.,-1.98767044752932));
#28659=CARTESIAN_POINT('Ctrl Pts',(-0.493843476541495,-1.,-1.98276658761821));
#28660=CARTESIAN_POINT('Ctrl Pts',(-0.490150627860952,-1.,-1.97783973019229));
#28661=CARTESIAN_POINT('Ctrl Pts',(-0.486502692907659,-1.,-1.97289186263272));
#28662=CARTESIAN_POINT('Ctrl Pts',(-0.482901662120691,-1.,-1.96792703422362));
#28663=CARTESIAN_POINT('Ctrl Pts',(-0.479349583074855,-1.,-1.96294933055943));
#28664=CARTESIAN_POINT('Ctrl Pts',(-0.475848034683176,-1.,-1.95796111148177));
#28665=CARTESIAN_POINT('Ctrl Pts',(-0.472397672264072,-1.,-1.95296148278133));
#28666=CARTESIAN_POINT('Ctrl Pts',(-0.468997482913135,-1.,-1.94794381136514));
#28667=CARTESIAN_POINT('Ctrl Pts',(-0.46564546202603,-1.,-1.9428979419619));
#28668=CARTESIAN_POINT('Ctrl Pts',(-0.462340031009056,-1.,-1.93781486640821));
#28669=CARTESIAN_POINT('Ctrl Pts',(-0.459081234547926,-1.,-1.93269066517934));
#28670=CARTESIAN_POINT('Ctrl Pts',(-0.455872005174371,-1.,-1.92753067150476));
#28671=CARTESIAN_POINT('Ctrl Pts',(-0.452719478359432,-1.,-1.92235380648502));
#28672=CARTESIAN_POINT('Ctrl Pts',(-0.449632260106662,-1.,-1.91718342555755));
#28673=CARTESIAN_POINT('Ctrl Pts',(-0.446617343485711,-1.,-1.9120369998112));
#28674=CARTESIAN_POINT('Ctrl Pts',(-0.443677556849151,-1.,-1.90691756144898));
#28675=CARTESIAN_POINT('Ctrl Pts',(-0.440807833704038,-1.,-1.90180124389086));
#28676=CARTESIAN_POINT('Ctrl Pts',(-0.437995003948244,-1.,-1.89663648956466));
#28677=CARTESIAN_POINT('Ctrl Pts',(-0.435225660963383,-1.,-1.89136993975504));
#28678=CARTESIAN_POINT('Ctrl Pts',(-0.432493038548748,-1.,-1.88596913666793));
#28679=CARTESIAN_POINT('Ctrl Pts',(-0.429803062482344,-1.,-1.88044229001832));
#28680=CARTESIAN_POINT('Ctrl Pts',(-0.427183828519102,-1.,-1.87486989291484));
#28681=CARTESIAN_POINT('Ctrl Pts',(-0.424678177291359,-1.,-1.86937803944323));
#28682=CARTESIAN_POINT('Ctrl Pts',(-0.422327307418275,-1.,-1.86408083334028));
#28683=CARTESIAN_POINT('Ctrl Pts',(-0.420157287975619,-1.,-1.85903281096686));
#28684=CARTESIAN_POINT('Ctrl Pts',(-0.418164129143534,-1.,-1.85417632856234));
#28685=CARTESIAN_POINT('Ctrl Pts',(-0.416300022038864,-1.,-1.84929312929882));
#28686=CARTESIAN_POINT('Ctrl Pts',(-0.41448743825434,-1.,-1.8440575707371));
#28687=CARTESIAN_POINT('Ctrl Pts',(-0.412633125322162,-1.,-1.83808953475839));
#28688=CARTESIAN_POINT('Ctrl Pts',(-0.410641256301675,-1.,-1.83100408895216));
#28689=CARTESIAN_POINT('Ctrl Pts',(-0.408428948108533,-1.,-1.8224702267854));
#28690=CARTESIAN_POINT('Ctrl Pts',(-0.405933518411838,-1.,-1.81223801813988));
#28691=CARTESIAN_POINT('Ctrl Pts',(-0.403107976170441,-1.,-1.80012077176221));
#28692=CARTESIAN_POINT('Ctrl Pts',(-0.39991940378308,-1.,-1.78598826347533));
#28693=CARTESIAN_POINT('Ctrl Pts',(-0.39634619612042,-1.,-1.7697556004756));
#28694=CARTESIAN_POINT('Ctrl Pts',(-0.392375812294307,-1.,-1.75137405313962));
#28695=CARTESIAN_POINT('Ctrl Pts',(-0.388877023509191,-1.,-1.7349317097561));
#28696=CARTESIAN_POINT('Ctrl Pts',(-0.38607079032701,-1.,-1.72162022246158));
#28697=CARTESIAN_POINT('Ctrl Pts',(-0.384119047315542,-1.,-1.71231062891958));
#28698=CARTESIAN_POINT('Ctrl Pts',(-0.383122945602004,-1.,-1.7075470150345));
#28699=CARTESIAN_POINT('',(-0.163289472382896,-1.,-1.74236521665491));
#28700=CARTESIAN_POINT('Origin',(0.,-1.,0.));
#28701=CARTESIAN_POINT('',(-0.0694764450219581,-1.,-2.19890268624765));
#28702=CARTESIAN_POINT('Ctrl Pts',(-0.163289472382896,-1.,-1.74236521665491));
#28703=CARTESIAN_POINT('Ctrl Pts',(-0.163814161002002,-1.,-1.7472034950333));
#28704=CARTESIAN_POINT('Ctrl Pts',(-0.164834765707158,-1.,-1.75666056638427));
#28705=CARTESIAN_POINT('Ctrl Pts',(-0.1662793551464,-1.,-1.77018771684844));
#28706=CARTESIAN_POINT('Ctrl Pts',(-0.168032772805197,-1.,-1.7869064998507));
#28707=CARTESIAN_POINT('Ctrl Pts',(-0.169936923904608,-1.,-1.80561530629706));
#28708=CARTESIAN_POINT('Ctrl Pts',(-0.171554770204119,-1.,-1.82215766811545));
#28709=CARTESIAN_POINT('Ctrl Pts',(-0.1728894428919,-1.,-1.83658380527692));
#28710=CARTESIAN_POINT('Ctrl Pts',(-0.173946627587731,-1.,-1.8489811319852));
#28711=CARTESIAN_POINT('Ctrl Pts',(-0.17473525927603,-1.,-1.85948367088837));
#28712=CARTESIAN_POINT('Ctrl Pts',(-0.175268337590758,-1.,-1.86828349694799));
#28713=CARTESIAN_POINT('Ctrl Pts',(-0.175563480746485,-1.,-1.87563767773588));
#28714=CARTESIAN_POINT('Ctrl Pts',(-0.175644148889699,-1.,-1.88188663145367));
#28715=CARTESIAN_POINT('Ctrl Pts',(-0.175538155840648,-1.,-1.88742606273259));
#28716=CARTESIAN_POINT('Ctrl Pts',(-0.175274276190844,-1.,-1.892646301985));
#28717=CARTESIAN_POINT('Ctrl Pts',(-0.174879405091263,-1.,-1.89788101117132));
#28718=CARTESIAN_POINT('Ctrl Pts',(-0.174375518661085,-1.,-1.90335253862834));
#28719=CARTESIAN_POINT('Ctrl Pts',(-0.173776635257817,-1.,-1.90911693975267));
#28720=CARTESIAN_POINT('Ctrl Pts',(-0.173090695383496,-1.,-1.91511429159527));
#28721=CARTESIAN_POINT('Ctrl Pts',(-0.172321621259514,-1.,-1.9212233439798));
#28722=CARTESIAN_POINT('Ctrl Pts',(-0.171471191532988,-1.,-1.92731093582036));
#28723=CARTESIAN_POINT('Ctrl Pts',(-0.170541253116202,-1.,-1.93329183155539));
#28724=CARTESIAN_POINT('Ctrl Pts',(-0.169534904817491,-1.,-1.93915639211581));
#28725=CARTESIAN_POINT('Ctrl Pts',(-0.168455741607556,-1.,-1.94493757756931));
#28726=CARTESIAN_POINT('Ctrl Pts',(-0.167307501784475,-1.,-1.95069027794294));
#28727=CARTESIAN_POINT('Ctrl Pts',(-0.166093592002812,-1.,-1.9564675971873));
#28728=CARTESIAN_POINT('Ctrl Pts',(-0.164816568920269,-1.,-1.96229379940136));
#28729=CARTESIAN_POINT('Ctrl Pts',(-0.163478185457734,-1.,-1.96816512677967));
#28730=CARTESIAN_POINT('Ctrl Pts',(-0.162079693556289,-1.,-1.97406280235188));
#28731=CARTESIAN_POINT('Ctrl Pts',(-0.160622060784611,-1.,-1.97996195437559));
#28732=CARTESIAN_POINT('Ctrl Pts',(-0.159106226437299,-1.,-1.98584238283292));
#28733=CARTESIAN_POINT('Ctrl Pts',(-0.157533331459227,-1.,-1.99169810931908));
#28734=CARTESIAN_POINT('Ctrl Pts',(-0.155904629548783,-1.,-1.99753284771497));
#28735=CARTESIAN_POINT('Ctrl Pts',(-0.154221403049722,-1.,-2.00335565310543));
#28736=CARTESIAN_POINT('Ctrl Pts',(-0.15248488362145,-1.,-2.00917680318424));
#28737=CARTESIAN_POINT('Ctrl Pts',(-0.150696157673078,-1.,-2.01500291940238));
#28738=CARTESIAN_POINT('Ctrl Pts',(-0.148856124775337,-1.,-2.02083464969894));
#28739=CARTESIAN_POINT('Ctrl Pts',(-0.146965557332583,-1.,-2.02666926182017));
#28740=CARTESIAN_POINT('Ctrl Pts',(-0.145025140186057,-1.,-2.03250223739942));
#28741=CARTESIAN_POINT('Ctrl Pts',(-0.143035515058209,-1.,-2.03832911025912));
#28742=CARTESIAN_POINT('Ctrl Pts',(-0.140997332152546,-1.,-2.04414757947916));
#28743=CARTESIAN_POINT('Ctrl Pts',(-0.138911255368966,-1.,-2.04995762001328));
#28744=CARTESIAN_POINT('Ctrl Pts',(-0.136777941218044,-1.,-2.05576044414264));
#28745=CARTESIAN_POINT('Ctrl Pts',(-0.134598026192106,-1.,-2.06155781517842));
#28746=CARTESIAN_POINT('Ctrl Pts',(-0.13237211154771,-1.,-2.06735123910326));
#28747=CARTESIAN_POINT('Ctrl Pts',(-0.130100748328403,-1.,-2.07314114713063));
#28748=CARTESIAN_POINT('Ctrl Pts',(-0.12778444527612,-1.,-2.07892715110987));
#28749=CARTESIAN_POINT('Ctrl Pts',(-0.125423679412061,-1.,-2.08470840653643));
#28750=CARTESIAN_POINT('Ctrl Pts',(-0.123018905621083,-1.,-2.09048392424825));
#28751=CARTESIAN_POINT('Ctrl Pts',(-0.120570567965122,-1.,-2.0962529286773));
#28752=CARTESIAN_POINT('Ctrl Pts',(-0.118079107988355,-1.,-2.102015121329));
#28753=CARTESIAN_POINT('Ctrl Pts',(-0.115544957687926,-1.,-2.10777050261309));
#28754=CARTESIAN_POINT('Ctrl Pts',(-0.112968534419737,-1.,-2.11351924490306));
#28755=CARTESIAN_POINT('Ctrl Pts',(-0.110350236135025,-1.,-2.11926155590865));
#28756=CARTESIAN_POINT('Ctrl Pts',(-0.10769043523109,-1.,-2.12499752307));
#28757=CARTESIAN_POINT('Ctrl Pts',(-0.104989479152739,-1.,-2.13072704887293));
#28758=CARTESIAN_POINT('Ctrl Pts',(-0.1022477005561,-1.,-2.13644992667165));
#28759=CARTESIAN_POINT('Ctrl Pts',(-0.0994654261990915,-1.,-2.14216588396025));
#28760=CARTESIAN_POINT('Ctrl Pts',(-0.0966429852305459,-1.,-2.14787463531795));
#28761=CARTESIAN_POINT('Ctrl Pts',(-0.0937807218867643,-1.,-2.1535759397817));
#28762=CARTESIAN_POINT('Ctrl Pts',(-0.0908789888107265,-1.,-2.15926961544516));
#28763=CARTESIAN_POINT('Ctrl Pts',(-0.0879381291386923,-1.,-2.16495552645014));
#28764=CARTESIAN_POINT('Ctrl Pts',(-0.0849584620835372,-1.,-2.17063357870952));
#28765=CARTESIAN_POINT('Ctrl Pts',(-0.0819402680872765,-1.,-2.176303712113));
#28766=CARTESIAN_POINT('Ctrl Pts',(-0.0788837727685243,-1.,-2.18196589448887));
#28767=CARTESIAN_POINT('Ctrl Pts',(-0.0757891465836148,-1.,-2.1876201139953));
#28768=CARTESIAN_POINT('Ctrl Pts',(-0.0732830357306725,-1.,-2.19213712013662));
#28769=CARTESIAN_POINT('Ctrl Pts',(-0.0713863779526154,-1.,-2.19552129484002));
#28770=CARTESIAN_POINT('Ctrl Pts',(-0.070114353632549,-1.,-2.19777582085423));
#28771=CARTESIAN_POINT('Ctrl Pts',(-0.0694764450219581,-1.,-2.19890268624765));
#28772=CARTESIAN_POINT('',(0.0694764450219584,-1.,-2.19890268624765));
#28773=CARTESIAN_POINT('',(-0.0694764450219581,-1.,-2.19890268624765));
#28774=CARTESIAN_POINT('',(0.163289472382896,-1.,-1.74236521665491));
#28775=CARTESIAN_POINT('Ctrl Pts',(0.0694764450219584,-1.,-2.19890268624765));
#28776=CARTESIAN_POINT('Ctrl Pts',(0.0701143536324926,-1.,-2.19777582085261));
#28777=CARTESIAN_POINT('Ctrl Pts',(0.0713863779524627,-1.,-2.19552129483562));
#28778=CARTESIAN_POINT('Ctrl Pts',(0.0732830357304276,-1.,-2.19213712012956));
#28779=CARTESIAN_POINT('Ctrl Pts',(0.0757891465833411,-1.,-2.1876201139874));
#28780=CARTESIAN_POINT('Ctrl Pts',(0.0788837727683228,-1.,-2.18196589448304));
#28781=CARTESIAN_POINT('Ctrl Pts',(0.0819402680871939,-1.,-2.1763037121106));
#28782=CARTESIAN_POINT('Ctrl Pts',(0.0849584620835643,-1.,-2.17063357871031));
#28783=CARTESIAN_POINT('Ctrl Pts',(0.0879381291387823,-1.,-2.16495552645275));
#28784=CARTESIAN_POINT('Ctrl Pts',(0.0908789888108266,-1.,-2.15926961544808));
#28785=CARTESIAN_POINT('Ctrl Pts',(0.0937807218868345,-1.,-2.15357593978377));
#28786=CARTESIAN_POINT('Ctrl Pts',(0.0966429852305689,-1.,-2.14787463531864));
#28787=CARTESIAN_POINT('Ctrl Pts',(0.0994654261990743,-1.,-2.14216588395974));
#28788=CARTESIAN_POINT('Ctrl Pts',(0.102247700556064,-1.,-2.13644992667052));
#28789=CARTESIAN_POINT('Ctrl Pts',(0.104989479152703,-1.,-2.1307270488718));
#28790=CARTESIAN_POINT('Ctrl Pts',(0.107690435231068,-1.,-2.12499752306927));
#28791=CARTESIAN_POINT('Ctrl Pts',(0.11035023613502,-1.,-2.11926155590849));
#28792=CARTESIAN_POINT('Ctrl Pts',(0.112968534419746,-1.,-2.11351924490335));
#28793=CARTESIAN_POINT('Ctrl Pts',(0.11554495768794,-1.,-2.10777050261359));
#28794=CARTESIAN_POINT('Ctrl Pts',(0.118079107988368,-1.,-2.10201512132945));
#28795=CARTESIAN_POINT('Ctrl Pts',(0.120570567965129,-1.,-2.09625292867756));
#28796=CARTESIAN_POINT('Ctrl Pts',(0.123018905621083,-1.,-2.09048392424826));
#28797=CARTESIAN_POINT('Ctrl Pts',(0.125423679412058,-1.,-2.08470840653628));
#28798=CARTESIAN_POINT('Ctrl Pts',(0.127784445276116,-1.,-2.07892715110967));
#28799=CARTESIAN_POINT('Ctrl Pts',(0.1301007483284,-1.,-2.07314114713047));
#28800=CARTESIAN_POINT('Ctrl Pts',(0.13237211154771,-1.,-2.06735123910319));
#28801=CARTESIAN_POINT('Ctrl Pts',(0.134598026192107,-1.,-2.06155781517844));
#28802=CARTESIAN_POINT('Ctrl Pts',(0.136777941218044,-1.,-2.0557604441427));
#28803=CARTESIAN_POINT('Ctrl Pts',(0.138911255368966,-1.,-2.04995762001333));
#28804=CARTESIAN_POINT('Ctrl Pts',(0.140997332152545,-1.,-2.04414757947919));
#28805=CARTESIAN_POINT('Ctrl Pts',(0.143035515058208,-1.,-2.03832911025913));
#28806=CARTESIAN_POINT('Ctrl Pts',(0.145025140186058,-1.,-2.03250223739941));
#28807=CARTESIAN_POINT('Ctrl Pts',(0.146965557332586,-1.,-2.02666926182017));
#28808=CARTESIAN_POINT('Ctrl Pts',(0.148856124775343,-1.,-2.02083464969897));
#28809=CARTESIAN_POINT('Ctrl Pts',(0.150696157673084,-1.,-2.01500291940243));
#28810=CARTESIAN_POINT('Ctrl Pts',(0.152484883621452,-1.,-2.00917680318426));
#28811=CARTESIAN_POINT('Ctrl Pts',(0.154221403049719,-1.,-2.00335565310539));
#28812=CARTESIAN_POINT('Ctrl Pts',(0.155904629548774,-1.,-1.99753284771487));
#28813=CARTESIAN_POINT('Ctrl Pts',(0.157533331459215,-1.,-1.99169810931893));
#28814=CARTESIAN_POINT('Ctrl Pts',(0.159106226437288,-1.,-1.98584238283279));
#28815=CARTESIAN_POINT('Ctrl Pts',(0.16062206078461,-1.,-1.97996195437557));
#28816=CARTESIAN_POINT('Ctrl Pts',(0.162079693556302,-1.,-1.97406280235204));
#28817=CARTESIAN_POINT('Ctrl Pts',(0.16347818545776,-1.,-1.96816512678));
#28818=CARTESIAN_POINT('Ctrl Pts',(0.1648165689203,-1.,-1.96229379940174));
#28819=CARTESIAN_POINT('Ctrl Pts',(0.166093592002833,-1.,-1.95646759718755));
#28820=CARTESIAN_POINT('Ctrl Pts',(0.167307501784469,-1.,-1.95069027794286));
#28821=CARTESIAN_POINT('Ctrl Pts',(0.168455741607516,-1.,-1.94493757756879));
#28822=CARTESIAN_POINT('Ctrl Pts',(0.169534904817425,-1.,-1.93915639211497));
#28823=CARTESIAN_POINT('Ctrl Pts',(0.170541253116136,-1.,-1.93329183155455));
#28824=CARTESIAN_POINT('Ctrl Pts',(0.17147119153296,-1.,-1.92731093582));
#28825=CARTESIAN_POINT('Ctrl Pts',(0.172321621259557,-1.,-1.92122334398034));
#28826=CARTESIAN_POINT('Ctrl Pts',(0.173090695383619,-1.,-1.91511429159681));
#28827=CARTESIAN_POINT('Ctrl Pts',(0.173776635257984,-1.,-1.90911693975475));
#28828=CARTESIAN_POINT('Ctrl Pts',(0.174375518661222,-1.,-1.90335253863003));
#28829=CARTESIAN_POINT('Ctrl Pts',(0.174879405091277,-1.,-1.89788101117148));
#28830=CARTESIAN_POINT('Ctrl Pts',(0.175274276190664,-1.,-1.89264630198279));
#28831=CARTESIAN_POINT('Ctrl Pts',(0.175538155840286,-1.,-1.88742606272818));
#28832=CARTESIAN_POINT('Ctrl Pts',(0.175644148889271,-1.,-1.88188663144846));
#28833=CARTESIAN_POINT('Ctrl Pts',(0.175563480746205,-1.,-1.87563767773249));
#28834=CARTESIAN_POINT('Ctrl Pts',(0.175268337590901,-1.,-1.86828349694972));
#28835=CARTESIAN_POINT('Ctrl Pts',(0.174735259276856,-1.,-1.85948367089838));
#28836=CARTESIAN_POINT('Ctrl Pts',(0.173946627589401,-1.,-1.84898113200543));
#28837=CARTESIAN_POINT('Ctrl Pts',(0.17288944289442,-1.,-1.83658380530747));
#28838=CARTESIAN_POINT('Ctrl Pts',(0.171554770207306,-1.,-1.82215766815414));
#28839=CARTESIAN_POINT('Ctrl Pts',(0.169936923908078,-1.,-1.80561530633924));
#28840=CARTESIAN_POINT('Ctrl Pts',(0.16803277280837,-1.,-1.78690649988931));
#28841=CARTESIAN_POINT('Ctrl Pts',(0.166279355148738,-1.,-1.77018771687692));
#28842=CARTESIAN_POINT('Ctrl Pts',(0.164834765708484,-1.,-1.75666056640041));
#28843=CARTESIAN_POINT('Ctrl Pts',(0.163814161002474,-1.,-1.74720349503904));
#28844=CARTESIAN_POINT('Ctrl Pts',(0.163289472382896,-1.,-1.74236521665491));
#28845=CARTESIAN_POINT('',(0.383122945602004,-1.,-1.7075470150345));
#28846=CARTESIAN_POINT('Origin',(0.,-1.,0.));
#28847=CARTESIAN_POINT('',(0.61342227326009,-1.,-2.11275013067528));
#28848=CARTESIAN_POINT('Ctrl Pts',(0.383122945602004,-1.,-1.7075470150345));
#28849=CARTESIAN_POINT('Ctrl Pts',(0.384119047314215,-1.,-1.71231062891398));
#28850=CARTESIAN_POINT('Ctrl Pts',(0.386070790323281,-1.,-1.72162022244582));
#28851=CARTESIAN_POINT('Ctrl Pts',(0.388877023502615,-1.,-1.73493170972829));
#28852=CARTESIAN_POINT('Ctrl Pts',(0.392375812285395,-1.,-1.75137405310193));
#28853=CARTESIAN_POINT('Ctrl Pts',(0.396346196110688,-1.,-1.76975560043442));
#28854=CARTESIAN_POINT('Ctrl Pts',(0.399919403774155,-1.,-1.78598826343754));
#28855=CARTESIAN_POINT('Ctrl Pts',(0.403107976163396,-1.,-1.80012077173238));
#28856=CARTESIAN_POINT('Ctrl Pts',(0.405933518407175,-1.,-1.81223801812013));
#28857=CARTESIAN_POINT('Ctrl Pts',(0.408428948106227,-1.,-1.82247022677562));
#28858=CARTESIAN_POINT('Ctrl Pts',(0.410641256301276,-1.,-1.83100408895047));
#28859=CARTESIAN_POINT('Ctrl Pts',(0.412633125322945,-1.,-1.8380895347617));
#28860=CARTESIAN_POINT('Ctrl Pts',(0.414487438255542,-1.,-1.84405757074218));
#28861=CARTESIAN_POINT('Ctrl Pts',(0.416300022039885,-1.,-1.84929312930314));
#28862=CARTESIAN_POINT('Ctrl Pts',(0.418164129144045,-1.,-1.8541763285645));
#28863=CARTESIAN_POINT('Ctrl Pts',(0.420157287975583,-1.,-1.8590328109667));
#28864=CARTESIAN_POINT('Ctrl Pts',(0.422327307417884,-1.,-1.86408083333863));
#28865=CARTESIAN_POINT('Ctrl Pts',(0.424678177290876,-1.,-1.8693780394412));
#28866=CARTESIAN_POINT('Ctrl Pts',(0.427183828518743,-1.,-1.87486989291334));
#28867=CARTESIAN_POINT('Ctrl Pts',(0.429803062482217,-1.,-1.88044229001779));
#28868=CARTESIAN_POINT('Ctrl Pts',(0.432493038548833,-1.,-1.88596913666828));
#28869=CARTESIAN_POINT('Ctrl Pts',(0.43522566096358,-1.,-1.89136993975585));
#28870=CARTESIAN_POINT('Ctrl Pts',(0.437995003948443,-1.,-1.89663648956549));
#28871=CARTESIAN_POINT('Ctrl Pts',(0.44080783370416,-1.,-1.90180124389137));
#28872=CARTESIAN_POINT('Ctrl Pts',(0.44367755684917,-1.,-1.90691756144906));
#28873=CARTESIAN_POINT('Ctrl Pts',(0.446617343485651,-1.,-1.91203699981095));
#28874=CARTESIAN_POINT('Ctrl Pts',(0.449632260106572,-1.,-1.91718342555717));
#28875=CARTESIAN_POINT('Ctrl Pts',(0.452719478359356,-1.,-1.9223538064847));
#28876=CARTESIAN_POINT('Ctrl Pts',(0.455872005174335,-1.,-1.92753067150461));
#28877=CARTESIAN_POINT('Ctrl Pts',(0.459081234547931,-1.,-1.93269066517936));
#28878=CARTESIAN_POINT('Ctrl Pts',(0.462340031009087,-1.,-1.93781486640834));
#28879=CARTESIAN_POINT('Ctrl Pts',(0.465645462026064,-1.,-1.94289794196205));
#28880=CARTESIAN_POINT('Ctrl Pts',(0.468997482913158,-1.,-1.94794381136524));
#28881=CARTESIAN_POINT('Ctrl Pts',(0.472397672264079,-1.,-1.95296148278136));
#28882=CARTESIAN_POINT('Ctrl Pts',(0.475848034683171,-1.,-1.95796111148175));
#28883=CARTESIAN_POINT('Ctrl Pts',(0.479349583074846,-1.,-1.96294933055938));
#28884=CARTESIAN_POINT('Ctrl Pts',(0.482901662120686,-1.,-1.96792703422358));
#28885=CARTESIAN_POINT('Ctrl Pts',(0.486502692907661,-1.,-1.97289186263272));
#28886=CARTESIAN_POINT('Ctrl Pts',(0.490150627860955,-1.,-1.97783973019229));
#28887=CARTESIAN_POINT('Ctrl Pts',(0.493843476541492,-1.,-1.9827665876182));
#28888=CARTESIAN_POINT('Ctrl Pts',(0.497579909545564,-1.,-1.98767044752929));
#28889=CARTESIAN_POINT('Ctrl Pts',(0.501359287727129,-1.,-1.9925514912615));
#28890=CARTESIAN_POINT('Ctrl Pts',(0.505181361323011,-1.,-1.99741107463567));
#28891=CARTESIAN_POINT('Ctrl Pts',(0.509046069886152,-1.,-2.00225107134733));
#28892=CARTESIAN_POINT('Ctrl Pts',(0.512953306961813,-1.,-2.00707309946955));
#28893=CARTESIAN_POINT('Ctrl Pts',(0.516902681728733,-1.,-2.01187773939257));
#28894=CARTESIAN_POINT('Ctrl Pts',(0.520893590399428,-1.,-2.01666477917306));
#28895=CARTESIAN_POINT('Ctrl Pts',(0.524925318333518,-1.,-2.02143356304712));
#28896=CARTESIAN_POINT('Ctrl Pts',(0.52899712724191,-1.,-2.02618329083289));
#28897=CARTESIAN_POINT('Ctrl Pts',(0.533108355132905,-1.,-2.03091336214401));
#28898=CARTESIAN_POINT('Ctrl Pts',(0.537258489833134,-1.,-2.03562362953993));
#28899=CARTESIAN_POINT('Ctrl Pts',(0.54144712061552,-1.,-2.0403142269048));
#28900=CARTESIAN_POINT('Ctrl Pts',(0.545673903817348,-1.,-2.0449854471456));
#28901=CARTESIAN_POINT('Ctrl Pts',(0.549938525150342,-1.,-2.04963761077974));
#28902=CARTESIAN_POINT('Ctrl Pts',(0.554240657464109,-1.,-2.05427091604482));
#28903=CARTESIAN_POINT('Ctrl Pts',(0.558579940185467,-1.,-2.05888537756571));
#28904=CARTESIAN_POINT('Ctrl Pts',(0.562955993082574,-1.,-2.06348090160697));
#28905=CARTESIAN_POINT('Ctrl Pts',(0.567368421181229,-1.,-2.06805732997383));
#28906=CARTESIAN_POINT('Ctrl Pts',(0.571816823242411,-1.,-2.07261449292758));
#28907=CARTESIAN_POINT('Ctrl Pts',(0.576300797416274,-1.,-2.07715226767361));
#28908=CARTESIAN_POINT('Ctrl Pts',(0.580819952107256,-1.,-2.08167059018138));
#28909=CARTESIAN_POINT('Ctrl Pts',(0.585373918990895,-1.,-2.086169437277));
#28910=CARTESIAN_POINT('Ctrl Pts',(0.589962365403189,-1.,-2.09064881812053));
#28911=CARTESIAN_POINT('Ctrl Pts',(0.594585006052823,-1.,-2.09510876220501));
#28912=CARTESIAN_POINT('Ctrl Pts',(0.599241616422144,-1.,-2.09954930865331));
#28913=CARTESIAN_POINT('Ctrl Pts',(0.603932030738212,-1.,-2.10397049887709));
#28914=CARTESIAN_POINT('Ctrl Pts',(0.607711315456826,-1.,-2.10749199615859));
#28915=CARTESIAN_POINT('Ctrl Pts',(0.610560911691113,-1.,-2.11012443807661));
#28916=CARTESIAN_POINT('Ctrl Pts',(0.61246736556225,-1.,-2.11187554260142));
#28917=CARTESIAN_POINT('Ctrl Pts',(0.61342227326009,-1.,-2.11275013067528));
#28918=CARTESIAN_POINT('',(0.745574324794401,-1.,-2.0698113262342));
#28919=CARTESIAN_POINT('',(0.61342227326009,-1.,-2.11275013067528));
#28920=CARTESIAN_POINT('',(0.693717979106306,-1.,-1.60662857109684));
#28921=CARTESIAN_POINT('Ctrl Pts',(0.745574324794401,-1.,-2.0698113262342));
#28922=CARTESIAN_POINT('Ctrl Pts',(0.74583279137781,-1.,-2.06854248895575));
#28923=CARTESIAN_POINT('Ctrl Pts',(0.746345871542695,-1.,-2.06600523016401));
#28924=CARTESIAN_POINT('Ctrl Pts',(0.747103932785504,-1.,-2.06220058927162));
#28925=CARTESIAN_POINT('Ctrl Pts',(0.748091554181101,-1.,-2.05713023030263));
#28926=CARTESIAN_POINT('Ctrl Pts',(0.749287468663053,-1.,-2.05079645591606));
#28927=CARTESIAN_POINT('Ctrl Pts',(0.750444657874758,-1.,-2.04446689147754));
#28928=CARTESIAN_POINT('Ctrl Pts',(0.751562963361383,-1.,-2.03814160092173));
#28929=CARTESIAN_POINT('Ctrl Pts',(0.752642180488104,-1.,-2.03182068456467));
#28930=CARTESIAN_POINT('Ctrl Pts',(0.753682061113765,-1.,-2.02550428623587));
#28931=CARTESIAN_POINT('Ctrl Pts',(0.75468233072352,-1.,-2.01919259406003));
#28932=CARTESIAN_POINT('Ctrl Pts',(0.7556427049581,-1.,-2.01288584328149));
#28933=CARTESIAN_POINT('Ctrl Pts',(0.756562904646496,-1.,-2.00658431587682));
#28934=CARTESIAN_POINT('Ctrl Pts',(0.757442676862341,-1.,-2.00028834739072));
#28935=CARTESIAN_POINT('Ctrl Pts',(0.758281796766377,-1.,-1.9939983109871));
#28936=CARTESIAN_POINT('Ctrl Pts',(0.759080037802242,-1.,-1.98771456680806));
#28937=CARTESIAN_POINT('Ctrl Pts',(0.759837147452135,-1.,-1.98143741418156));
#28938=CARTESIAN_POINT('Ctrl Pts',(0.760552825409855,-1.,-1.97516705321521));
#28939=CARTESIAN_POINT('Ctrl Pts',(0.761226690483986,-1.,-1.96890351582545));
#28940=CARTESIAN_POINT('Ctrl Pts',(0.761858300014575,-1.,-1.96264672744229));
#28941=CARTESIAN_POINT('Ctrl Pts',(0.762447203806263,-1.,-1.95639665309893));
#28942=CARTESIAN_POINT('Ctrl Pts',(0.762992990878774,-1.,-1.95015342590025));
#28943=CARTESIAN_POINT('Ctrl Pts',(0.76349533353858,-1.,-1.94391746617626));
#28944=CARTESIAN_POINT('Ctrl Pts',(0.763954049121393,-1.,-1.93768964875867));
#28945=CARTESIAN_POINT('Ctrl Pts',(0.764369010673889,-1.,-1.93147105496367));
#28946=CARTESIAN_POINT('Ctrl Pts',(0.764740025488189,-1.,-1.92526263537041));
#28947=CARTESIAN_POINT('Ctrl Pts',(0.765066729667095,-1.,-1.91906491634197));
#28948=CARTESIAN_POINT('Ctrl Pts',(0.765348465884739,-1.,-1.91287765805174));
#28949=CARTESIAN_POINT('Ctrl Pts',(0.765584196937936,-1.,-1.90669961402362));
#28950=CARTESIAN_POINT('Ctrl Pts',(0.765772772593395,-1.,-1.90052930393599));
#28951=CARTESIAN_POINT('Ctrl Pts',(0.765913193856979,-1.,-1.89436577771389));
#28952=CARTESIAN_POINT('Ctrl Pts',(0.76600483706209,-1.,-1.88820926433409));
#28953=CARTESIAN_POINT('Ctrl Pts',(0.766047794851868,-1.,-1.88206215302561));
#28954=CARTESIAN_POINT('Ctrl Pts',(0.766042837036759,-1.,-1.87592888967886));
#28955=CARTESIAN_POINT('Ctrl Pts',(0.765990708546111,-1.,-1.86981398314345));
#28956=CARTESIAN_POINT('Ctrl Pts',(0.765891519092557,-1.,-1.86372027063315));
#28957=CARTESIAN_POINT('Ctrl Pts',(0.765744212909305,-1.,-1.85764741390391));
#28958=CARTESIAN_POINT('Ctrl Pts',(0.765545710619023,-1.,-1.85158945130054));
#28959=CARTESIAN_POINT('Ctrl Pts',(0.765291664861971,-1.,-1.84553698875911));
#28960=CARTESIAN_POINT('Ctrl Pts',(0.764978057881687,-1.,-1.83948181064823));
#28961=CARTESIAN_POINT('Ctrl Pts',(0.764602549687845,-1.,-1.8334207722714));
#28962=CARTESIAN_POINT('Ctrl Pts',(0.764165902606055,-1.,-1.8273599120008));
#28963=CARTESIAN_POINT('Ctrl Pts',(0.763673465462854,-1.,-1.82131873145297));
#28964=CARTESIAN_POINT('Ctrl Pts',(0.763132003836783,-1.,-1.81532118405566));
#28965=CARTESIAN_POINT('Ctrl Pts',(0.762546129464036,-1.,-1.80938551463989));
#28966=CARTESIAN_POINT('Ctrl Pts',(0.761915336443515,-1.,-1.80351583877334));
#28967=CARTESIAN_POINT('Ctrl Pts',(0.761229695230359,-1.,-1.79768986997735));
#28968=CARTESIAN_POINT('Ctrl Pts',(0.760469555880425,-1.,-1.79185815610802));
#28969=CARTESIAN_POINT('Ctrl Pts',(0.759614401109868,-1.,-1.78596964884527));
#28970=CARTESIAN_POINT('Ctrl Pts',(0.75865062667738,-1.,-1.77999411220912));
#28971=CARTESIAN_POINT('Ctrl Pts',(0.757578264077238,-1.,-1.77394167108342));
#28972=CARTESIAN_POINT('Ctrl Pts',(0.756421896028403,-1.,-1.76789396003141));
#28973=CARTESIAN_POINT('Ctrl Pts',(0.755220979975262,-1.,-1.7619781724032));
#28974=CARTESIAN_POINT('Ctrl Pts',(0.75400925402848,-1.,-1.75631083600175));
#28975=CARTESIAN_POINT('Ctrl Pts',(0.752797683531377,-1.,-1.75095139468809));
#28976=CARTESIAN_POINT('Ctrl Pts',(0.751555614163629,-1.,-1.74585086852298));
#28977=CARTESIAN_POINT('Ctrl Pts',(0.75019343597954,-1.,-1.74080458266705));
#28978=CARTESIAN_POINT('Ctrl Pts',(0.748582462954854,-1.,-1.73550351679848));
#28979=CARTESIAN_POINT('Ctrl Pts',(0.746574710096436,-1.,-1.72958533647399));
#28980=CARTESIAN_POINT('Ctrl Pts',(0.744021445433764,-1.,-1.7226822991693));
#28981=CARTESIAN_POINT('Ctrl Pts',(0.740795162032087,-1.,-1.71447789751927));
#28982=CARTESIAN_POINT('Ctrl Pts',(0.736799665724771,-1.,-1.70473309006121));
#28983=CARTESIAN_POINT('Ctrl Pts',(0.731963238697195,-1.,-1.69326921975743));
#28984=CARTESIAN_POINT('Ctrl Pts',(0.726235967997433,-1.,-1.67996158455503));
#28985=CARTESIAN_POINT('Ctrl Pts',(0.719585433804282,-1.,-1.6647288055568));
#28986=CARTESIAN_POINT('Ctrl Pts',(0.711993139355394,-1.,-1.64752408832016));
#28987=CARTESIAN_POINT('Ctrl Pts',(0.705159151988319,-1.,-1.63216541664676));
#28988=CARTESIAN_POINT('Ctrl Pts',(0.699605146405088,-1.,-1.61974673472612));
#28989=CARTESIAN_POINT('Ctrl Pts',(0.695712097881194,-1.,-1.61106790958151));
#28990=CARTESIAN_POINT('Ctrl Pts',(0.693717979106306,-1.,-1.60662857109684));
#28991=CARTESIAN_POINT('',(0.892032620296855,-1.,-1.5055822144029));
#28992=CARTESIAN_POINT('Origin',(0.,-1.,0.));
#28993=CARTESIAN_POINT('',(1.23627494547115,-1.,-1.81978687191668));
#28994=CARTESIAN_POINT('Ctrl Pts',(0.892032620296855,-1.,-1.5055822144029));
#28995=CARTESIAN_POINT('Ctrl Pts',(0.894452006964543,-1.,-1.50980486806688));
#28996=CARTESIAN_POINT('Ctrl Pts',(0.89918504748351,-1.,-1.51805569590094));
#28997=CARTESIAN_POINT('Ctrl Pts',(0.905967409625651,-1.,-1.52984849887993));
#28998=CARTESIAN_POINT('Ctrl Pts',(0.914375919026456,-1.,-1.54440491149498));
#28999=CARTESIAN_POINT('Ctrl Pts',(0.923832188944341,-1.,-1.56065988578893));
#29000=CARTESIAN_POINT('Ctrl Pts',(0.932246680108685,-1.,-1.57499388382243));
#29001=CARTESIAN_POINT('Ctrl Pts',(0.939646377893399,-1.,-1.58744937487176));
#29002=CARTESIAN_POINT('Ctrl Pts',(0.946078063315257,-1.,-1.59810042043673));
#29003=CARTESIAN_POINT('Ctrl Pts',(0.951613284356035,-1.,-1.60706069896936));
#29004=CARTESIAN_POINT('Ctrl Pts',(0.95635442292067,-1.,-1.61449324337085));
#29005=CARTESIAN_POINT('Ctrl Pts',(0.960438326101728,-1.,-1.62061638140221));
#29006=CARTESIAN_POINT('Ctrl Pts',(0.964046107040535,-1.,-1.62571930670187));
#29007=CARTESIAN_POINT('Ctrl Pts',(0.967387853230345,-1.,-1.63013849959462));
#29008=CARTESIAN_POINT('Ctrl Pts',(0.970669715997509,-1.,-1.63420665729798));
#29009=CARTESIAN_POINT('Ctrl Pts',(0.974066058287418,-1.,-1.63820952658144));
#29010=CARTESIAN_POINT('Ctrl Pts',(0.977689794119416,-1.,-1.64233990826687));
#29011=CARTESIAN_POINT('Ctrl Pts',(0.981562530939489,-1.,-1.64665139190656));
#29012=CARTESIAN_POINT('Ctrl Pts',(0.98564262292082,-1.,-1.65110016612638));
#29013=CARTESIAN_POINT('Ctrl Pts',(0.989855627854164,-1.,-1.65559044289699));
#29014=CARTESIAN_POINT('Ctrl Pts',(0.994121836661305,-1.,-1.66001553809947));
#29015=CARTESIAN_POINT('Ctrl Pts',(0.998389654952757,-1.,-1.66430758030376));
#29016=CARTESIAN_POINT('Ctrl Pts',(1.00265091003727,-1.,-1.66846059277303));
#29017=CARTESIAN_POINT('Ctrl Pts',(1.00692206696414,-1.,-1.67250335383293));
#29018=CARTESIAN_POINT('Ctrl Pts',(1.01123236493511,-1.,-1.67648246776464));
#29019=CARTESIAN_POINT('Ctrl Pts',(1.01561026162773,-1.,-1.68044289894798));
#29020=CARTESIAN_POINT('Ctrl Pts',(1.02006795074201,-1.,-1.68440578021706));
#29021=CARTESIAN_POINT('Ctrl Pts',(1.02460180535255,-1.,-1.68836910178447));
#29022=CARTESIAN_POINT('Ctrl Pts',(1.02919977579147,-1.,-1.69231840863458));
#29023=CARTESIAN_POINT('Ctrl Pts',(1.03384646003588,-1.,-1.69623414782771));
#29024=CARTESIAN_POINT('Ctrl Pts',(1.03852922490789,-1.,-1.70010052930962));
#29025=CARTESIAN_POINT('Ctrl Pts',(1.04324363334554,-1.,-1.70391338707982));
#29026=CARTESIAN_POINT('Ctrl Pts',(1.04799085404995,-1.,-1.70767646263649));
#29027=CARTESIAN_POINT('Ctrl Pts',(1.05277517202855,-1.,-1.71139783543989));
#29028=CARTESIAN_POINT('Ctrl Pts',(1.05760163192479,-1.,-1.7150865442702));
#29029=CARTESIAN_POINT('Ctrl Pts',(1.06247324680647,-1.,-1.71874858456904));
#29030=CARTESIAN_POINT('Ctrl Pts',(1.06738966975462,-1.,-1.72238500928453));
#29031=CARTESIAN_POINT('Ctrl Pts',(1.07234866990252,-1.,-1.72599406198488));
#29032=CARTESIAN_POINT('Ctrl Pts',(1.0773470373727,-1.,-1.72957248977424));
#29033=CARTESIAN_POINT('Ctrl Pts',(1.08238162784749,-1.,-1.73311705663407));
#29034=CARTESIAN_POINT('Ctrl Pts',(1.08745056285427,-1.,-1.73662628326091));
#29035=CARTESIAN_POINT('Ctrl Pts',(1.09255329056493,-1.,-1.74010053962247));
#29036=CARTESIAN_POINT('Ctrl Pts',(1.09768999241225,-1.,-1.74354119236208));
#29037=CARTESIAN_POINT('Ctrl Pts',(1.10286118991143,-1.,-1.74695004214923));
#29038=CARTESIAN_POINT('Ctrl Pts',(1.10806728183007,-1.,-1.7503286607592));
#29039=CARTESIAN_POINT('Ctrl Pts',(1.11330807582551,-1.,-1.7536777209463));
#29040=CARTESIAN_POINT('Ctrl Pts',(1.11858293216763,-1.,-1.75699720772105));
#29041=CARTESIAN_POINT('Ctrl Pts',(1.12389096855086,-1.,-1.76028671825096));
#29042=CARTESIAN_POINT('Ctrl Pts',(1.12923123555075,-1.,-1.7635457196617));
#29043=CARTESIAN_POINT('Ctrl Pts',(1.1346029180462,-1.,-1.76677384551862));
#29044=CARTESIAN_POINT('Ctrl Pts',(1.14000548336975,-1.,-1.76997111386769));
#29045=CARTESIAN_POINT('Ctrl Pts',(1.1454385822692,-1.,-1.77313777896194));
#29046=CARTESIAN_POINT('Ctrl Pts',(1.15090197841514,-1.,-1.7762742255701));
#29047=CARTESIAN_POINT('Ctrl Pts',(1.15639547194698,-1.,-1.77938085564275));
#29048=CARTESIAN_POINT('Ctrl Pts',(1.16191881298499,-1.,-1.78245795881009));
#29049=CARTESIAN_POINT('Ctrl Pts',(1.16747166312303,-1.,-1.78550566040443));
#29050=CARTESIAN_POINT('Ctrl Pts',(1.17305363177328,-1.,-1.78852398877617));
#29051=CARTESIAN_POINT('Ctrl Pts',(1.17866429440809,-1.,-1.79151291552689));
#29052=CARTESIAN_POINT('Ctrl Pts',(1.18430321697432,-1.,-1.79447240321515));
#29053=CARTESIAN_POINT('Ctrl Pts',(1.18996997934445,-1.,-1.79740245923478));
#29054=CARTESIAN_POINT('Ctrl Pts',(1.19566418930242,-1.,-1.80030314369879));
#29055=CARTESIAN_POINT('Ctrl Pts',(1.20138548938974,-1.,-1.80317454838603));
#29056=CARTESIAN_POINT('Ctrl Pts',(1.20713356605475,-1.,-1.80601678480707));
#29057=CARTESIAN_POINT('Ctrl Pts',(1.21290815708314,-1.,-1.80882996917129));
#29058=CARTESIAN_POINT('Ctrl Pts',(1.21870906103557,-1.,-1.81161420806656));
#29059=CARTESIAN_POINT('Ctrl Pts',(1.2245361330495,-1.,-1.81436959210434));
#29060=CARTESIAN_POINT('Ctrl Pts',(1.2292186489137,-1.,-1.8165508718364));
#29061=CARTESIAN_POINT('Ctrl Pts',(1.2327422452705,-1.,-1.81817389921279));
#29062=CARTESIAN_POINT('Ctrl Pts',(1.23509651170476,-1.,-1.81925017193666));
#29063=CARTESIAN_POINT('Ctrl Pts',(1.23627494547115,-1.,-1.81978687191668));
#29064=CARTESIAN_POINT('',(1.34869019493419,-1.,-1.73811241238545));
#29065=CARTESIAN_POINT('',(1.23627494547115,-1.,-1.81978687191668));
#29066=CARTESIAN_POINT('',(1.15624053661742,-1.,-1.31362392696032));
#29067=CARTESIAN_POINT('Ctrl Pts',(1.34869019493419,-1.,-1.73811241238545));
#29068=CARTESIAN_POINT('Ctrl Pts',(1.34854391898045,-1.,-1.73682580585691));
#29069=CARTESIAN_POINT('Ctrl Pts',(1.34824783112887,-1.,-1.73425417885907));
#29070=CARTESIAN_POINT('Ctrl Pts',(1.34779309152035,-1.,-1.7304014965394));
#29071=CARTESIAN_POINT('Ctrl Pts',(1.34716554819527,-1.,-1.72527410680674));
#29072=CARTESIAN_POINT('Ctrl Pts',(1.34634568653227,-1.,-1.7188807715049));
#29073=CARTESIAN_POINT('Ctrl Pts',(1.34549029589416,-1.,-1.71250340686822));
#29074=CARTESIAN_POINT('Ctrl Pts',(1.34459924533831,-1.,-1.70614212266738));
#29075=CARTESIAN_POINT('Ctrl Pts',(1.34367237124483,-1.,-1.69979707754427));
#29076=CARTESIAN_POINT('Ctrl Pts',(1.34270948206319,-1.,-1.6934684849687));
#29077=CARTESIAN_POINT('Ctrl Pts',(1.341710374848,-1.,-1.68715660868764));
#29078=CARTESIAN_POINT('Ctrl Pts',(1.34067485185203,-1.,-1.68086176030362));
#29079=CARTESIAN_POINT('Ctrl Pts',(1.3396027347034,-1.,-1.67458429426086));
#29080=CARTESIAN_POINT('Ctrl Pts',(1.33849388654388,-1.,-1.66832460783989));
#29081=CARTESIAN_POINT('Ctrl Pts',(1.33734820885262,-1.,-1.66208312541983));
#29082=CARTESIAN_POINT('Ctrl Pts',(1.33616559745172,-1.,-1.65586025952593));
#29083=CARTESIAN_POINT('Ctrl Pts',(1.33494590467993,-1.,-1.6496563728683));
#29084=CARTESIAN_POINT('Ctrl Pts',(1.33368890676572,-1.,-1.6434717485603));
#29085=CARTESIAN_POINT('Ctrl Pts',(1.33239425103724,-1.,-1.63730653475089));
#29086=CARTESIAN_POINT('Ctrl Pts',(1.33106149345645,-1.,-1.63116079730923));
#29087=CARTESIAN_POINT('Ctrl Pts',(1.3296901950568,-1.,-1.62503464209797));
#29088=CARTESIAN_POINT('Ctrl Pts',(1.32828000610449,-1.,-1.61892832270724));
#29089=CARTESIAN_POINT('Ctrl Pts',(1.32683074483356,-1.,-1.6128423401575));
#29090=CARTESIAN_POINT('Ctrl Pts',(1.32534250785782,-1.,-1.60677758290954));
#29091=CARTESIAN_POINT('Ctrl Pts',(1.32381550858256,-1.,-1.60073511858687));
#29092=CARTESIAN_POINT('Ctrl Pts',(1.32224985747682,-1.,-1.59471591079403));
#29093=CARTESIAN_POINT('Ctrl Pts',(1.32064537110892,-1.,-1.58872057258245));
#29094=CARTESIAN_POINT('Ctrl Pts',(1.31900135021432,-1.,-1.58274907898834));
#29095=CARTESIAN_POINT('Ctrl Pts',(1.31731642317187,-1.,-1.5768005650559));
#29096=CARTESIAN_POINT('Ctrl Pts',(1.31558903860016,-1.,-1.57087397835723));
#29097=CARTESIAN_POINT('Ctrl Pts',(1.31381795281002,-1.,-1.56496872402353));
#29098=CARTESIAN_POINT('Ctrl Pts',(1.31200264341696,-1.,-1.55908521254821));
#29099=CARTESIAN_POINT('Ctrl Pts',(1.31014393684222,-1.,-1.55322568759481));
#29100=CARTESIAN_POINT('Ctrl Pts',(1.30824393907473,-1.,-1.54739413957185));
#29101=CARTESIAN_POINT('Ctrl Pts',(1.30630475189556,-1.,-1.54159462645432));
#29102=CARTESIAN_POINT('Ctrl Pts',(1.30432735639489,-1.,-1.53582981268977));
#29103=CARTESIAN_POINT('Ctrl Pts',(1.30231064395568,-1.,-1.53009970283891));
#29104=CARTESIAN_POINT('Ctrl Pts',(1.30024984366328,-1.,-1.52439957861062));
#29105=CARTESIAN_POINT('Ctrl Pts',(1.29813791800747,-1.,-1.51872184912724));
#29106=CARTESIAN_POINT('Ctrl Pts',(1.29596850710509,-1.,-1.51305994241402));
#29107=CARTESIAN_POINT('Ctrl Pts',(1.29373841372842,-1.,-1.50741159078365));
#29108=CARTESIAN_POINT('Ctrl Pts',(1.29145022885181,-1.,-1.50178230149776));
#29109=CARTESIAN_POINT('Ctrl Pts',(1.28911506584254,-1.,-1.49618896881754));
#29110=CARTESIAN_POINT('Ctrl Pts',(1.2867467611644,-1.,-1.4906522831278));
#29111=CARTESIAN_POINT('Ctrl Pts',(1.28435533880201,-1.,-1.4851881711891));
#29112=CARTESIAN_POINT('Ctrl Pts',(1.28194158939517,-1.,-1.47980070347096));
#29113=CARTESIAN_POINT('Ctrl Pts',(1.2794891824849,-1.,-1.4744717526707));
#29114=CARTESIAN_POINT('Ctrl Pts',(1.27696414831089,-1.,-1.46916035917133));
#29115=CARTESIAN_POINT('Ctrl Pts',(1.27433119897822,-1.,-1.46382431332476));
#29116=CARTESIAN_POINT('Ctrl Pts',(1.27156805265289,-1.,-1.45843906294697));
#29117=CARTESIAN_POINT('Ctrl Pts',(1.2686778680489,-1.,-1.45301422764247));
#29118=CARTESIAN_POINT('Ctrl Pts',(1.26570925118868,-1.,-1.44761985001662));
#29119=CARTESIAN_POINT('Ctrl Pts',(1.26273903323858,-1.,-1.44236470511303));
#29120=CARTESIAN_POINT('Ctrl Pts',(1.25983531012005,-1.,-1.43734919180848));
#29121=CARTESIAN_POINT('Ctrl Pts',(1.25702687965755,-1.,-1.43262645609691));
#29122=CARTESIAN_POINT('Ctrl Pts',(1.25426945222639,-1.,-1.42815938799387));
#29123=CARTESIAN_POINT('Ctrl Pts',(1.2514145557001,-1.,-1.42378102115575));
#29124=CARTESIAN_POINT('Ctrl Pts',(1.24824430986571,-1.,-1.41923722596025));
#29125=CARTESIAN_POINT('Ctrl Pts',(1.24450600513056,-1.,-1.41422913175179));
#29126=CARTESIAN_POINT('Ctrl Pts',(1.23994455029534,-1.,-1.40845295531283));
#29127=CARTESIAN_POINT('Ctrl Pts',(1.23434087290423,-1.,-1.40164708206106));
#29128=CARTESIAN_POINT('Ctrl Pts',(1.22752961899387,-1.,-1.39361389568796));
#29129=CARTESIAN_POINT('Ctrl Pts',(1.21938737280852,-1.,-1.38420564527715));
#29130=CARTESIAN_POINT('Ctrl Pts',(1.20982812925645,-1.,-1.37331915607905));
#29131=CARTESIAN_POINT('Ctrl Pts',(1.1987959077932,-1.,-1.36088705043885));
#29132=CARTESIAN_POINT('Ctrl Pts',(1.18625865667441,-1.,-1.34687054001093));
#29133=CARTESIAN_POINT('Ctrl Pts',(1.17501305789857,-1.,-1.33437539347008));
#29134=CARTESIAN_POINT('Ctrl Pts',(1.16589330093588,-1.,-1.32428080721772));
#29135=CARTESIAN_POINT('Ctrl Pts',(1.15950888730809,-1.,-1.31722977216397));
#29136=CARTESIAN_POINT('Ctrl Pts',(1.15624053661742,-1.,-1.31362392696032));
#29137=CARTESIAN_POINT('',(1.31362392696032,-1.,-1.15624053661742));
#29138=CARTESIAN_POINT('Origin',(0.,-1.,0.));
#29139=CARTESIAN_POINT('',(1.73811241238545,-1.,-1.34869019493419));
#29140=CARTESIAN_POINT('Ctrl Pts',(1.31362392696032,-1.,-1.15624053661742));
#29141=CARTESIAN_POINT('Ctrl Pts',(1.3172297721596,-1.,-1.15950888730433));
#29142=CARTESIAN_POINT('Ctrl Pts',(1.32428080720544,-1.,-1.16589330092532));
#29143=CARTESIAN_POINT('Ctrl Pts',(1.33437539344842,-1.,-1.17501305787994));
#29144=CARTESIAN_POINT('Ctrl Pts',(1.34687053998157,-1.,-1.18625865664915));
#29145=CARTESIAN_POINT('Ctrl Pts',(1.36088705040677,-1.,-1.1987959077656));
#29146=CARTESIAN_POINT('Ctrl Pts',(1.37331915604962,-1.,-1.20982812923113));
#29147=CARTESIAN_POINT('Ctrl Pts',(1.38420564525391,-1.,-1.21938737278853));
#29148=CARTESIAN_POINT('Ctrl Pts',(1.39361389567257,-1.,-1.22752961898063));
#29149=CARTESIAN_POINT('Ctrl Pts',(1.40164708205345,-1.,-1.23434087289768));
#29150=CARTESIAN_POINT('Ctrl Pts',(1.40845295531151,-1.,-1.23994455029421));
#29151=CARTESIAN_POINT('Ctrl Pts',(1.41422913175437,-1.,-1.24450600513278));
#29152=CARTESIAN_POINT('Ctrl Pts',(1.41923722596421,-1.,-1.24824430986911));
#29153=CARTESIAN_POINT('Ctrl Pts',(1.42378102115911,-1.,-1.25141455570299));
#29154=CARTESIAN_POINT('Ctrl Pts',(1.42815938799555,-1.,-1.25426945222783));
#29155=CARTESIAN_POINT('Ctrl Pts',(1.43262645609679,-1.,-1.25702687965744));
#29156=CARTESIAN_POINT('Ctrl Pts',(1.43734919180719,-1.,-1.25983531011894));
#29157=CARTESIAN_POINT('Ctrl Pts',(1.44236470511145,-1.,-1.26273903323723));
#29158=CARTESIAN_POINT('Ctrl Pts',(1.44761985001544,-1.,-1.26570925118767));
#29159=CARTESIAN_POINT('Ctrl Pts',(1.45301422764205,-1.,-1.26867786804854));
#29160=CARTESIAN_POINT('Ctrl Pts',(1.45843906294725,-1.,-1.27156805265312));
#29161=CARTESIAN_POINT('Ctrl Pts',(1.4638243133254,-1.,-1.27433119897877));
#29162=CARTESIAN_POINT('Ctrl Pts',(1.46916035917197,-1.,-1.27696414831144));
#29163=CARTESIAN_POINT('Ctrl Pts',(1.4744717526711,-1.,-1.27948918248524));
#29164=CARTESIAN_POINT('Ctrl Pts',(1.47980070347102,-1.,-1.28194158939522));
#29165=CARTESIAN_POINT('Ctrl Pts',(1.48518817118891,-1.,-1.28435533880184));
#29166=CARTESIAN_POINT('Ctrl Pts',(1.4906522831275,-1.,-1.28674676116415));
#29167=CARTESIAN_POINT('Ctrl Pts',(1.49618896881729,-1.,-1.28911506584232));
#29168=CARTESIAN_POINT('Ctrl Pts',(1.50178230149764,-1.,-1.29145022885171));
#29169=CARTESIAN_POINT('Ctrl Pts',(1.50741159078367,-1.,-1.29373841372843));
#29170=CARTESIAN_POINT('Ctrl Pts',(1.51305994241412,-1.,-1.29596850710518));
#29171=CARTESIAN_POINT('Ctrl Pts',(1.51872184912735,-1.,-1.29813791800757));
#29172=CARTESIAN_POINT('Ctrl Pts',(1.5243995786107,-1.,-1.30024984366334));
#29173=CARTESIAN_POINT('Ctrl Pts',(1.53009970283893,-1.,-1.3023106439557));
#29174=CARTESIAN_POINT('Ctrl Pts',(1.53582981268976,-1.,-1.30432735639487));
#29175=CARTESIAN_POINT('Ctrl Pts',(1.54159462645428,-1.,-1.30630475189553));
#29176=CARTESIAN_POINT('Ctrl Pts',(1.54739413957183,-1.,-1.30824393907471));
#29177=CARTESIAN_POINT('Ctrl Pts',(1.55322568759481,-1.,-1.31014393684221));
#29178=CARTESIAN_POINT('Ctrl Pts',(1.55908521254822,-1.,-1.31200264341696));
#29179=CARTESIAN_POINT('Ctrl Pts',(1.56496872402352,-1.,-1.31381795281002));
#29180=CARTESIAN_POINT('Ctrl Pts',(1.57087397835721,-1.,-1.31558903860015));
#29181=CARTESIAN_POINT('Ctrl Pts',(1.57680056505585,-1.,-1.31731642317183));
#29182=CARTESIAN_POINT('Ctrl Pts',(1.58274907898829,-1.,-1.31900135021428));
#29183=CARTESIAN_POINT('Ctrl Pts',(1.58872057258244,-1.,-1.32064537110891));
#29184=CARTESIAN_POINT('Ctrl Pts',(1.59471591079408,-1.,-1.32224985747686));
#29185=CARTESIAN_POINT('Ctrl Pts',(1.600735118587,-1.,-1.32381550858266));
#29186=CARTESIAN_POINT('Ctrl Pts',(1.6067775829097,-1.,-1.32534250785794));
#29187=CARTESIAN_POINT('Ctrl Pts',(1.61284234015762,-1.,-1.32683074483365));
#29188=CARTESIAN_POINT('Ctrl Pts',(1.61892832270723,-1.,-1.32828000610448));
#29189=CARTESIAN_POINT('Ctrl Pts',(1.62503464209777,-1.,-1.32969019505665));
#29190=CARTESIAN_POINT('Ctrl Pts',(1.63116079730887,-1.,-1.33106149345618));
#29191=CARTESIAN_POINT('Ctrl Pts',(1.63730653475049,-1.,-1.33239425103694));
#29192=CARTESIAN_POINT('Ctrl Pts',(1.64347174856007,-1.,-1.33368890676554));
#29193=CARTESIAN_POINT('Ctrl Pts',(1.64965637286843,-1.,-1.33494590468003));
#29194=CARTESIAN_POINT('Ctrl Pts',(1.65586025952651,-1.,-1.33616559745217));
#29195=CARTESIAN_POINT('Ctrl Pts',(1.66208312542073,-1.,-1.33734820885331));
#29196=CARTESIAN_POINT('Ctrl Pts',(1.66832460784078,-1.,-1.33849388654458));
#29197=CARTESIAN_POINT('Ctrl Pts',(1.67458429426126,-1.,-1.33960273470372));
#29198=CARTESIAN_POINT('Ctrl Pts',(1.68086176030308,-1.,-1.3406748518516));
#29199=CARTESIAN_POINT('Ctrl Pts',(1.68715660868602,-1.,-1.34171037484673));
#29200=CARTESIAN_POINT('Ctrl Pts',(1.6934684849664,-1.,-1.34270948206139));
#29201=CARTESIAN_POINT('Ctrl Pts',(1.69979707754221,-1.,-1.34367237124322));
#29202=CARTESIAN_POINT('Ctrl Pts',(1.70614212266676,-1.,-1.34459924533783));
#29203=CARTESIAN_POINT('Ctrl Pts',(1.71250340687011,-1.,-1.34549029589563));
#29204=CARTESIAN_POINT('Ctrl Pts',(1.7188807715095,-1.,-1.34634568653586));
#29205=CARTESIAN_POINT('Ctrl Pts',(1.72527410681298,-1.,-1.34716554820013));
#29206=CARTESIAN_POINT('Ctrl Pts',(1.73040149654497,-1.,-1.3477930915247));
#29207=CARTESIAN_POINT('Ctrl Pts',(1.73425417886254,-1.,-1.34824783113158));
#29208=CARTESIAN_POINT('Ctrl Pts',(1.73682580585819,-1.,-1.34854391898145));
#29209=CARTESIAN_POINT('Ctrl Pts',(1.73811241238545,-1.,-1.34869019493419));
#29210=CARTESIAN_POINT('',(1.81978687191668,-1.,-1.23627494547115));
#29211=CARTESIAN_POINT('',(1.73811241238545,-1.,-1.34869019493419));
#29212=CARTESIAN_POINT('',(1.5055822144029,-1.,-0.892032620296855));
#29213=CARTESIAN_POINT('Ctrl Pts',(1.81978687191668,-1.,-1.23627494547115));
#29214=CARTESIAN_POINT('Ctrl Pts',(1.81925017193531,-1.,-1.23509651170384));
#29215=CARTESIAN_POINT('Ctrl Pts',(1.81817389920914,-1.,-1.23274224526804));
#29216=CARTESIAN_POINT('Ctrl Pts',(1.81655087183054,-1.,-1.22921864890975));
#29217=CARTESIAN_POINT('Ctrl Pts',(1.81436959209778,-1.,-1.22453613304507));
#29218=CARTESIAN_POINT('Ctrl Pts',(1.81161420806172,-1.,-1.2187090610323));
#29219=CARTESIAN_POINT('Ctrl Pts',(1.80882996916931,-1.,-1.2129081570818));
#29220=CARTESIAN_POINT('Ctrl Pts',(1.80601678480772,-1.,-1.20713356605519));
#29221=CARTESIAN_POINT('Ctrl Pts',(1.8031745483882,-1.,-1.2013854893912));
#29222=CARTESIAN_POINT('Ctrl Pts',(1.80030314370121,-1.,-1.19566418930405));
#29223=CARTESIAN_POINT('Ctrl Pts',(1.79740245923649,-1.,-1.1899699793456));
#29224=CARTESIAN_POINT('Ctrl Pts',(1.79447240321572,-1.,-1.18430321697471));
#29225=CARTESIAN_POINT('Ctrl Pts',(1.79151291552646,-1.,-1.17866429440781));
#29226=CARTESIAN_POINT('Ctrl Pts',(1.78852398877523,-1.,-1.17305363177265));
#29227=CARTESIAN_POINT('Ctrl Pts',(1.78550566040349,-1.,-1.16747166312239));
#29228=CARTESIAN_POINT('Ctrl Pts',(1.78245795880949,-1.,-1.16191881298458));
#29229=CARTESIAN_POINT('Ctrl Pts',(1.77938085564261,-1.,-1.15639547194689));
#29230=CARTESIAN_POINT('Ctrl Pts',(1.77627422557034,-1.,-1.15090197841531));
#29231=CARTESIAN_POINT('Ctrl Pts',(1.77313777896234,-1.,-1.14543858226948));
#29232=CARTESIAN_POINT('Ctrl Pts',(1.76997111386806,-1.,-1.14000548337));
#29233=CARTESIAN_POINT('Ctrl Pts',(1.76677384551883,-1.,-1.13460291804635));
#29234=CARTESIAN_POINT('Ctrl Pts',(1.76354571966171,-1.,-1.12923123555076));
#29235=CARTESIAN_POINT('Ctrl Pts',(1.76028671825084,-1.,-1.12389096855078));
#29236=CARTESIAN_POINT('Ctrl Pts',(1.75699720772089,-1.,-1.11858293216752));
#29237=CARTESIAN_POINT('Ctrl Pts',(1.75367772094617,-1.,-1.11330807582542));
#29238=CARTESIAN_POINT('Ctrl Pts',(1.75032866075914,-1.,-1.10806728183003));
#29239=CARTESIAN_POINT('Ctrl Pts',(1.74695004214924,-1.,-1.10286118991144));
#29240=CARTESIAN_POINT('Ctrl Pts',(1.74354119236212,-1.,-1.09768999241229));
#29241=CARTESIAN_POINT('Ctrl Pts',(1.74010053962252,-1.,-1.09255329056496));
#29242=CARTESIAN_POINT('Ctrl Pts',(1.73662628326093,-1.,-1.08745056285429));
#29243=CARTESIAN_POINT('Ctrl Pts',(1.73311705663407,-1.,-1.08238162784749));
#29244=CARTESIAN_POINT('Ctrl Pts',(1.72957248977424,-1.,-1.0773470373727));
#29245=CARTESIAN_POINT('Ctrl Pts',(1.72599406198489,-1.,-1.07234866990252));
#29246=CARTESIAN_POINT('Ctrl Pts',(1.72238500928456,-1.,-1.06738966975463));
#29247=CARTESIAN_POINT('Ctrl Pts',(1.71874858456908,-1.,-1.0624732468065));
#29248=CARTESIAN_POINT('Ctrl Pts',(1.71508654427022,-1.,-1.05760163192481));
#29249=CARTESIAN_POINT('Ctrl Pts',(1.71139783543986,-1.,-1.05277517202854));
#29250=CARTESIAN_POINT('Ctrl Pts',(1.70767646263641,-1.,-1.0479908540499));
#29251=CARTESIAN_POINT('Ctrl Pts',(1.70391338707969,-1.,-1.04324363334546));
#29252=CARTESIAN_POINT('Ctrl Pts',(1.70010052930951,-1.,-1.03852922490782));
#29253=CARTESIAN_POINT('Ctrl Pts',(1.69623414782769,-1.,-1.03384646003587));
#29254=CARTESIAN_POINT('Ctrl Pts',(1.69231840863471,-1.,-1.02919977579155));
#29255=CARTESIAN_POINT('Ctrl Pts',(1.68836910178475,-1.,-1.02460180535272));
#29256=CARTESIAN_POINT('Ctrl Pts',(1.68440578021739,-1.,-1.02006795074222));
#29257=CARTESIAN_POINT('Ctrl Pts',(1.6804428989482,-1.,-1.01561026162787));
#29258=CARTESIAN_POINT('Ctrl Pts',(1.67648246776457,-1.,-1.01123236493507));
#29259=CARTESIAN_POINT('Ctrl Pts',(1.67250335383248,-1.,-1.00692206696387));
#29260=CARTESIAN_POINT('Ctrl Pts',(1.66846059277231,-1.,-1.00265091003682));
#29261=CARTESIAN_POINT('Ctrl Pts',(1.66430758030304,-1.,-0.998389654952317));
#29262=CARTESIAN_POINT('Ctrl Pts',(1.66001553809916,-1.,-0.994121836661116));
#29263=CARTESIAN_POINT('Ctrl Pts',(1.65559044289746,-1.,-0.98985562785445));
#29264=CARTESIAN_POINT('Ctrl Pts',(1.6511001661277,-1.,-0.985642622921626));
#29265=CARTESIAN_POINT('Ctrl Pts',(1.64665139190834,-1.,-0.981562530940574));
#29266=CARTESIAN_POINT('Ctrl Pts',(1.64233990826831,-1.,-0.977689794120297));
#29267=CARTESIAN_POINT('Ctrl Pts',(1.63820952658157,-1.,-0.974066058287501));
#29268=CARTESIAN_POINT('Ctrl Pts',(1.63420665729609,-1.,-0.970669715996356));
#29269=CARTESIAN_POINT('Ctrl Pts',(1.63013849959083,-1.,-0.967387853228041));
#29270=CARTESIAN_POINT('Ctrl Pts',(1.6257193066974,-1.,-0.964046107037821));
#29271=CARTESIAN_POINT('Ctrl Pts',(1.62061638139929,-1.,-0.960438326099958));
#29272=CARTESIAN_POINT('Ctrl Pts',(1.61449324337233,-1.,-0.956354422921573));
#29273=CARTESIAN_POINT('Ctrl Pts',(1.60706069897794,-1.,-0.951613284361248));
#29274=CARTESIAN_POINT('Ctrl Pts',(1.59810042045408,-1.,-0.946078063325796));
#29275=CARTESIAN_POINT('Ctrl Pts',(1.58744937489796,-1.,-0.939646377909319));
#29276=CARTESIAN_POINT('Ctrl Pts',(1.57499388385561,-1.,-0.932246680128849));
#29277=CARTESIAN_POINT('Ctrl Pts',(1.56065988582509,-1.,-0.923832188966322));
#29278=CARTESIAN_POINT('Ctrl Pts',(1.54440491152807,-1.,-0.91437591904658));
#29279=CARTESIAN_POINT('Ctrl Pts',(1.52984849890434,-1.,-0.905967409640499));
#29280=CARTESIAN_POINT('Ctrl Pts',(1.51805569591479,-1.,-0.89918504749193));
#29281=CARTESIAN_POINT('Ctrl Pts',(1.50980486807181,-1.,-0.894452006967538));
#29282=CARTESIAN_POINT('Ctrl Pts',(1.5055822144029,-1.,-0.892032620296855));
#29283=CARTESIAN_POINT('',(1.60662857109684,-1.,-0.693717979106306));
#29284=CARTESIAN_POINT('Origin',(0.,-1.,0.));
#29285=CARTESIAN_POINT('',(2.0698113262342,-1.,-0.745574324794401));
#29286=CARTESIAN_POINT('Ctrl Pts',(1.60662857109684,-1.,-0.693717979106306));
#29287=CARTESIAN_POINT('Ctrl Pts',(1.61106790957619,-1.,-0.69571209787897));
#29288=CARTESIAN_POINT('Ctrl Pts',(1.61974673471117,-1.,-0.699605146398837));
#29289=CARTESIAN_POINT('Ctrl Pts',(1.6321654166204,-1.,-0.705159151977294));
#29290=CARTESIAN_POINT('Ctrl Pts',(1.64752408828442,-1.,-0.711993139340448));
#29291=CARTESIAN_POINT('Ctrl Pts',(1.66472880551777,-1.,-0.71958543378795));
#29292=CARTESIAN_POINT('Ctrl Pts',(1.67996158451922,-1.,-0.726235967982445));
#29293=CARTESIAN_POINT('Ctrl Pts',(1.69326921972915,-1.,-0.731963238685357));
#29294=CARTESIAN_POINT('Ctrl Pts',(1.70473309004249,-1.,-0.736799665716932));
#29295=CARTESIAN_POINT('Ctrl Pts',(1.71447789751001,-1.,-0.74079516202821));
#29296=CARTESIAN_POINT('Ctrl Pts',(1.72268229916769,-1.,-0.744021445433094));
#29297=CARTESIAN_POINT('Ctrl Pts',(1.72958533647714,-1.,-0.746574710097752));
#29298=CARTESIAN_POINT('Ctrl Pts',(1.7355035168033,-1.,-0.74858246295687));
#29299=CARTESIAN_POINT('Ctrl Pts',(1.74080458267114,-1.,-0.75019343598125));
#29300=CARTESIAN_POINT('Ctrl Pts',(1.74585086852502,-1.,-0.751555614164483));
#29301=CARTESIAN_POINT('Ctrl Pts',(1.75095139468794,-1.,-0.752797683531314));
#29302=CARTESIAN_POINT('Ctrl Pts',(1.75631083600019,-1.,-0.754009254027829));
#29303=CARTESIAN_POINT('Ctrl Pts',(1.76197817240128,-1.,-0.755220979974462));
#29304=CARTESIAN_POINT('Ctrl Pts',(1.76789396002998,-1.,-0.75642189602781));
#29305=CARTESIAN_POINT('Ctrl Pts',(1.77394167108292,-1.,-0.757578264077029));
#29306=CARTESIAN_POINT('Ctrl Pts',(1.77999411220945,-1.,-0.758650626677519));
#29307=CARTESIAN_POINT('Ctrl Pts',(1.78596964884604,-1.,-0.75961440111019));
#29308=CARTESIAN_POINT('Ctrl Pts',(1.7918581561088,-1.,-0.760469555880749));
#29309=CARTESIAN_POINT('Ctrl Pts',(1.79768986997783,-1.,-0.761229695230558));
#29310=CARTESIAN_POINT('Ctrl Pts',(1.80351583877342,-1.,-0.761915336443547));
#29311=CARTESIAN_POINT('Ctrl Pts',(1.80938551463965,-1.,-0.762546129463938));
#29312=CARTESIAN_POINT('Ctrl Pts',(1.8153211840553,-1.,-0.763132003836634));
#29313=CARTESIAN_POINT('Ctrl Pts',(1.82131873145266,-1.,-0.763673465462727));
#29314=CARTESIAN_POINT('Ctrl Pts',(1.82735991200065,-1.,-0.764165902605995));
#29315=CARTESIAN_POINT('Ctrl Pts',(1.83342077227142,-1.,-0.764602549687853));
#29316=CARTESIAN_POINT('Ctrl Pts',(1.83948181064835,-1.,-0.764978057881738));
#29317=CARTESIAN_POINT('Ctrl Pts',(1.84553698875924,-1.,-0.765291664862029));
#29318=CARTESIAN_POINT('Ctrl Pts',(1.85158945130063,-1.,-0.765545710619063));
#29319=CARTESIAN_POINT('Ctrl Pts',(1.85764741390394,-1.,-0.765744212909319));
#29320=CARTESIAN_POINT('Ctrl Pts',(1.86372027063312,-1.,-0.765891519092547));
#29321=CARTESIAN_POINT('Ctrl Pts',(1.86981398314341,-1.,-0.765990708546091));
#29322=CARTESIAN_POINT('Ctrl Pts',(1.87592888967883,-1.,-0.766042837036744));
#29323=CARTESIAN_POINT('Ctrl Pts',(1.88206215302561,-1.,-0.766047794851865));
#29324=CARTESIAN_POINT('Ctrl Pts',(1.88820926433409,-1.,-0.766004837062091));
#29325=CARTESIAN_POINT('Ctrl Pts',(1.89436577771388,-1.,-0.765913193856978));
#29326=CARTESIAN_POINT('Ctrl Pts',(1.90052930393596,-1.,-0.765772772593386));
#29327=CARTESIAN_POINT('Ctrl Pts',(1.90669961402356,-1.,-0.765584196937919));
#29328=CARTESIAN_POINT('Ctrl Pts',(1.91287765805169,-1.,-0.765348465884722));
#29329=CARTESIAN_POINT('Ctrl Pts',(1.91906491634196,-1.,-0.765066729667089));
#29330=CARTESIAN_POINT('Ctrl Pts',(1.92526263537048,-1.,-0.764740025488212));
#29331=CARTESIAN_POINT('Ctrl Pts',(1.93147105496382,-1.,-0.764369010673941));
#29332=CARTESIAN_POINT('Ctrl Pts',(1.93768964875886,-1.,-0.763954049121459));
#29333=CARTESIAN_POINT('Ctrl Pts',(1.9439174661764,-1.,-0.763495333538629));
#29334=CARTESIAN_POINT('Ctrl Pts',(1.95015342590024,-1.,-0.762992990878769));
#29335=CARTESIAN_POINT('Ctrl Pts',(1.95639665309869,-1.,-0.762447203806179));
#29336=CARTESIAN_POINT('Ctrl Pts',(1.96264672744186,-1.,-0.761858300014424));
#29337=CARTESIAN_POINT('Ctrl Pts',(1.96890351582499,-1.,-0.761226690483821));
#29338=CARTESIAN_POINT('Ctrl Pts',(1.97516705321494,-1.,-0.760552825409757));
#29339=CARTESIAN_POINT('Ctrl Pts',(1.98143741418172,-1.,-0.75983714745219));
#29340=CARTESIAN_POINT('Ctrl Pts',(1.98771456680874,-1.,-0.759080037802488));
#29341=CARTESIAN_POINT('Ctrl Pts',(1.99399831098817,-1.,-0.758281796766761));
#29342=CARTESIAN_POINT('Ctrl Pts',(2.00028834739178,-1.,-0.757442676862724));
#29343=CARTESIAN_POINT('Ctrl Pts',(2.0065843158773,-1.,-0.756562904646671));
#29344=CARTESIAN_POINT('Ctrl Pts',(2.01288584328084,-1.,-0.755642704957865));
#29345=CARTESIAN_POINT('Ctrl Pts',(2.01919259405809,-1.,-0.754682330722816));
#29346=CARTESIAN_POINT('Ctrl Pts',(2.02550428623313,-1.,-0.753682061112768));
#29347=CARTESIAN_POINT('Ctrl Pts',(2.03182068456221,-1.,-0.752642180487211));
#29348=CARTESIAN_POINT('Ctrl Pts',(2.03814160092099,-1.,-0.751562963361115));
#29349=CARTESIAN_POINT('Ctrl Pts',(2.04446689147979,-1.,-0.750444657875576));
#29350=CARTESIAN_POINT('Ctrl Pts',(2.05079645592154,-1.,-0.749287468665046));
#29351=CARTESIAN_POINT('Ctrl Pts',(2.05713023031006,-1.,-0.748091554183803));
#29352=CARTESIAN_POINT('Ctrl Pts',(2.06220058927826,-1.,-0.74710393278792));
#29353=CARTESIAN_POINT('Ctrl Pts',(2.06600523016815,-1.,-0.746345871544201));
#29354=CARTESIAN_POINT('Ctrl Pts',(2.06854248895728,-1.,-0.745832791378367));
#29355=CARTESIAN_POINT('Ctrl Pts',(2.0698113262342,-1.,-0.745574324794401));
#29356=CARTESIAN_POINT('',(2.11275013067528,-1.,-0.61342227326009));
#29357=CARTESIAN_POINT('',(2.0698113262342,-1.,-0.745574324794401));
#29358=CARTESIAN_POINT('',(1.7075470150345,-1.,-0.383122945602004));
#29359=CARTESIAN_POINT('Ctrl Pts',(2.11275013067528,-1.,-0.61342227326009));
#29360=CARTESIAN_POINT('Ctrl Pts',(2.11187554259986,-1.,-0.6124673655618));
#29361=CARTESIAN_POINT('Ctrl Pts',(2.11012443807238,-1.,-0.610560911689899));
#29362=CARTESIAN_POINT('Ctrl Pts',(2.1074919961518,-1.,-0.607711315454876));
#29363=CARTESIAN_POINT('Ctrl Pts',(2.10397049886949,-1.,-0.60393203073603));
#29364=CARTESIAN_POINT('Ctrl Pts',(2.0995493086477,-1.,-0.599241616420534));
#29365=CARTESIAN_POINT('Ctrl Pts',(2.0951087622027,-1.,-0.594585006052162));
#29366=CARTESIAN_POINT('Ctrl Pts',(2.09064881812129,-1.,-0.589962365403406));
#29367=CARTESIAN_POINT('Ctrl Pts',(2.08616943727951,-1.,-0.585373918991617));
#29368=CARTESIAN_POINT('Ctrl Pts',(2.08167059018418,-1.,-0.580819952108064));
#29369=CARTESIAN_POINT('Ctrl Pts',(2.07715226767559,-1.,-0.576300797416845));
#29370=CARTESIAN_POINT('Ctrl Pts',(2.07261449292824,-1.,-0.571816823242603));
#29371=CARTESIAN_POINT('Ctrl Pts',(2.06805732997334,-1.,-0.567368421181087));
#29372=CARTESIAN_POINT('Ctrl Pts',(2.06348090160589,-1.,-0.562955993082262));
#29373=CARTESIAN_POINT('Ctrl Pts',(2.05888537756462,-1.,-0.558579940185152));
#29374=CARTESIAN_POINT('Ctrl Pts',(2.05427091604413,-1.,-0.554240657463906));
#29375=CARTESIAN_POINT('Ctrl Pts',(2.04963761077958,-1.,-0.549938525150295));
#29376=CARTESIAN_POINT('Ctrl Pts',(2.04498544714588,-1.,-0.54567390381743));
#29377=CARTESIAN_POINT('Ctrl Pts',(2.04031422690527,-1.,-0.541447120615659));
#29378=CARTESIAN_POINT('Ctrl Pts',(2.03562362954037,-1.,-0.537258489833262));
#29379=CARTESIAN_POINT('Ctrl Pts',(2.03091336214426,-1.,-0.533108355132977));
#29380=CARTESIAN_POINT('Ctrl Pts',(2.0261832908329,-1.,-0.528997127241914));
#29381=CARTESIAN_POINT('Ctrl Pts',(2.02143356304698,-1.,-0.524925318333476));
#29382=CARTESIAN_POINT('Ctrl Pts',(2.01666477917286,-1.,-0.520893590399371));
#29383=CARTESIAN_POINT('Ctrl Pts',(2.01187773939242,-1.,-0.516902681728687));
#29384=CARTESIAN_POINT('Ctrl Pts',(2.00707309946949,-1.,-0.512953306961793));
#29385=CARTESIAN_POINT('Ctrl Pts',(2.00225107134734,-1.,-0.509046069886157));
#29386=CARTESIAN_POINT('Ctrl Pts',(1.99741107463572,-1.,-0.505181361323026));
#29387=CARTESIAN_POINT('Ctrl Pts',(1.99255149126155,-1.,-0.501359287727146));
#29388=CARTESIAN_POINT('Ctrl Pts',(1.98767044752932,-1.,-0.497579909545574));
#29389=CARTESIAN_POINT('Ctrl Pts',(1.98276658761821,-1.,-0.493843476541495));
#29390=CARTESIAN_POINT('Ctrl Pts',(1.97783973019229,-1.,-0.490150627860953));
#29391=CARTESIAN_POINT('Ctrl Pts',(1.97289186263272,-1.,-0.486502692907659));
#29392=CARTESIAN_POINT('Ctrl Pts',(1.96792703422362,-1.,-0.482901662120691));
#29393=CARTESIAN_POINT('Ctrl Pts',(1.96294933055943,-1.,-0.479349583074855));
#29394=CARTESIAN_POINT('Ctrl Pts',(1.95796111148177,-1.,-0.475848034683176));
#29395=CARTESIAN_POINT('Ctrl Pts',(1.95296148278133,-1.,-0.472397672264072));
#29396=CARTESIAN_POINT('Ctrl Pts',(1.94794381136514,-1.,-0.468997482913135));
#29397=CARTESIAN_POINT('Ctrl Pts',(1.9428979419619,-1.,-0.46564546202603));
#29398=CARTESIAN_POINT('Ctrl Pts',(1.93781486640821,-1.,-0.462340031009057));
#29399=CARTESIAN_POINT('Ctrl Pts',(1.93269066517934,-1.,-0.459081234547926));
#29400=CARTESIAN_POINT('Ctrl Pts',(1.92753067150476,-1.,-0.455872005174371));
#29401=CARTESIAN_POINT('Ctrl Pts',(1.92235380648502,-1.,-0.452719478359433));
#29402=CARTESIAN_POINT('Ctrl Pts',(1.91718342555755,-1.,-0.449632260106662));
#29403=CARTESIAN_POINT('Ctrl Pts',(1.9120369998112,-1.,-0.446617343485711));
#29404=CARTESIAN_POINT('Ctrl Pts',(1.90691756144898,-1.,-0.443677556849151));
#29405=CARTESIAN_POINT('Ctrl Pts',(1.90180124389086,-1.,-0.440807833704038));
#29406=CARTESIAN_POINT('Ctrl Pts',(1.89663648956466,-1.,-0.437995003948244));
#29407=CARTESIAN_POINT('Ctrl Pts',(1.89136993975504,-1.,-0.435225660963383));
#29408=CARTESIAN_POINT('Ctrl Pts',(1.88596913666793,-1.,-0.432493038548748));
#29409=CARTESIAN_POINT('Ctrl Pts',(1.88044229001832,-1.,-0.429803062482345));
#29410=CARTESIAN_POINT('Ctrl Pts',(1.87486989291484,-1.,-0.427183828519102));
#29411=CARTESIAN_POINT('Ctrl Pts',(1.86937803944323,-1.,-0.424678177291359));
#29412=CARTESIAN_POINT('Ctrl Pts',(1.86408083334028,-1.,-0.422327307418275));
#29413=CARTESIAN_POINT('Ctrl Pts',(1.85903281096686,-1.,-0.42015728797562));
#29414=CARTESIAN_POINT('Ctrl Pts',(1.85417632856234,-1.,-0.418164129143534));
#29415=CARTESIAN_POINT('Ctrl Pts',(1.84929312929882,-1.,-0.416300022038864));
#29416=CARTESIAN_POINT('Ctrl Pts',(1.8440575707371,-1.,-0.41448743825434));
#29417=CARTESIAN_POINT('Ctrl Pts',(1.83808953475839,-1.,-0.412633125322162));
#29418=CARTESIAN_POINT('Ctrl Pts',(1.83100408895216,-1.,-0.410641256301675));
#29419=CARTESIAN_POINT('Ctrl Pts',(1.8224702267854,-1.,-0.408428948108534));
#29420=CARTESIAN_POINT('Ctrl Pts',(1.81223801813988,-1.,-0.405933518411838));
#29421=CARTESIAN_POINT('Ctrl Pts',(1.80012077176221,-1.,-0.403107976170441));
#29422=CARTESIAN_POINT('Ctrl Pts',(1.78598826347533,-1.,-0.399919403783081));
#29423=CARTESIAN_POINT('Ctrl Pts',(1.7697556004756,-1.,-0.39634619612042));
#29424=CARTESIAN_POINT('Ctrl Pts',(1.75137405313962,-1.,-0.392375812294307));
#29425=CARTESIAN_POINT('Ctrl Pts',(1.7349317097561,-1.,-0.388877023509192));
#29426=CARTESIAN_POINT('Ctrl Pts',(1.72162022246158,-1.,-0.38607079032701));
#29427=CARTESIAN_POINT('Ctrl Pts',(1.71231062891958,-1.,-0.384119047315542));
#29428=CARTESIAN_POINT('Ctrl Pts',(1.7075470150345,-1.,-0.383122945602004));
#29429=CARTESIAN_POINT('',(1.74236521665491,-1.,-0.163289472382896));
#29430=CARTESIAN_POINT('Origin',(0.,-1.,0.));
#29431=CARTESIAN_POINT('',(2.19890268624765,-1.,-0.0694764450219582));
#29432=CARTESIAN_POINT('Ctrl Pts',(1.74236521665491,-1.,-0.163289472382896));
#29433=CARTESIAN_POINT('Ctrl Pts',(1.7472034950333,-1.,-0.163814161002002));
#29434=CARTESIAN_POINT('Ctrl Pts',(1.75666056638427,-1.,-0.164834765707159));
#29435=CARTESIAN_POINT('Ctrl Pts',(1.77018771684844,-1.,-0.1662793551464));
#29436=CARTESIAN_POINT('Ctrl Pts',(1.7869064998507,-1.,-0.168032772805197));
#29437=CARTESIAN_POINT('Ctrl Pts',(1.80561530629706,-1.,-0.169936923904608));
#29438=CARTESIAN_POINT('Ctrl Pts',(1.82215766811545,-1.,-0.171554770204119));
#29439=CARTESIAN_POINT('Ctrl Pts',(1.83658380527692,-1.,-0.1728894428919));
#29440=CARTESIAN_POINT('Ctrl Pts',(1.8489811319852,-1.,-0.173946627587732));
#29441=CARTESIAN_POINT('Ctrl Pts',(1.85948367088837,-1.,-0.17473525927603));
#29442=CARTESIAN_POINT('Ctrl Pts',(1.86828349694799,-1.,-0.175268337590758));
#29443=CARTESIAN_POINT('Ctrl Pts',(1.87563767773588,-1.,-0.175563480746485));
#29444=CARTESIAN_POINT('Ctrl Pts',(1.88188663145367,-1.,-0.175644148889699));
#29445=CARTESIAN_POINT('Ctrl Pts',(1.88742606273259,-1.,-0.175538155840648));
#29446=CARTESIAN_POINT('Ctrl Pts',(1.892646301985,-1.,-0.175274276190844));
#29447=CARTESIAN_POINT('Ctrl Pts',(1.89788101117132,-1.,-0.174879405091263));
#29448=CARTESIAN_POINT('Ctrl Pts',(1.90335253862834,-1.,-0.174375518661085));
#29449=CARTESIAN_POINT('Ctrl Pts',(1.90911693975267,-1.,-0.173776635257817));
#29450=CARTESIAN_POINT('Ctrl Pts',(1.91511429159527,-1.,-0.173090695383496));
#29451=CARTESIAN_POINT('Ctrl Pts',(1.9212233439798,-1.,-0.172321621259514));
#29452=CARTESIAN_POINT('Ctrl Pts',(1.92731093582036,-1.,-0.171471191532988));
#29453=CARTESIAN_POINT('Ctrl Pts',(1.93329183155539,-1.,-0.170541253116202));
#29454=CARTESIAN_POINT('Ctrl Pts',(1.93915639211581,-1.,-0.169534904817491));
#29455=CARTESIAN_POINT('Ctrl Pts',(1.94493757756931,-1.,-0.168455741607556));
#29456=CARTESIAN_POINT('Ctrl Pts',(1.95069027794294,-1.,-0.167307501784476));
#29457=CARTESIAN_POINT('Ctrl Pts',(1.9564675971873,-1.,-0.166093592002813));
#29458=CARTESIAN_POINT('Ctrl Pts',(1.96229379940136,-1.,-0.164816568920269));
#29459=CARTESIAN_POINT('Ctrl Pts',(1.96816512677967,-1.,-0.163478185457734));
#29460=CARTESIAN_POINT('Ctrl Pts',(1.97406280235188,-1.,-0.162079693556289));
#29461=CARTESIAN_POINT('Ctrl Pts',(1.97996195437559,-1.,-0.160622060784611));
#29462=CARTESIAN_POINT('Ctrl Pts',(1.98584238283292,-1.,-0.159106226437299));
#29463=CARTESIAN_POINT('Ctrl Pts',(1.99169810931908,-1.,-0.157533331459227));
#29464=CARTESIAN_POINT('Ctrl Pts',(1.99753284771497,-1.,-0.155904629548784));
#29465=CARTESIAN_POINT('Ctrl Pts',(2.00335565310543,-1.,-0.154221403049722));
#29466=CARTESIAN_POINT('Ctrl Pts',(2.00917680318424,-1.,-0.15248488362145));
#29467=CARTESIAN_POINT('Ctrl Pts',(2.01500291940238,-1.,-0.150696157673078));
#29468=CARTESIAN_POINT('Ctrl Pts',(2.02083464969894,-1.,-0.148856124775337));
#29469=CARTESIAN_POINT('Ctrl Pts',(2.02666926182017,-1.,-0.146965557332583));
#29470=CARTESIAN_POINT('Ctrl Pts',(2.03250223739942,-1.,-0.145025140186058));
#29471=CARTESIAN_POINT('Ctrl Pts',(2.03832911025912,-1.,-0.143035515058209));
#29472=CARTESIAN_POINT('Ctrl Pts',(2.04414757947916,-1.,-0.140997332152546));
#29473=CARTESIAN_POINT('Ctrl Pts',(2.04995762001328,-1.,-0.138911255368966));
#29474=CARTESIAN_POINT('Ctrl Pts',(2.05576044414264,-1.,-0.136777941218044));
#29475=CARTESIAN_POINT('Ctrl Pts',(2.06155781517842,-1.,-0.134598026192106));
#29476=CARTESIAN_POINT('Ctrl Pts',(2.06735123910326,-1.,-0.132372111547711));
#29477=CARTESIAN_POINT('Ctrl Pts',(2.07314114713063,-1.,-0.130100748328404));
#29478=CARTESIAN_POINT('Ctrl Pts',(2.07892715110987,-1.,-0.12778444527612));
#29479=CARTESIAN_POINT('Ctrl Pts',(2.08470840653643,-1.,-0.125423679412062));
#29480=CARTESIAN_POINT('Ctrl Pts',(2.09048392424825,-1.,-0.123018905621083));
#29481=CARTESIAN_POINT('Ctrl Pts',(2.0962529286773,-1.,-0.120570567965122));
#29482=CARTESIAN_POINT('Ctrl Pts',(2.102015121329,-1.,-0.118079107988356));
#29483=CARTESIAN_POINT('Ctrl Pts',(2.10777050261309,-1.,-0.115544957687927));
#29484=CARTESIAN_POINT('Ctrl Pts',(2.11351924490306,-1.,-0.112968534419737));
#29485=CARTESIAN_POINT('Ctrl Pts',(2.11926155590865,-1.,-0.110350236135025));
#29486=CARTESIAN_POINT('Ctrl Pts',(2.12499752307,-1.,-0.10769043523109));
#29487=CARTESIAN_POINT('Ctrl Pts',(2.13072704887293,-1.,-0.10498947915274));
#29488=CARTESIAN_POINT('Ctrl Pts',(2.13644992667165,-1.,-0.102247700556101));
#29489=CARTESIAN_POINT('Ctrl Pts',(2.14216588396025,-1.,-0.0994654261990917));
#29490=CARTESIAN_POINT('Ctrl Pts',(2.14787463531795,-1.,-0.096642985230546));
#29491=CARTESIAN_POINT('Ctrl Pts',(2.1535759397817,-1.,-0.0937807218867645));
#29492=CARTESIAN_POINT('Ctrl Pts',(2.15926961544516,-1.,-0.0908789888107267));
#29493=CARTESIAN_POINT('Ctrl Pts',(2.16495552645014,-1.,-0.0879381291386924));
#29494=CARTESIAN_POINT('Ctrl Pts',(2.17063357870952,-1.,-0.0849584620835374));
#29495=CARTESIAN_POINT('Ctrl Pts',(2.176303712113,-1.,-0.0819402680872767));
#29496=CARTESIAN_POINT('Ctrl Pts',(2.18196589448887,-1.,-0.0788837727685244));
#29497=CARTESIAN_POINT('Ctrl Pts',(2.1876201139953,-1.,-0.0757891465836149));
#29498=CARTESIAN_POINT('Ctrl Pts',(2.19213712013662,-1.,-0.0732830357306726));
#29499=CARTESIAN_POINT('Ctrl Pts',(2.19552129484002,-1.,-0.0713863779526155));
#29500=CARTESIAN_POINT('Ctrl Pts',(2.19777582085423,-1.,-0.0701143536325491));
#29501=CARTESIAN_POINT('Ctrl Pts',(2.19890268624765,-1.,-0.0694764450219582));
#29502=CARTESIAN_POINT('',(2.19890268624765,-1.,0.0694764450219582));
#29503=CARTESIAN_POINT('',(2.19890268624765,-1.,-0.0694764450219582));
#29504=CARTESIAN_POINT('',(1.74236521665491,-1.,0.163289472382896));
#29505=CARTESIAN_POINT('Ctrl Pts',(2.19890268624765,-1.,0.0694764450219582));
#29506=CARTESIAN_POINT('Ctrl Pts',(2.19777582085261,-1.,0.0701143536324925));
#29507=CARTESIAN_POINT('Ctrl Pts',(2.19552129483562,-1.,0.0713863779524626));
#29508=CARTESIAN_POINT('Ctrl Pts',(2.19213712012956,-1.,0.0732830357304275));
#29509=CARTESIAN_POINT('Ctrl Pts',(2.1876201139874,-1.,0.075789146583341));
#29510=CARTESIAN_POINT('Ctrl Pts',(2.18196589448304,-1.,0.0788837727683226));
#29511=CARTESIAN_POINT('Ctrl Pts',(2.1763037121106,-1.,0.0819402680871938));
#29512=CARTESIAN_POINT('Ctrl Pts',(2.17063357871031,-1.,0.0849584620835642));
#29513=CARTESIAN_POINT('Ctrl Pts',(2.16495552645275,-1.,0.0879381291387821));
#29514=CARTESIAN_POINT('Ctrl Pts',(2.15926961544808,-1.,0.0908789888108265));
#29515=CARTESIAN_POINT('Ctrl Pts',(2.15357593978377,-1.,0.0937807218868344));
#29516=CARTESIAN_POINT('Ctrl Pts',(2.14787463531864,-1.,0.0966429852305688));
#29517=CARTESIAN_POINT('Ctrl Pts',(2.14216588395974,-1.,0.0994654261990741));
#29518=CARTESIAN_POINT('Ctrl Pts',(2.13644992667052,-1.,0.102247700556063));
#29519=CARTESIAN_POINT('Ctrl Pts',(2.1307270488718,-1.,0.104989479152703));
#29520=CARTESIAN_POINT('Ctrl Pts',(2.12499752306927,-1.,0.107690435231068));
#29521=CARTESIAN_POINT('Ctrl Pts',(2.11926155590849,-1.,0.11035023613502));
#29522=CARTESIAN_POINT('Ctrl Pts',(2.11351924490335,-1.,0.112968534419746));
#29523=CARTESIAN_POINT('Ctrl Pts',(2.10777050261359,-1.,0.11554495768794));
#29524=CARTESIAN_POINT('Ctrl Pts',(2.10201512132945,-1.,0.118079107988368));
#29525=CARTESIAN_POINT('Ctrl Pts',(2.09625292867756,-1.,0.120570567965129));
#29526=CARTESIAN_POINT('Ctrl Pts',(2.09048392424826,-1.,0.123018905621083));
#29527=CARTESIAN_POINT('Ctrl Pts',(2.08470840653628,-1.,0.125423679412058));
#29528=CARTESIAN_POINT('Ctrl Pts',(2.07892715110967,-1.,0.127784445276116));
#29529=CARTESIAN_POINT('Ctrl Pts',(2.07314114713047,-1.,0.1301007483284));
#29530=CARTESIAN_POINT('Ctrl Pts',(2.06735123910319,-1.,0.132372111547709));
#29531=CARTESIAN_POINT('Ctrl Pts',(2.06155781517844,-1.,0.134598026192107));
#29532=CARTESIAN_POINT('Ctrl Pts',(2.0557604441427,-1.,0.136777941218044));
#29533=CARTESIAN_POINT('Ctrl Pts',(2.04995762001333,-1.,0.138911255368966));
#29534=CARTESIAN_POINT('Ctrl Pts',(2.04414757947919,-1.,0.140997332152545));
#29535=CARTESIAN_POINT('Ctrl Pts',(2.03832911025913,-1.,0.143035515058208));
#29536=CARTESIAN_POINT('Ctrl Pts',(2.03250223739941,-1.,0.145025140186058));
#29537=CARTESIAN_POINT('Ctrl Pts',(2.02666926182017,-1.,0.146965557332586));
#29538=CARTESIAN_POINT('Ctrl Pts',(2.02083464969897,-1.,0.148856124775342));
#29539=CARTESIAN_POINT('Ctrl Pts',(2.01500291940243,-1.,0.150696157673084));
#29540=CARTESIAN_POINT('Ctrl Pts',(2.00917680318426,-1.,0.152484883621452));
#29541=CARTESIAN_POINT('Ctrl Pts',(2.00335565310539,-1.,0.154221403049719));
#29542=CARTESIAN_POINT('Ctrl Pts',(1.99753284771487,-1.,0.155904629548774));
#29543=CARTESIAN_POINT('Ctrl Pts',(1.99169810931893,-1.,0.157533331459215));
#29544=CARTESIAN_POINT('Ctrl Pts',(1.98584238283279,-1.,0.159106226437288));
#29545=CARTESIAN_POINT('Ctrl Pts',(1.97996195437557,-1.,0.16062206078461));
#29546=CARTESIAN_POINT('Ctrl Pts',(1.97406280235204,-1.,0.162079693556302));
#29547=CARTESIAN_POINT('Ctrl Pts',(1.96816512678,-1.,0.16347818545776));
#29548=CARTESIAN_POINT('Ctrl Pts',(1.96229379940174,-1.,0.1648165689203));
#29549=CARTESIAN_POINT('Ctrl Pts',(1.95646759718755,-1.,0.166093592002832));
#29550=CARTESIAN_POINT('Ctrl Pts',(1.95069027794286,-1.,0.167307501784469));
#29551=CARTESIAN_POINT('Ctrl Pts',(1.94493757756879,-1.,0.168455741607515));
#29552=CARTESIAN_POINT('Ctrl Pts',(1.93915639211497,-1.,0.169534904817425));
#29553=CARTESIAN_POINT('Ctrl Pts',(1.93329183155455,-1.,0.170541253116136));
#29554=CARTESIAN_POINT('Ctrl Pts',(1.92731093582,-1.,0.17147119153296));
#29555=CARTESIAN_POINT('Ctrl Pts',(1.92122334398034,-1.,0.172321621259556));
#29556=CARTESIAN_POINT('Ctrl Pts',(1.91511429159681,-1.,0.173090695383619));
#29557=CARTESIAN_POINT('Ctrl Pts',(1.90911693975475,-1.,0.173776635257983));
#29558=CARTESIAN_POINT('Ctrl Pts',(1.90335253863003,-1.,0.174375518661222));
#29559=CARTESIAN_POINT('Ctrl Pts',(1.89788101117148,-1.,0.174879405091277));
#29560=CARTESIAN_POINT('Ctrl Pts',(1.89264630198279,-1.,0.175274276190664));
#29561=CARTESIAN_POINT('Ctrl Pts',(1.88742606272818,-1.,0.175538155840286));
#29562=CARTESIAN_POINT('Ctrl Pts',(1.88188663144846,-1.,0.175644148889271));
#29563=CARTESIAN_POINT('Ctrl Pts',(1.87563767773249,-1.,0.175563480746205));
#29564=CARTESIAN_POINT('Ctrl Pts',(1.86828349694972,-1.,0.1752683375909));
#29565=CARTESIAN_POINT('Ctrl Pts',(1.85948367089838,-1.,0.174735259276856));
#29566=CARTESIAN_POINT('Ctrl Pts',(1.84898113200543,-1.,0.173946627589401));
#29567=CARTESIAN_POINT('Ctrl Pts',(1.83658380530747,-1.,0.17288944289442));
#29568=CARTESIAN_POINT('Ctrl Pts',(1.82215766815414,-1.,0.171554770207306));
#29569=CARTESIAN_POINT('Ctrl Pts',(1.80561530633924,-1.,0.169936923908078));
#29570=CARTESIAN_POINT('Ctrl Pts',(1.78690649988931,-1.,0.16803277280837));
#29571=CARTESIAN_POINT('Ctrl Pts',(1.77018771687692,-1.,0.166279355148738));
#29572=CARTESIAN_POINT('Ctrl Pts',(1.75666056640041,-1.,0.164834765708484));
#29573=CARTESIAN_POINT('Ctrl Pts',(1.74720349503904,-1.,0.163814161002474));
#29574=CARTESIAN_POINT('Ctrl Pts',(1.74236521665491,-1.,0.163289472382896));
#29575=CARTESIAN_POINT('',(1.7075470150345,-1.,0.383122945602004));
#29576=CARTESIAN_POINT('Origin',(0.,-1.,0.));
#29577=CARTESIAN_POINT('',(2.11275013067528,-1.,0.613422273260091));
#29578=CARTESIAN_POINT('Ctrl Pts',(1.7075470150345,-1.,0.383122945602004));
#29579=CARTESIAN_POINT('Ctrl Pts',(1.71231062891398,-1.,0.384119047314215));
#29580=CARTESIAN_POINT('Ctrl Pts',(1.72162022244582,-1.,0.386070790323281));
#29581=CARTESIAN_POINT('Ctrl Pts',(1.73493170972829,-1.,0.388877023502615));
#29582=CARTESIAN_POINT('Ctrl Pts',(1.75137405310193,-1.,0.392375812285396));
#29583=CARTESIAN_POINT('Ctrl Pts',(1.76975560043442,-1.,0.396346196110688));
#29584=CARTESIAN_POINT('Ctrl Pts',(1.78598826343754,-1.,0.399919403774156));
#29585=CARTESIAN_POINT('Ctrl Pts',(1.80012077173238,-1.,0.403107976163396));
#29586=CARTESIAN_POINT('Ctrl Pts',(1.81223801812013,-1.,0.405933518407176));
#29587=CARTESIAN_POINT('Ctrl Pts',(1.82247022677562,-1.,0.408428948106228));
#29588=CARTESIAN_POINT('Ctrl Pts',(1.83100408895047,-1.,0.410641256301276));
#29589=CARTESIAN_POINT('Ctrl Pts',(1.8380895347617,-1.,0.412633125322945));
#29590=CARTESIAN_POINT('Ctrl Pts',(1.84405757074218,-1.,0.414487438255542));
#29591=CARTESIAN_POINT('Ctrl Pts',(1.84929312930314,-1.,0.416300022039885));
#29592=CARTESIAN_POINT('Ctrl Pts',(1.8541763285645,-1.,0.418164129144046));
#29593=CARTESIAN_POINT('Ctrl Pts',(1.8590328109667,-1.,0.420157287975583));
#29594=CARTESIAN_POINT('Ctrl Pts',(1.86408083333863,-1.,0.422327307417885));
#29595=CARTESIAN_POINT('Ctrl Pts',(1.8693780394412,-1.,0.424678177290876));
#29596=CARTESIAN_POINT('Ctrl Pts',(1.87486989291333,-1.,0.427183828518743));
#29597=CARTESIAN_POINT('Ctrl Pts',(1.88044229001778,-1.,0.429803062482217));
#29598=CARTESIAN_POINT('Ctrl Pts',(1.88596913666828,-1.,0.432493038548833));
#29599=CARTESIAN_POINT('Ctrl Pts',(1.89136993975585,-1.,0.43522566096358));
#29600=CARTESIAN_POINT('Ctrl Pts',(1.89663648956549,-1.,0.437995003948443));
#29601=CARTESIAN_POINT('Ctrl Pts',(1.90180124389137,-1.,0.440807833704161));
#29602=CARTESIAN_POINT('Ctrl Pts',(1.90691756144906,-1.,0.443677556849171));
#29603=CARTESIAN_POINT('Ctrl Pts',(1.91203699981095,-1.,0.446617343485651));
#29604=CARTESIAN_POINT('Ctrl Pts',(1.91718342555717,-1.,0.449632260106572));
#29605=CARTESIAN_POINT('Ctrl Pts',(1.9223538064847,-1.,0.452719478359356));
#29606=CARTESIAN_POINT('Ctrl Pts',(1.92753067150461,-1.,0.455872005174336));
#29607=CARTESIAN_POINT('Ctrl Pts',(1.93269066517936,-1.,0.459081234547932));
#29608=CARTESIAN_POINT('Ctrl Pts',(1.93781486640834,-1.,0.462340031009087));
#29609=CARTESIAN_POINT('Ctrl Pts',(1.94289794196205,-1.,0.465645462026065));
#29610=CARTESIAN_POINT('Ctrl Pts',(1.94794381136524,-1.,0.468997482913158));
#29611=CARTESIAN_POINT('Ctrl Pts',(1.95296148278136,-1.,0.47239767226408));
#29612=CARTESIAN_POINT('Ctrl Pts',(1.95796111148175,-1.,0.475848034683172));
#29613=CARTESIAN_POINT('Ctrl Pts',(1.96294933055938,-1.,0.479349583074846));
#29614=CARTESIAN_POINT('Ctrl Pts',(1.96792703422358,-1.,0.482901662120687));
#29615=CARTESIAN_POINT('Ctrl Pts',(1.97289186263272,-1.,0.486502692907661));
#29616=CARTESIAN_POINT('Ctrl Pts',(1.97783973019229,-1.,0.490150627860955));
#29617=CARTESIAN_POINT('Ctrl Pts',(1.9827665876182,-1.,0.493843476541493));
#29618=CARTESIAN_POINT('Ctrl Pts',(1.98767044752929,-1.,0.497579909545564));
#29619=CARTESIAN_POINT('Ctrl Pts',(1.9925514912615,-1.,0.501359287727129));
#29620=CARTESIAN_POINT('Ctrl Pts',(1.99741107463567,-1.,0.505181361323011));
#29621=CARTESIAN_POINT('Ctrl Pts',(2.00225107134733,-1.,0.509046069886152));
#29622=CARTESIAN_POINT('Ctrl Pts',(2.00707309946955,-1.,0.512953306961814));
#29623=CARTESIAN_POINT('Ctrl Pts',(2.01187773939257,-1.,0.516902681728733));
#29624=CARTESIAN_POINT('Ctrl Pts',(2.01666477917305,-1.,0.520893590399429));
#29625=CARTESIAN_POINT('Ctrl Pts',(2.02143356304712,-1.,0.524925318333519));
#29626=CARTESIAN_POINT('Ctrl Pts',(2.02618329083289,-1.,0.528997127241911));
#29627=CARTESIAN_POINT('Ctrl Pts',(2.03091336214401,-1.,0.533108355132905));
#29628=CARTESIAN_POINT('Ctrl Pts',(2.03562362953993,-1.,0.537258489833135));
#29629=CARTESIAN_POINT('Ctrl Pts',(2.0403142269048,-1.,0.54144712061552));
#29630=CARTESIAN_POINT('Ctrl Pts',(2.0449854471456,-1.,0.545673903817349));
#29631=CARTESIAN_POINT('Ctrl Pts',(2.04963761077974,-1.,0.549938525150342));
#29632=CARTESIAN_POINT('Ctrl Pts',(2.05427091604482,-1.,0.55424065746411));
#29633=CARTESIAN_POINT('Ctrl Pts',(2.05888537756571,-1.,0.558579940185468));
#29634=CARTESIAN_POINT('Ctrl Pts',(2.06348090160697,-1.,0.562955993082574));
#29635=CARTESIAN_POINT('Ctrl Pts',(2.06805732997383,-1.,0.56736842118123));
#29636=CARTESIAN_POINT('Ctrl Pts',(2.07261449292757,-1.,0.571816823242411));
#29637=CARTESIAN_POINT('Ctrl Pts',(2.07715226767361,-1.,0.576300797416275));
#29638=CARTESIAN_POINT('Ctrl Pts',(2.08167059018138,-1.,0.580819952107257));
#29639=CARTESIAN_POINT('Ctrl Pts',(2.086169437277,-1.,0.585373918990895));
#29640=CARTESIAN_POINT('Ctrl Pts',(2.09064881812053,-1.,0.58996236540319));
#29641=CARTESIAN_POINT('Ctrl Pts',(2.09510876220501,-1.,0.594585006052824));
#29642=CARTESIAN_POINT('Ctrl Pts',(2.09954930865331,-1.,0.599241616422144));
#29643=CARTESIAN_POINT('Ctrl Pts',(2.10397049887709,-1.,0.603932030738212));
#29644=CARTESIAN_POINT('Ctrl Pts',(2.10749199615859,-1.,0.607711315456826));
#29645=CARTESIAN_POINT('Ctrl Pts',(2.11012443807661,-1.,0.610560911691114));
#29646=CARTESIAN_POINT('Ctrl Pts',(2.11187554260142,-1.,0.61246736556225));
#29647=CARTESIAN_POINT('Ctrl Pts',(2.11275013067528,-1.,0.613422273260091));
#29648=CARTESIAN_POINT('',(2.0698113262342,-1.,0.745574324794401));
#29649=CARTESIAN_POINT('',(2.11275013067528,-1.,0.613422273260091));
#29650=CARTESIAN_POINT('Ctrl Pts',(2.0698113262342,-1.,0.745574324794401));
#29651=CARTESIAN_POINT('Ctrl Pts',(2.06854248895575,-1.,0.74583279137781));
#29652=CARTESIAN_POINT('Ctrl Pts',(2.06600523016401,-1.,0.746345871542696));
#29653=CARTESIAN_POINT('Ctrl Pts',(2.06220058927162,-1.,0.747103932785504));
#29654=CARTESIAN_POINT('Ctrl Pts',(2.05713023030263,-1.,0.748091554181101));
#29655=CARTESIAN_POINT('Ctrl Pts',(2.05079645591606,-1.,0.749287468663053));
#29656=CARTESIAN_POINT('Ctrl Pts',(2.04446689147754,-1.,0.750444657874758));
#29657=CARTESIAN_POINT('Ctrl Pts',(2.03814160092173,-1.,0.751562963361384));
#29658=CARTESIAN_POINT('Ctrl Pts',(2.03182068456467,-1.,0.752642180488104));
#29659=CARTESIAN_POINT('Ctrl Pts',(2.02550428623587,-1.,0.753682061113766));
#29660=CARTESIAN_POINT('Ctrl Pts',(2.01919259406003,-1.,0.75468233072352));
#29661=CARTESIAN_POINT('Ctrl Pts',(2.01288584328149,-1.,0.755642704958101));
#29662=CARTESIAN_POINT('Ctrl Pts',(2.00658431587682,-1.,0.756562904646496));
#29663=CARTESIAN_POINT('Ctrl Pts',(2.00028834739072,-1.,0.757442676862342));
#29664=CARTESIAN_POINT('Ctrl Pts',(1.9939983109871,-1.,0.758281796766377));
#29665=CARTESIAN_POINT('Ctrl Pts',(1.98771456680806,-1.,0.759080037802243));
#29666=CARTESIAN_POINT('Ctrl Pts',(1.98143741418156,-1.,0.759837147452135));
#29667=CARTESIAN_POINT('Ctrl Pts',(1.97516705321521,-1.,0.760552825409856));
#29668=CARTESIAN_POINT('Ctrl Pts',(1.96890351582545,-1.,0.761226690483986));
#29669=CARTESIAN_POINT('Ctrl Pts',(1.96264672744229,-1.,0.761858300014575));
#29670=CARTESIAN_POINT('Ctrl Pts',(1.95639665309893,-1.,0.762447203806264));
#29671=CARTESIAN_POINT('Ctrl Pts',(1.95015342590025,-1.,0.762992990878774));
#29672=CARTESIAN_POINT('Ctrl Pts',(1.94391746617626,-1.,0.763495333538581));
#29673=CARTESIAN_POINT('Ctrl Pts',(1.93768964875867,-1.,0.763954049121394));
#29674=CARTESIAN_POINT('Ctrl Pts',(1.93147105496367,-1.,0.76436901067389));
#29675=CARTESIAN_POINT('Ctrl Pts',(1.92526263537041,-1.,0.764740025488189));
#29676=CARTESIAN_POINT('Ctrl Pts',(1.91906491634197,-1.,0.765066729667095));
#29677=CARTESIAN_POINT('Ctrl Pts',(1.91287765805174,-1.,0.765348465884739));
#29678=CARTESIAN_POINT('Ctrl Pts',(1.90669961402362,-1.,0.765584196937937));
#29679=CARTESIAN_POINT('Ctrl Pts',(1.90052930393599,-1.,0.765772772593395));
#29680=CARTESIAN_POINT('Ctrl Pts',(1.89436577771389,-1.,0.765913193856979));
#29681=CARTESIAN_POINT('Ctrl Pts',(1.88820926433409,-1.,0.76600483706209));
#29682=CARTESIAN_POINT('Ctrl Pts',(1.88206215302561,-1.,0.766047794851869));
#29683=CARTESIAN_POINT('Ctrl Pts',(1.87592888967886,-1.,0.766042837036759));
#29684=CARTESIAN_POINT('Ctrl Pts',(1.86981398314345,-1.,0.765990708546112));
#29685=CARTESIAN_POINT('Ctrl Pts',(1.86372027063314,-1.,0.765891519092557));
#29686=CARTESIAN_POINT('Ctrl Pts',(1.85764741390391,-1.,0.765744212909305));
#29687=CARTESIAN_POINT('Ctrl Pts',(1.85158945130054,-1.,0.765545710619023));
#29688=CARTESIAN_POINT('Ctrl Pts',(1.8455369887591,-1.,0.765291664861972));
#29689=CARTESIAN_POINT('Ctrl Pts',(1.83948181064823,-1.,0.764978057881688));
#29690=CARTESIAN_POINT('Ctrl Pts',(1.8334207722714,-1.,0.764602549687846));
#29691=CARTESIAN_POINT('Ctrl Pts',(1.8273599120008,-1.,0.764165902606056));
#29692=CARTESIAN_POINT('Ctrl Pts',(1.82131873145297,-1.,0.763673465462854));
#29693=CARTESIAN_POINT('Ctrl Pts',(1.81532118405566,-1.,0.763132003836783));
#29694=CARTESIAN_POINT('Ctrl Pts',(1.80938551463989,-1.,0.762546129464036));
#29695=CARTESIAN_POINT('Ctrl Pts',(1.80351583877334,-1.,0.761915336443516));
#29696=CARTESIAN_POINT('Ctrl Pts',(1.79768986997735,-1.,0.761229695230359));
#29697=CARTESIAN_POINT('Ctrl Pts',(1.79185815610802,-1.,0.760469555880425));
#29698=CARTESIAN_POINT('Ctrl Pts',(1.78596964884526,-1.,0.759614401109868));
#29699=CARTESIAN_POINT('Ctrl Pts',(1.77999411220912,-1.,0.75865062667738));
#29700=CARTESIAN_POINT('Ctrl Pts',(1.77394167108342,-1.,0.757578264077238));
#29701=CARTESIAN_POINT('Ctrl Pts',(1.76789396003141,-1.,0.756421896028403));
#29702=CARTESIAN_POINT('Ctrl Pts',(1.7619781724032,-1.,0.755220979975262));
#29703=CARTESIAN_POINT('Ctrl Pts',(1.75631083600175,-1.,0.75400925402848));
#29704=CARTESIAN_POINT('Ctrl Pts',(1.75095139468809,-1.,0.752797683531377));
#29705=CARTESIAN_POINT('Ctrl Pts',(1.74585086852298,-1.,0.751555614163629));
#29706=CARTESIAN_POINT('Ctrl Pts',(1.74080458266705,-1.,0.750193435979541));
#29707=CARTESIAN_POINT('Ctrl Pts',(1.73550351679848,-1.,0.748582462954855));
#29708=CARTESIAN_POINT('Ctrl Pts',(1.72958533647399,-1.,0.746574710096437));
#29709=CARTESIAN_POINT('Ctrl Pts',(1.7226822991693,-1.,0.744021445433765));
#29710=CARTESIAN_POINT('Ctrl Pts',(1.71447789751927,-1.,0.740795162032088));
#29711=CARTESIAN_POINT('Ctrl Pts',(1.70473309006121,-1.,0.736799665724771));
#29712=CARTESIAN_POINT('Ctrl Pts',(1.69326921975743,-1.,0.731963238697195));
#29713=CARTESIAN_POINT('Ctrl Pts',(1.67996158455503,-1.,0.726235967997433));
#29714=CARTESIAN_POINT('Ctrl Pts',(1.6647288055568,-1.,0.719585433804282));
#29715=CARTESIAN_POINT('Ctrl Pts',(1.64752408832016,-1.,0.711993139355394));
#29716=CARTESIAN_POINT('Ctrl Pts',(1.63216541664676,-1.,0.705159151988319));
#29717=CARTESIAN_POINT('Ctrl Pts',(1.61974673472612,-1.,0.699605146405088));
#29718=CARTESIAN_POINT('Ctrl Pts',(1.61106790958151,-1.,0.695712097881194));
#29719=CARTESIAN_POINT('Ctrl Pts',(1.60662857109684,-1.,0.693717979106306));
#29720=CARTESIAN_POINT('Origin',(0.,-1.,0.));
#29721=CARTESIAN_POINT('Origin',(0.,0.,0.));
#29722=CARTESIAN_POINT('Origin',(0.,2.2,0.));
#29723=CARTESIAN_POINT('Origin',(0.,1.,0.));
#29724=CARTESIAN_POINT('',(-1.4,2.2,1.71450551880629E-16));
#29725=CARTESIAN_POINT('Origin',(0.,2.2,0.));
#29726=CARTESIAN_POINT('',(-1.4,1.,1.71450551880629E-16));
#29727=CARTESIAN_POINT('',(-1.4,1.,1.71450551880629E-16));
#29728=CARTESIAN_POINT('Origin',(0.,1.,0.));
#29729=CARTESIAN_POINT('Origin',(0.,2.2,0.));
#29730=CARTESIAN_POINT('Ctrl Pts',(2.11275013067528,-1.,0.613422273260091));
#29731=CARTESIAN_POINT('Ctrl Pts',(2.11275013067528,1.,0.613422273260091));
#29732=CARTESIAN_POINT('Ctrl Pts',(2.11187554260142,-1.,0.61246736556225));
#29733=CARTESIAN_POINT('Ctrl Pts',(2.11187554260142,1.,0.61246736556225));
#29734=CARTESIAN_POINT('Ctrl Pts',(2.11012443807661,-1.,0.610560911691114));
#29735=CARTESIAN_POINT('Ctrl Pts',(2.11012443807661,1.,0.610560911691114));
#29736=CARTESIAN_POINT('Ctrl Pts',(2.10749199615859,-1.,0.607711315456826));
#29737=CARTESIAN_POINT('Ctrl Pts',(2.10749199615859,1.,0.607711315456826));
#29738=CARTESIAN_POINT('Ctrl Pts',(2.10397049887709,-1.,0.603932030738212));
#29739=CARTESIAN_POINT('Ctrl Pts',(2.10397049887709,1.,0.603932030738212));
#29740=CARTESIAN_POINT('Ctrl Pts',(2.09954930865331,-1.,0.599241616422144));
#29741=CARTESIAN_POINT('Ctrl Pts',(2.09954930865331,1.,0.599241616422144));
#29742=CARTESIAN_POINT('Ctrl Pts',(2.09510876220501,-1.,0.594585006052824));
#29743=CARTESIAN_POINT('Ctrl Pts',(2.09510876220501,1.,0.594585006052824));
#29744=CARTESIAN_POINT('Ctrl Pts',(2.09064881812053,-1.,0.58996236540319));
#29745=CARTESIAN_POINT('Ctrl Pts',(2.09064881812053,1.,0.58996236540319));
#29746=CARTESIAN_POINT('Ctrl Pts',(2.086169437277,-1.,0.585373918990895));
#29747=CARTESIAN_POINT('Ctrl Pts',(2.086169437277,1.,0.585373918990895));
#29748=CARTESIAN_POINT('Ctrl Pts',(2.08167059018138,-1.,0.580819952107257));
#29749=CARTESIAN_POINT('Ctrl Pts',(2.08167059018138,1.,0.580819952107257));
#29750=CARTESIAN_POINT('Ctrl Pts',(2.07715226767361,-1.,0.576300797416275));
#29751=CARTESIAN_POINT('Ctrl Pts',(2.07715226767361,1.,0.576300797416275));
#29752=CARTESIAN_POINT('Ctrl Pts',(2.07261449292757,-1.,0.571816823242411));
#29753=CARTESIAN_POINT('Ctrl Pts',(2.07261449292757,1.,0.571816823242411));
#29754=CARTESIAN_POINT('Ctrl Pts',(2.06805732997383,-1.,0.56736842118123));
#29755=CARTESIAN_POINT('Ctrl Pts',(2.06805732997383,1.,0.56736842118123));
#29756=CARTESIAN_POINT('Ctrl Pts',(2.06348090160697,-1.,0.562955993082574));
#29757=CARTESIAN_POINT('Ctrl Pts',(2.06348090160697,1.,0.562955993082574));
#29758=CARTESIAN_POINT('Ctrl Pts',(2.05888537756571,-1.,0.558579940185468));
#29759=CARTESIAN_POINT('Ctrl Pts',(2.05888537756571,1.,0.558579940185468));
#29760=CARTESIAN_POINT('Ctrl Pts',(2.05427091604482,-1.,0.55424065746411));
#29761=CARTESIAN_POINT('Ctrl Pts',(2.05427091604482,1.,0.55424065746411));
#29762=CARTESIAN_POINT('Ctrl Pts',(2.04963761077974,-1.,0.549938525150342));
#29763=CARTESIAN_POINT('Ctrl Pts',(2.04963761077974,1.,0.549938525150342));
#29764=CARTESIAN_POINT('Ctrl Pts',(2.0449854471456,-1.,0.545673903817349));
#29765=CARTESIAN_POINT('Ctrl Pts',(2.0449854471456,1.,0.545673903817349));
#29766=CARTESIAN_POINT('Ctrl Pts',(2.0403142269048,-1.,0.54144712061552));
#29767=CARTESIAN_POINT('Ctrl Pts',(2.0403142269048,1.,0.54144712061552));
#29768=CARTESIAN_POINT('Ctrl Pts',(2.03562362953993,-1.,0.537258489833135));
#29769=CARTESIAN_POINT('Ctrl Pts',(2.03562362953993,1.,0.537258489833135));
#29770=CARTESIAN_POINT('Ctrl Pts',(2.03091336214401,-1.,0.533108355132905));
#29771=CARTESIAN_POINT('Ctrl Pts',(2.03091336214401,1.,0.533108355132905));
#29772=CARTESIAN_POINT('Ctrl Pts',(2.02618329083289,-1.,0.528997127241911));
#29773=CARTESIAN_POINT('Ctrl Pts',(2.02618329083289,1.,0.528997127241911));
#29774=CARTESIAN_POINT('Ctrl Pts',(2.02143356304712,-1.,0.524925318333519));
#29775=CARTESIAN_POINT('Ctrl Pts',(2.02143356304712,1.,0.524925318333519));
#29776=CARTESIAN_POINT('Ctrl Pts',(2.01666477917305,-1.,0.520893590399429));
#29777=CARTESIAN_POINT('Ctrl Pts',(2.01666477917305,1.,0.520893590399429));
#29778=CARTESIAN_POINT('Ctrl Pts',(2.01187773939257,-1.,0.516902681728733));
#29779=CARTESIAN_POINT('Ctrl Pts',(2.01187773939257,1.,0.516902681728733));
#29780=CARTESIAN_POINT('Ctrl Pts',(2.00707309946955,-1.,0.512953306961814));
#29781=CARTESIAN_POINT('Ctrl Pts',(2.00707309946955,1.,0.512953306961814));
#29782=CARTESIAN_POINT('Ctrl Pts',(2.00225107134733,-1.,0.509046069886152));
#29783=CARTESIAN_POINT('Ctrl Pts',(2.00225107134733,1.,0.509046069886152));
#29784=CARTESIAN_POINT('Ctrl Pts',(1.99741107463567,-1.,0.505181361323011));
#29785=CARTESIAN_POINT('Ctrl Pts',(1.99741107463567,1.,0.505181361323011));
#29786=CARTESIAN_POINT('Ctrl Pts',(1.9925514912615,-1.,0.501359287727129));
#29787=CARTESIAN_POINT('Ctrl Pts',(1.9925514912615,1.,0.501359287727129));
#29788=CARTESIAN_POINT('Ctrl Pts',(1.98767044752929,-1.,0.497579909545564));
#29789=CARTESIAN_POINT('Ctrl Pts',(1.98767044752929,1.,0.497579909545564));
#29790=CARTESIAN_POINT('Ctrl Pts',(1.9827665876182,-1.,0.493843476541493));
#29791=CARTESIAN_POINT('Ctrl Pts',(1.9827665876182,1.,0.493843476541493));
#29792=CARTESIAN_POINT('Ctrl Pts',(1.97783973019229,-1.,0.490150627860955));
#29793=CARTESIAN_POINT('Ctrl Pts',(1.97783973019229,1.,0.490150627860955));
#29794=CARTESIAN_POINT('Ctrl Pts',(1.97289186263272,-1.,0.486502692907661));
#29795=CARTESIAN_POINT('Ctrl Pts',(1.97289186263272,1.,0.486502692907661));
#29796=CARTESIAN_POINT('Ctrl Pts',(1.96792703422358,-1.,0.482901662120687));
#29797=CARTESIAN_POINT('Ctrl Pts',(1.96792703422358,1.,0.482901662120687));
#29798=CARTESIAN_POINT('Ctrl Pts',(1.96294933055938,-1.,0.479349583074846));
#29799=CARTESIAN_POINT('Ctrl Pts',(1.96294933055938,1.,0.479349583074846));
#29800=CARTESIAN_POINT('Ctrl Pts',(1.95796111148175,-1.,0.475848034683172));
#29801=CARTESIAN_POINT('Ctrl Pts',(1.95796111148175,1.,0.475848034683172));
#29802=CARTESIAN_POINT('Ctrl Pts',(1.95296148278136,-1.,0.47239767226408));
#29803=CARTESIAN_POINT('Ctrl Pts',(1.95296148278136,1.,0.47239767226408));
#29804=CARTESIAN_POINT('Ctrl Pts',(1.94794381136524,-1.,0.468997482913158));
#29805=CARTESIAN_POINT('Ctrl Pts',(1.94794381136524,1.,0.468997482913158));
#29806=CARTESIAN_POINT('Ctrl Pts',(1.94289794196205,-1.,0.465645462026065));
#29807=CARTESIAN_POINT('Ctrl Pts',(1.94289794196205,1.,0.465645462026065));
#29808=CARTESIAN_POINT('Ctrl Pts',(1.93781486640834,-1.,0.462340031009087));
#29809=CARTESIAN_POINT('Ctrl Pts',(1.93781486640834,1.,0.462340031009087));
#29810=CARTESIAN_POINT('Ctrl Pts',(1.93269066517936,-1.,0.459081234547932));
#29811=CARTESIAN_POINT('Ctrl Pts',(1.93269066517936,1.,0.459081234547932));
#29812=CARTESIAN_POINT('Ctrl Pts',(1.92753067150461,-1.,0.455872005174336));
#29813=CARTESIAN_POINT('Ctrl Pts',(1.92753067150461,1.,0.455872005174336));
#29814=CARTESIAN_POINT('Ctrl Pts',(1.9223538064847,-1.,0.452719478359356));
#29815=CARTESIAN_POINT('Ctrl Pts',(1.9223538064847,1.,0.452719478359356));
#29816=CARTESIAN_POINT('Ctrl Pts',(1.91718342555717,-1.,0.449632260106572));
#29817=CARTESIAN_POINT('Ctrl Pts',(1.91718342555717,1.,0.449632260106572));
#29818=CARTESIAN_POINT('Ctrl Pts',(1.91203699981095,-1.,0.446617343485651));
#29819=CARTESIAN_POINT('Ctrl Pts',(1.91203699981095,1.,0.446617343485651));
#29820=CARTESIAN_POINT('Ctrl Pts',(1.90691756144906,-1.,0.443677556849171));
#29821=CARTESIAN_POINT('Ctrl Pts',(1.90691756144906,1.,0.443677556849171));
#29822=CARTESIAN_POINT('Ctrl Pts',(1.90180124389137,-1.,0.440807833704161));
#29823=CARTESIAN_POINT('Ctrl Pts',(1.90180124389137,1.,0.440807833704161));
#29824=CARTESIAN_POINT('Ctrl Pts',(1.89663648956549,-1.,0.437995003948443));
#29825=CARTESIAN_POINT('Ctrl Pts',(1.89663648956549,1.,0.437995003948443));
#29826=CARTESIAN_POINT('Ctrl Pts',(1.89136993975585,-1.,0.43522566096358));
#29827=CARTESIAN_POINT('Ctrl Pts',(1.89136993975585,1.,0.43522566096358));
#29828=CARTESIAN_POINT('Ctrl Pts',(1.88596913666828,-1.,0.432493038548833));
#29829=CARTESIAN_POINT('Ctrl Pts',(1.88596913666828,1.,0.432493038548833));
#29830=CARTESIAN_POINT('Ctrl Pts',(1.88044229001778,-1.,0.429803062482217));
#29831=CARTESIAN_POINT('Ctrl Pts',(1.88044229001778,1.,0.429803062482217));
#29832=CARTESIAN_POINT('Ctrl Pts',(1.87486989291333,-1.,0.427183828518743));
#29833=CARTESIAN_POINT('Ctrl Pts',(1.87486989291333,1.,0.427183828518743));
#29834=CARTESIAN_POINT('Ctrl Pts',(1.8693780394412,-1.,0.424678177290876));
#29835=CARTESIAN_POINT('Ctrl Pts',(1.8693780394412,1.,0.424678177290876));
#29836=CARTESIAN_POINT('Ctrl Pts',(1.86408083333863,-1.,0.422327307417885));
#29837=CARTESIAN_POINT('Ctrl Pts',(1.86408083333863,1.,0.422327307417885));
#29838=CARTESIAN_POINT('Ctrl Pts',(1.8590328109667,-1.,0.420157287975583));
#29839=CARTESIAN_POINT('Ctrl Pts',(1.8590328109667,1.,0.420157287975583));
#29840=CARTESIAN_POINT('Ctrl Pts',(1.8541763285645,-1.,0.418164129144046));
#29841=CARTESIAN_POINT('Ctrl Pts',(1.8541763285645,1.,0.418164129144046));
#29842=CARTESIAN_POINT('Ctrl Pts',(1.84929312930314,-1.,0.416300022039885));
#29843=CARTESIAN_POINT('Ctrl Pts',(1.84929312930314,1.,0.416300022039885));
#29844=CARTESIAN_POINT('Ctrl Pts',(1.84405757074218,-1.,0.414487438255542));
#29845=CARTESIAN_POINT('Ctrl Pts',(1.84405757074218,1.,0.414487438255542));
#29846=CARTESIAN_POINT('Ctrl Pts',(1.8380895347617,-1.,0.412633125322945));
#29847=CARTESIAN_POINT('Ctrl Pts',(1.8380895347617,1.,0.412633125322945));
#29848=CARTESIAN_POINT('Ctrl Pts',(1.83100408895047,-1.,0.410641256301276));
#29849=CARTESIAN_POINT('Ctrl Pts',(1.83100408895047,1.,0.410641256301276));
#29850=CARTESIAN_POINT('Ctrl Pts',(1.82247022677562,-1.,0.408428948106228));
#29851=CARTESIAN_POINT('Ctrl Pts',(1.82247022677562,1.,0.408428948106228));
#29852=CARTESIAN_POINT('Ctrl Pts',(1.81223801812013,-1.,0.405933518407176));
#29853=CARTESIAN_POINT('Ctrl Pts',(1.81223801812013,1.,0.405933518407176));
#29854=CARTESIAN_POINT('Ctrl Pts',(1.80012077173238,-1.,0.403107976163396));
#29855=CARTESIAN_POINT('Ctrl Pts',(1.80012077173238,1.,0.403107976163396));
#29856=CARTESIAN_POINT('Ctrl Pts',(1.78598826343754,-1.,0.399919403774156));
#29857=CARTESIAN_POINT('Ctrl Pts',(1.78598826343754,1.,0.399919403774156));
#29858=CARTESIAN_POINT('Ctrl Pts',(1.76975560043442,-1.,0.396346196110688));
#29859=CARTESIAN_POINT('Ctrl Pts',(1.76975560043442,1.,0.396346196110688));
#29860=CARTESIAN_POINT('Ctrl Pts',(1.75137405310193,-1.,0.392375812285396));
#29861=CARTESIAN_POINT('Ctrl Pts',(1.75137405310193,1.,0.392375812285396));
#29862=CARTESIAN_POINT('Ctrl Pts',(1.73493170972829,-1.,0.388877023502615));
#29863=CARTESIAN_POINT('Ctrl Pts',(1.73493170972829,1.,0.388877023502615));
#29864=CARTESIAN_POINT('Ctrl Pts',(1.72162022244582,-1.,0.386070790323281));
#29865=CARTESIAN_POINT('Ctrl Pts',(1.72162022244582,1.,0.386070790323281));
#29866=CARTESIAN_POINT('Ctrl Pts',(1.71231062891398,-1.,0.384119047314215));
#29867=CARTESIAN_POINT('Ctrl Pts',(1.71231062891398,1.,0.384119047314215));
#29868=CARTESIAN_POINT('Ctrl Pts',(1.7075470150345,-1.,0.383122945602004));
#29869=CARTESIAN_POINT('Ctrl Pts',(1.7075470150345,1.,0.383122945602004));
#29870=CARTESIAN_POINT('',(1.7075470150345,1.,0.383122945602004));
#29871=CARTESIAN_POINT('',(1.7075470150345,0.,0.383122945602005));
#29872=CARTESIAN_POINT('',(2.11275013067528,1.,0.613422273260091));
#29873=CARTESIAN_POINT('Ctrl Pts',(2.11275013067528,1.,0.613422273260091));
#29874=CARTESIAN_POINT('Ctrl Pts',(2.11187554260142,1.,0.61246736556225));
#29875=CARTESIAN_POINT('Ctrl Pts',(2.11012443807661,1.,0.610560911691114));
#29876=CARTESIAN_POINT('Ctrl Pts',(2.10749199615859,1.,0.607711315456826));
#29877=CARTESIAN_POINT('Ctrl Pts',(2.10397049887709,1.,0.603932030738212));
#29878=CARTESIAN_POINT('Ctrl Pts',(2.09954930865331,1.,0.599241616422144));
#29879=CARTESIAN_POINT('Ctrl Pts',(2.09510876220501,1.,0.594585006052824));
#29880=CARTESIAN_POINT('Ctrl Pts',(2.09064881812053,1.,0.58996236540319));
#29881=CARTESIAN_POINT('Ctrl Pts',(2.086169437277,1.,0.585373918990895));
#29882=CARTESIAN_POINT('Ctrl Pts',(2.08167059018138,1.,0.580819952107257));
#29883=CARTESIAN_POINT('Ctrl Pts',(2.07715226767361,1.,0.576300797416275));
#29884=CARTESIAN_POINT('Ctrl Pts',(2.07261449292757,1.,0.571816823242411));
#29885=CARTESIAN_POINT('Ctrl Pts',(2.06805732997383,1.,0.56736842118123));
#29886=CARTESIAN_POINT('Ctrl Pts',(2.06348090160697,1.,0.562955993082574));
#29887=CARTESIAN_POINT('Ctrl Pts',(2.05888537756571,1.,0.558579940185468));
#29888=CARTESIAN_POINT('Ctrl Pts',(2.05427091604482,1.,0.55424065746411));
#29889=CARTESIAN_POINT('Ctrl Pts',(2.04963761077974,1.,0.549938525150342));
#29890=CARTESIAN_POINT('Ctrl Pts',(2.0449854471456,1.,0.545673903817349));
#29891=CARTESIAN_POINT('Ctrl Pts',(2.0403142269048,1.,0.54144712061552));
#29892=CARTESIAN_POINT('Ctrl Pts',(2.03562362953993,1.,0.537258489833135));
#29893=CARTESIAN_POINT('Ctrl Pts',(2.03091336214401,1.,0.533108355132905));
#29894=CARTESIAN_POINT('Ctrl Pts',(2.02618329083289,1.,0.528997127241911));
#29895=CARTESIAN_POINT('Ctrl Pts',(2.02143356304712,1.,0.524925318333519));
#29896=CARTESIAN_POINT('Ctrl Pts',(2.01666477917305,1.,0.520893590399429));
#29897=CARTESIAN_POINT('Ctrl Pts',(2.01187773939257,1.,0.516902681728733));
#29898=CARTESIAN_POINT('Ctrl Pts',(2.00707309946955,1.,0.512953306961814));
#29899=CARTESIAN_POINT('Ctrl Pts',(2.00225107134733,1.,0.509046069886152));
#29900=CARTESIAN_POINT('Ctrl Pts',(1.99741107463567,1.,0.505181361323011));
#29901=CARTESIAN_POINT('Ctrl Pts',(1.9925514912615,1.,0.501359287727129));
#29902=CARTESIAN_POINT('Ctrl Pts',(1.98767044752929,1.,0.497579909545564));
#29903=CARTESIAN_POINT('Ctrl Pts',(1.9827665876182,1.,0.493843476541493));
#29904=CARTESIAN_POINT('Ctrl Pts',(1.97783973019229,1.,0.490150627860955));
#29905=CARTESIAN_POINT('Ctrl Pts',(1.97289186263272,1.,0.486502692907661));
#29906=CARTESIAN_POINT('Ctrl Pts',(1.96792703422358,1.,0.482901662120687));
#29907=CARTESIAN_POINT('Ctrl Pts',(1.96294933055938,1.,0.479349583074846));
#29908=CARTESIAN_POINT('Ctrl Pts',(1.95796111148175,1.,0.475848034683172));
#29909=CARTESIAN_POINT('Ctrl Pts',(1.95296148278136,1.,0.47239767226408));
#29910=CARTESIAN_POINT('Ctrl Pts',(1.94794381136524,1.,0.468997482913158));
#29911=CARTESIAN_POINT('Ctrl Pts',(1.94289794196205,1.,0.465645462026065));
#29912=CARTESIAN_POINT('Ctrl Pts',(1.93781486640834,1.,0.462340031009087));
#29913=CARTESIAN_POINT('Ctrl Pts',(1.93269066517936,1.,0.459081234547932));
#29914=CARTESIAN_POINT('Ctrl Pts',(1.92753067150461,1.,0.455872005174336));
#29915=CARTESIAN_POINT('Ctrl Pts',(1.9223538064847,1.,0.452719478359356));
#29916=CARTESIAN_POINT('Ctrl Pts',(1.91718342555717,1.,0.449632260106572));
#29917=CARTESIAN_POINT('Ctrl Pts',(1.91203699981095,1.,0.446617343485651));
#29918=CARTESIAN_POINT('Ctrl Pts',(1.90691756144906,1.,0.443677556849171));
#29919=CARTESIAN_POINT('Ctrl Pts',(1.90180124389137,1.,0.440807833704161));
#29920=CARTESIAN_POINT('Ctrl Pts',(1.89663648956549,1.,0.437995003948443));
#29921=CARTESIAN_POINT('Ctrl Pts',(1.89136993975585,1.,0.43522566096358));
#29922=CARTESIAN_POINT('Ctrl Pts',(1.88596913666828,1.,0.432493038548833));
#29923=CARTESIAN_POINT('Ctrl Pts',(1.88044229001778,1.,0.429803062482217));
#29924=CARTESIAN_POINT('Ctrl Pts',(1.87486989291333,1.,0.427183828518743));
#29925=CARTESIAN_POINT('Ctrl Pts',(1.8693780394412,1.,0.424678177290876));
#29926=CARTESIAN_POINT('Ctrl Pts',(1.86408083333863,1.,0.422327307417885));
#29927=CARTESIAN_POINT('Ctrl Pts',(1.8590328109667,1.,0.420157287975583));
#29928=CARTESIAN_POINT('Ctrl Pts',(1.8541763285645,1.,0.418164129144046));
#29929=CARTESIAN_POINT('Ctrl Pts',(1.84929312930314,1.,0.416300022039885));
#29930=CARTESIAN_POINT('Ctrl Pts',(1.84405757074218,1.,0.414487438255542));
#29931=CARTESIAN_POINT('Ctrl Pts',(1.8380895347617,1.,0.412633125322945));
#29932=CARTESIAN_POINT('Ctrl Pts',(1.83100408895047,1.,0.410641256301276));
#29933=CARTESIAN_POINT('Ctrl Pts',(1.82247022677562,1.,0.408428948106228));
#29934=CARTESIAN_POINT('Ctrl Pts',(1.81223801812013,1.,0.405933518407176));
#29935=CARTESIAN_POINT('Ctrl Pts',(1.80012077173238,1.,0.403107976163396));
#29936=CARTESIAN_POINT('Ctrl Pts',(1.78598826343754,1.,0.399919403774156));
#29937=CARTESIAN_POINT('Ctrl Pts',(1.76975560043442,1.,0.396346196110688));
#29938=CARTESIAN_POINT('Ctrl Pts',(1.75137405310193,1.,0.392375812285396));
#29939=CARTESIAN_POINT('Ctrl Pts',(1.73493170972829,1.,0.388877023502615));
#29940=CARTESIAN_POINT('Ctrl Pts',(1.72162022244582,1.,0.386070790323281));
#29941=CARTESIAN_POINT('Ctrl Pts',(1.71231062891398,1.,0.384119047314215));
#29942=CARTESIAN_POINT('Ctrl Pts',(1.7075470150345,1.,0.383122945602004));
#29943=CARTESIAN_POINT('',(2.11275013067528,0.,0.613422273260091));
#29944=CARTESIAN_POINT('Origin',(2.0698113262342,0.,0.745574324794401));
#29945=CARTESIAN_POINT('',(2.0698113262342,1.,0.745574324794401));
#29946=CARTESIAN_POINT('',(2.11275013067528,1.,0.613422273260091));
#29947=CARTESIAN_POINT('',(2.0698113262342,0.,0.745574324794401));
#29948=CARTESIAN_POINT('Ctrl Pts',(1.60662857109684,-1.,0.693717979106306));
#29949=CARTESIAN_POINT('Ctrl Pts',(1.60662857109684,1.,0.693717979106306));
#29950=CARTESIAN_POINT('Ctrl Pts',(1.61106790958151,-1.,0.695712097881194));
#29951=CARTESIAN_POINT('Ctrl Pts',(1.61106790958151,1.,0.695712097881194));
#29952=CARTESIAN_POINT('Ctrl Pts',(1.61974673472612,-1.,0.699605146405088));
#29953=CARTESIAN_POINT('Ctrl Pts',(1.61974673472612,1.,0.699605146405088));
#29954=CARTESIAN_POINT('Ctrl Pts',(1.63216541664676,-1.,0.705159151988319));
#29955=CARTESIAN_POINT('Ctrl Pts',(1.63216541664676,1.,0.705159151988319));
#29956=CARTESIAN_POINT('Ctrl Pts',(1.64752408832016,-1.,0.711993139355394));
#29957=CARTESIAN_POINT('Ctrl Pts',(1.64752408832016,1.,0.711993139355394));
#29958=CARTESIAN_POINT('Ctrl Pts',(1.6647288055568,-1.,0.719585433804282));
#29959=CARTESIAN_POINT('Ctrl Pts',(1.6647288055568,1.,0.719585433804282));
#29960=CARTESIAN_POINT('Ctrl Pts',(1.67996158455503,-1.,0.726235967997433));
#29961=CARTESIAN_POINT('Ctrl Pts',(1.67996158455503,1.,0.726235967997433));
#29962=CARTESIAN_POINT('Ctrl Pts',(1.69326921975743,-1.,0.731963238697195));
#29963=CARTESIAN_POINT('Ctrl Pts',(1.69326921975743,1.,0.731963238697195));
#29964=CARTESIAN_POINT('Ctrl Pts',(1.70473309006121,-1.,0.736799665724771));
#29965=CARTESIAN_POINT('Ctrl Pts',(1.70473309006121,1.,0.736799665724771));
#29966=CARTESIAN_POINT('Ctrl Pts',(1.71447789751927,-1.,0.740795162032088));
#29967=CARTESIAN_POINT('Ctrl Pts',(1.71447789751927,1.,0.740795162032088));
#29968=CARTESIAN_POINT('Ctrl Pts',(1.7226822991693,-1.,0.744021445433765));
#29969=CARTESIAN_POINT('Ctrl Pts',(1.7226822991693,1.,0.744021445433765));
#29970=CARTESIAN_POINT('Ctrl Pts',(1.72958533647399,-1.,0.746574710096437));
#29971=CARTESIAN_POINT('Ctrl Pts',(1.72958533647399,1.,0.746574710096437));
#29972=CARTESIAN_POINT('Ctrl Pts',(1.73550351679848,-1.,0.748582462954855));
#29973=CARTESIAN_POINT('Ctrl Pts',(1.73550351679848,1.,0.748582462954855));
#29974=CARTESIAN_POINT('Ctrl Pts',(1.74080458266705,-1.,0.750193435979541));
#29975=CARTESIAN_POINT('Ctrl Pts',(1.74080458266705,1.,0.750193435979541));
#29976=CARTESIAN_POINT('Ctrl Pts',(1.74585086852298,-1.,0.751555614163629));
#29977=CARTESIAN_POINT('Ctrl Pts',(1.74585086852298,1.,0.751555614163629));
#29978=CARTESIAN_POINT('Ctrl Pts',(1.75095139468809,-1.,0.752797683531377));
#29979=CARTESIAN_POINT('Ctrl Pts',(1.75095139468809,1.,0.752797683531377));
#29980=CARTESIAN_POINT('Ctrl Pts',(1.75631083600175,-1.,0.75400925402848));
#29981=CARTESIAN_POINT('Ctrl Pts',(1.75631083600175,1.,0.75400925402848));
#29982=CARTESIAN_POINT('Ctrl Pts',(1.7619781724032,-1.,0.755220979975262));
#29983=CARTESIAN_POINT('Ctrl Pts',(1.7619781724032,1.,0.755220979975262));
#29984=CARTESIAN_POINT('Ctrl Pts',(1.76789396003141,-1.,0.756421896028403));
#29985=CARTESIAN_POINT('Ctrl Pts',(1.76789396003141,1.,0.756421896028403));
#29986=CARTESIAN_POINT('Ctrl Pts',(1.77394167108342,-1.,0.757578264077238));
#29987=CARTESIAN_POINT('Ctrl Pts',(1.77394167108342,1.,0.757578264077238));
#29988=CARTESIAN_POINT('Ctrl Pts',(1.77999411220912,-1.,0.75865062667738));
#29989=CARTESIAN_POINT('Ctrl Pts',(1.77999411220912,1.,0.75865062667738));
#29990=CARTESIAN_POINT('Ctrl Pts',(1.78596964884526,-1.,0.759614401109868));
#29991=CARTESIAN_POINT('Ctrl Pts',(1.78596964884526,1.,0.759614401109868));
#29992=CARTESIAN_POINT('Ctrl Pts',(1.79185815610802,-1.,0.760469555880425));
#29993=CARTESIAN_POINT('Ctrl Pts',(1.79185815610802,1.,0.760469555880425));
#29994=CARTESIAN_POINT('Ctrl Pts',(1.79768986997735,-1.,0.761229695230359));
#29995=CARTESIAN_POINT('Ctrl Pts',(1.79768986997735,1.,0.761229695230359));
#29996=CARTESIAN_POINT('Ctrl Pts',(1.80351583877334,-1.,0.761915336443516));
#29997=CARTESIAN_POINT('Ctrl Pts',(1.80351583877334,1.,0.761915336443516));
#29998=CARTESIAN_POINT('Ctrl Pts',(1.80938551463989,-1.,0.762546129464036));
#29999=CARTESIAN_POINT('Ctrl Pts',(1.80938551463989,1.,0.762546129464036));
#30000=CARTESIAN_POINT('Ctrl Pts',(1.81532118405566,-1.,0.763132003836783));
#30001=CARTESIAN_POINT('Ctrl Pts',(1.81532118405566,1.,0.763132003836783));
#30002=CARTESIAN_POINT('Ctrl Pts',(1.82131873145297,-1.,0.763673465462854));
#30003=CARTESIAN_POINT('Ctrl Pts',(1.82131873145297,1.,0.763673465462854));
#30004=CARTESIAN_POINT('Ctrl Pts',(1.8273599120008,-1.,0.764165902606056));
#30005=CARTESIAN_POINT('Ctrl Pts',(1.8273599120008,1.,0.764165902606056));
#30006=CARTESIAN_POINT('Ctrl Pts',(1.8334207722714,-1.,0.764602549687846));
#30007=CARTESIAN_POINT('Ctrl Pts',(1.8334207722714,1.,0.764602549687846));
#30008=CARTESIAN_POINT('Ctrl Pts',(1.83948181064823,-1.,0.764978057881688));
#30009=CARTESIAN_POINT('Ctrl Pts',(1.83948181064823,1.,0.764978057881688));
#30010=CARTESIAN_POINT('Ctrl Pts',(1.8455369887591,-1.,0.765291664861972));
#30011=CARTESIAN_POINT('Ctrl Pts',(1.8455369887591,1.,0.765291664861972));
#30012=CARTESIAN_POINT('Ctrl Pts',(1.85158945130054,-1.,0.765545710619023));
#30013=CARTESIAN_POINT('Ctrl Pts',(1.85158945130054,1.,0.765545710619023));
#30014=CARTESIAN_POINT('Ctrl Pts',(1.85764741390391,-1.,0.765744212909305));
#30015=CARTESIAN_POINT('Ctrl Pts',(1.85764741390391,1.,0.765744212909305));
#30016=CARTESIAN_POINT('Ctrl Pts',(1.86372027063314,-1.,0.765891519092557));
#30017=CARTESIAN_POINT('Ctrl Pts',(1.86372027063314,1.,0.765891519092557));
#30018=CARTESIAN_POINT('Ctrl Pts',(1.86981398314345,-1.,0.765990708546112));
#30019=CARTESIAN_POINT('Ctrl Pts',(1.86981398314345,1.,0.765990708546112));
#30020=CARTESIAN_POINT('Ctrl Pts',(1.87592888967886,-1.,0.766042837036759));
#30021=CARTESIAN_POINT('Ctrl Pts',(1.87592888967886,1.,0.766042837036759));
#30022=CARTESIAN_POINT('Ctrl Pts',(1.88206215302561,-1.,0.766047794851869));
#30023=CARTESIAN_POINT('Ctrl Pts',(1.88206215302561,1.,0.766047794851869));
#30024=CARTESIAN_POINT('Ctrl Pts',(1.88820926433409,-1.,0.76600483706209));
#30025=CARTESIAN_POINT('Ctrl Pts',(1.88820926433409,1.,0.76600483706209));
#30026=CARTESIAN_POINT('Ctrl Pts',(1.89436577771389,-1.,0.765913193856979));
#30027=CARTESIAN_POINT('Ctrl Pts',(1.89436577771389,1.,0.765913193856979));
#30028=CARTESIAN_POINT('Ctrl Pts',(1.90052930393599,-1.,0.765772772593395));
#30029=CARTESIAN_POINT('Ctrl Pts',(1.90052930393599,1.,0.765772772593395));
#30030=CARTESIAN_POINT('Ctrl Pts',(1.90669961402362,-1.,0.765584196937937));
#30031=CARTESIAN_POINT('Ctrl Pts',(1.90669961402362,1.,0.765584196937937));
#30032=CARTESIAN_POINT('Ctrl Pts',(1.91287765805174,-1.,0.765348465884739));
#30033=CARTESIAN_POINT('Ctrl Pts',(1.91287765805174,1.,0.765348465884739));
#30034=CARTESIAN_POINT('Ctrl Pts',(1.91906491634197,-1.,0.765066729667095));
#30035=CARTESIAN_POINT('Ctrl Pts',(1.91906491634197,1.,0.765066729667095));
#30036=CARTESIAN_POINT('Ctrl Pts',(1.92526263537041,-1.,0.764740025488189));
#30037=CARTESIAN_POINT('Ctrl Pts',(1.92526263537041,1.,0.764740025488189));
#30038=CARTESIAN_POINT('Ctrl Pts',(1.93147105496367,-1.,0.76436901067389));
#30039=CARTESIAN_POINT('Ctrl Pts',(1.93147105496367,1.,0.76436901067389));
#30040=CARTESIAN_POINT('Ctrl Pts',(1.93768964875867,-1.,0.763954049121394));
#30041=CARTESIAN_POINT('Ctrl Pts',(1.93768964875867,1.,0.763954049121394));
#30042=CARTESIAN_POINT('Ctrl Pts',(1.94391746617626,-1.,0.763495333538581));
#30043=CARTESIAN_POINT('Ctrl Pts',(1.94391746617626,1.,0.763495333538581));
#30044=CARTESIAN_POINT('Ctrl Pts',(1.95015342590025,-1.,0.762992990878774));
#30045=CARTESIAN_POINT('Ctrl Pts',(1.95015342590025,1.,0.762992990878774));
#30046=CARTESIAN_POINT('Ctrl Pts',(1.95639665309893,-1.,0.762447203806264));
#30047=CARTESIAN_POINT('Ctrl Pts',(1.95639665309893,1.,0.762447203806264));
#30048=CARTESIAN_POINT('Ctrl Pts',(1.96264672744229,-1.,0.761858300014575));
#30049=CARTESIAN_POINT('Ctrl Pts',(1.96264672744229,1.,0.761858300014575));
#30050=CARTESIAN_POINT('Ctrl Pts',(1.96890351582545,-1.,0.761226690483986));
#30051=CARTESIAN_POINT('Ctrl Pts',(1.96890351582545,1.,0.761226690483986));
#30052=CARTESIAN_POINT('Ctrl Pts',(1.97516705321521,-1.,0.760552825409856));
#30053=CARTESIAN_POINT('Ctrl Pts',(1.97516705321521,1.,0.760552825409856));
#30054=CARTESIAN_POINT('Ctrl Pts',(1.98143741418156,-1.,0.759837147452135));
#30055=CARTESIAN_POINT('Ctrl Pts',(1.98143741418156,1.,0.759837147452135));
#30056=CARTESIAN_POINT('Ctrl Pts',(1.98771456680806,-1.,0.759080037802243));
#30057=CARTESIAN_POINT('Ctrl Pts',(1.98771456680806,1.,0.759080037802243));
#30058=CARTESIAN_POINT('Ctrl Pts',(1.9939983109871,-1.,0.758281796766377));
#30059=CARTESIAN_POINT('Ctrl Pts',(1.9939983109871,1.,0.758281796766377));
#30060=CARTESIAN_POINT('Ctrl Pts',(2.00028834739072,-1.,0.757442676862342));
#30061=CARTESIAN_POINT('Ctrl Pts',(2.00028834739072,1.,0.757442676862342));
#30062=CARTESIAN_POINT('Ctrl Pts',(2.00658431587682,-1.,0.756562904646496));
#30063=CARTESIAN_POINT('Ctrl Pts',(2.00658431587682,1.,0.756562904646496));
#30064=CARTESIAN_POINT('Ctrl Pts',(2.01288584328149,-1.,0.755642704958101));
#30065=CARTESIAN_POINT('Ctrl Pts',(2.01288584328149,1.,0.755642704958101));
#30066=CARTESIAN_POINT('Ctrl Pts',(2.01919259406003,-1.,0.75468233072352));
#30067=CARTESIAN_POINT('Ctrl Pts',(2.01919259406003,1.,0.75468233072352));
#30068=CARTESIAN_POINT('Ctrl Pts',(2.02550428623587,-1.,0.753682061113766));
#30069=CARTESIAN_POINT('Ctrl Pts',(2.02550428623587,1.,0.753682061113766));
#30070=CARTESIAN_POINT('Ctrl Pts',(2.03182068456467,-1.,0.752642180488104));
#30071=CARTESIAN_POINT('Ctrl Pts',(2.03182068456467,1.,0.752642180488104));
#30072=CARTESIAN_POINT('Ctrl Pts',(2.03814160092173,-1.,0.751562963361384));
#30073=CARTESIAN_POINT('Ctrl Pts',(2.03814160092173,1.,0.751562963361384));
#30074=CARTESIAN_POINT('Ctrl Pts',(2.04446689147754,-1.,0.750444657874758));
#30075=CARTESIAN_POINT('Ctrl Pts',(2.04446689147754,1.,0.750444657874758));
#30076=CARTESIAN_POINT('Ctrl Pts',(2.05079645591606,-1.,0.749287468663053));
#30077=CARTESIAN_POINT('Ctrl Pts',(2.05079645591606,1.,0.749287468663053));
#30078=CARTESIAN_POINT('Ctrl Pts',(2.05713023030263,-1.,0.748091554181101));
#30079=CARTESIAN_POINT('Ctrl Pts',(2.05713023030263,1.,0.748091554181101));
#30080=CARTESIAN_POINT('Ctrl Pts',(2.06220058927162,-1.,0.747103932785504));
#30081=CARTESIAN_POINT('Ctrl Pts',(2.06220058927162,1.,0.747103932785504));
#30082=CARTESIAN_POINT('Ctrl Pts',(2.06600523016401,-1.,0.746345871542696));
#30083=CARTESIAN_POINT('Ctrl Pts',(2.06600523016401,1.,0.746345871542696));
#30084=CARTESIAN_POINT('Ctrl Pts',(2.06854248895575,-1.,0.74583279137781));
#30085=CARTESIAN_POINT('Ctrl Pts',(2.06854248895575,1.,0.74583279137781));
#30086=CARTESIAN_POINT('Ctrl Pts',(2.0698113262342,-1.,0.745574324794401));
#30087=CARTESIAN_POINT('Ctrl Pts',(2.0698113262342,1.,0.745574324794401));
#30088=CARTESIAN_POINT('',(1.60662857109684,1.,0.693717979106306));
#30089=CARTESIAN_POINT('Ctrl Pts',(1.60662857109684,1.,0.693717979106306));
#30090=CARTESIAN_POINT('Ctrl Pts',(1.61106790958151,1.,0.695712097881194));
#30091=CARTESIAN_POINT('Ctrl Pts',(1.61974673472612,1.,0.699605146405088));
#30092=CARTESIAN_POINT('Ctrl Pts',(1.63216541664676,1.,0.705159151988319));
#30093=CARTESIAN_POINT('Ctrl Pts',(1.64752408832016,1.,0.711993139355394));
#30094=CARTESIAN_POINT('Ctrl Pts',(1.6647288055568,1.,0.719585433804282));
#30095=CARTESIAN_POINT('Ctrl Pts',(1.67996158455503,1.,0.726235967997433));
#30096=CARTESIAN_POINT('Ctrl Pts',(1.69326921975743,1.,0.731963238697195));
#30097=CARTESIAN_POINT('Ctrl Pts',(1.70473309006121,1.,0.736799665724771));
#30098=CARTESIAN_POINT('Ctrl Pts',(1.71447789751927,1.,0.740795162032088));
#30099=CARTESIAN_POINT('Ctrl Pts',(1.7226822991693,1.,0.744021445433765));
#30100=CARTESIAN_POINT('Ctrl Pts',(1.72958533647399,1.,0.746574710096437));
#30101=CARTESIAN_POINT('Ctrl Pts',(1.73550351679848,1.,0.748582462954855));
#30102=CARTESIAN_POINT('Ctrl Pts',(1.74080458266705,1.,0.750193435979541));
#30103=CARTESIAN_POINT('Ctrl Pts',(1.74585086852298,1.,0.751555614163629));
#30104=CARTESIAN_POINT('Ctrl Pts',(1.75095139468809,1.,0.752797683531377));
#30105=CARTESIAN_POINT('Ctrl Pts',(1.75631083600175,1.,0.75400925402848));
#30106=CARTESIAN_POINT('Ctrl Pts',(1.7619781724032,1.,0.755220979975262));
#30107=CARTESIAN_POINT('Ctrl Pts',(1.76789396003141,1.,0.756421896028403));
#30108=CARTESIAN_POINT('Ctrl Pts',(1.77394167108342,1.,0.757578264077238));
#30109=CARTESIAN_POINT('Ctrl Pts',(1.77999411220912,1.,0.75865062667738));
#30110=CARTESIAN_POINT('Ctrl Pts',(1.78596964884526,1.,0.759614401109868));
#30111=CARTESIAN_POINT('Ctrl Pts',(1.79185815610802,1.,0.760469555880425));
#30112=CARTESIAN_POINT('Ctrl Pts',(1.79768986997735,1.,0.761229695230359));
#30113=CARTESIAN_POINT('Ctrl Pts',(1.80351583877334,1.,0.761915336443516));
#30114=CARTESIAN_POINT('Ctrl Pts',(1.80938551463989,1.,0.762546129464036));
#30115=CARTESIAN_POINT('Ctrl Pts',(1.81532118405566,1.,0.763132003836783));
#30116=CARTESIAN_POINT('Ctrl Pts',(1.82131873145297,1.,0.763673465462854));
#30117=CARTESIAN_POINT('Ctrl Pts',(1.8273599120008,1.,0.764165902606056));
#30118=CARTESIAN_POINT('Ctrl Pts',(1.8334207722714,1.,0.764602549687846));
#30119=CARTESIAN_POINT('Ctrl Pts',(1.83948181064823,1.,0.764978057881688));
#30120=CARTESIAN_POINT('Ctrl Pts',(1.8455369887591,1.,0.765291664861972));
#30121=CARTESIAN_POINT('Ctrl Pts',(1.85158945130054,1.,0.765545710619023));
#30122=CARTESIAN_POINT('Ctrl Pts',(1.85764741390391,1.,0.765744212909305));
#30123=CARTESIAN_POINT('Ctrl Pts',(1.86372027063314,1.,0.765891519092557));
#30124=CARTESIAN_POINT('Ctrl Pts',(1.86981398314345,1.,0.765990708546112));
#30125=CARTESIAN_POINT('Ctrl Pts',(1.87592888967886,1.,0.766042837036759));
#30126=CARTESIAN_POINT('Ctrl Pts',(1.88206215302561,1.,0.766047794851869));
#30127=CARTESIAN_POINT('Ctrl Pts',(1.88820926433409,1.,0.76600483706209));
#30128=CARTESIAN_POINT('Ctrl Pts',(1.89436577771389,1.,0.765913193856979));
#30129=CARTESIAN_POINT('Ctrl Pts',(1.90052930393599,1.,0.765772772593395));
#30130=CARTESIAN_POINT('Ctrl Pts',(1.90669961402362,1.,0.765584196937937));
#30131=CARTESIAN_POINT('Ctrl Pts',(1.91287765805174,1.,0.765348465884739));
#30132=CARTESIAN_POINT('Ctrl Pts',(1.91906491634197,1.,0.765066729667095));
#30133=CARTESIAN_POINT('Ctrl Pts',(1.92526263537041,1.,0.764740025488189));
#30134=CARTESIAN_POINT('Ctrl Pts',(1.93147105496367,1.,0.76436901067389));
#30135=CARTESIAN_POINT('Ctrl Pts',(1.93768964875867,1.,0.763954049121394));
#30136=CARTESIAN_POINT('Ctrl Pts',(1.94391746617626,1.,0.763495333538581));
#30137=CARTESIAN_POINT('Ctrl Pts',(1.95015342590025,1.,0.762992990878774));
#30138=CARTESIAN_POINT('Ctrl Pts',(1.95639665309893,1.,0.762447203806264));
#30139=CARTESIAN_POINT('Ctrl Pts',(1.96264672744229,1.,0.761858300014575));
#30140=CARTESIAN_POINT('Ctrl Pts',(1.96890351582545,1.,0.761226690483986));
#30141=CARTESIAN_POINT('Ctrl Pts',(1.97516705321521,1.,0.760552825409856));
#30142=CARTESIAN_POINT('Ctrl Pts',(1.98143741418156,1.,0.759837147452135));
#30143=CARTESIAN_POINT('Ctrl Pts',(1.98771456680806,1.,0.759080037802243));
#30144=CARTESIAN_POINT('Ctrl Pts',(1.9939983109871,1.,0.758281796766377));
#30145=CARTESIAN_POINT('Ctrl Pts',(2.00028834739072,1.,0.757442676862342));
#30146=CARTESIAN_POINT('Ctrl Pts',(2.00658431587682,1.,0.756562904646496));
#30147=CARTESIAN_POINT('Ctrl Pts',(2.01288584328149,1.,0.755642704958101));
#30148=CARTESIAN_POINT('Ctrl Pts',(2.01919259406003,1.,0.75468233072352));
#30149=CARTESIAN_POINT('Ctrl Pts',(2.02550428623587,1.,0.753682061113766));
#30150=CARTESIAN_POINT('Ctrl Pts',(2.03182068456467,1.,0.752642180488104));
#30151=CARTESIAN_POINT('Ctrl Pts',(2.03814160092173,1.,0.751562963361384));
#30152=CARTESIAN_POINT('Ctrl Pts',(2.04446689147754,1.,0.750444657874758));
#30153=CARTESIAN_POINT('Ctrl Pts',(2.05079645591606,1.,0.749287468663053));
#30154=CARTESIAN_POINT('Ctrl Pts',(2.05713023030263,1.,0.748091554181101));
#30155=CARTESIAN_POINT('Ctrl Pts',(2.06220058927162,1.,0.747103932785504));
#30156=CARTESIAN_POINT('Ctrl Pts',(2.06600523016401,1.,0.746345871542696));
#30157=CARTESIAN_POINT('Ctrl Pts',(2.06854248895575,1.,0.74583279137781));
#30158=CARTESIAN_POINT('Ctrl Pts',(2.0698113262342,1.,0.745574324794401));
#30159=CARTESIAN_POINT('',(1.60662857109684,0.,0.693717979106305));
#30160=CARTESIAN_POINT('Origin',(0.,0.,0.));
#30161=CARTESIAN_POINT('',(1.5055822144029,1.,0.892032620296856));
#30162=CARTESIAN_POINT('Origin',(0.,1.,0.));
#30163=CARTESIAN_POINT('',(1.5055822144029,0.,0.892032620296855));
#30164=CARTESIAN_POINT('Ctrl Pts',(1.81978687191668,-1.,1.23627494547115));
#30165=CARTESIAN_POINT('Ctrl Pts',(1.81978687191668,1.,1.23627494547115));
#30166=CARTESIAN_POINT('Ctrl Pts',(1.81925017193666,-1.,1.23509651170476));
#30167=CARTESIAN_POINT('Ctrl Pts',(1.81925017193666,1.,1.23509651170476));
#30168=CARTESIAN_POINT('Ctrl Pts',(1.81817389921279,-1.,1.2327422452705));
#30169=CARTESIAN_POINT('Ctrl Pts',(1.81817389921279,1.,1.2327422452705));
#30170=CARTESIAN_POINT('Ctrl Pts',(1.8165508718364,-1.,1.2292186489137));
#30171=CARTESIAN_POINT('Ctrl Pts',(1.8165508718364,1.,1.2292186489137));
#30172=CARTESIAN_POINT('Ctrl Pts',(1.81436959210434,-1.,1.2245361330495));
#30173=CARTESIAN_POINT('Ctrl Pts',(1.81436959210434,1.,1.2245361330495));
#30174=CARTESIAN_POINT('Ctrl Pts',(1.81161420806656,-1.,1.21870906103557));
#30175=CARTESIAN_POINT('Ctrl Pts',(1.81161420806656,1.,1.21870906103557));
#30176=CARTESIAN_POINT('Ctrl Pts',(1.80882996917129,-1.,1.21290815708314));
#30177=CARTESIAN_POINT('Ctrl Pts',(1.80882996917129,1.,1.21290815708314));
#30178=CARTESIAN_POINT('Ctrl Pts',(1.80601678480707,-1.,1.20713356605475));
#30179=CARTESIAN_POINT('Ctrl Pts',(1.80601678480707,1.,1.20713356605475));
#30180=CARTESIAN_POINT('Ctrl Pts',(1.80317454838603,-1.,1.20138548938974));
#30181=CARTESIAN_POINT('Ctrl Pts',(1.80317454838603,1.,1.20138548938974));
#30182=CARTESIAN_POINT('Ctrl Pts',(1.80030314369879,-1.,1.19566418930242));
#30183=CARTESIAN_POINT('Ctrl Pts',(1.80030314369879,1.,1.19566418930242));
#30184=CARTESIAN_POINT('Ctrl Pts',(1.79740245923478,-1.,1.18996997934445));
#30185=CARTESIAN_POINT('Ctrl Pts',(1.79740245923478,1.,1.18996997934445));
#30186=CARTESIAN_POINT('Ctrl Pts',(1.79447240321515,-1.,1.18430321697432));
#30187=CARTESIAN_POINT('Ctrl Pts',(1.79447240321515,1.,1.18430321697432));
#30188=CARTESIAN_POINT('Ctrl Pts',(1.79151291552689,-1.,1.17866429440809));
#30189=CARTESIAN_POINT('Ctrl Pts',(1.79151291552689,1.,1.17866429440809));
#30190=CARTESIAN_POINT('Ctrl Pts',(1.78852398877616,-1.,1.17305363177328));
#30191=CARTESIAN_POINT('Ctrl Pts',(1.78852398877616,1.,1.17305363177328));
#30192=CARTESIAN_POINT('Ctrl Pts',(1.78550566040443,-1.,1.16747166312303));
#30193=CARTESIAN_POINT('Ctrl Pts',(1.78550566040443,1.,1.16747166312303));
#30194=CARTESIAN_POINT('Ctrl Pts',(1.78245795881009,-1.,1.16191881298499));
#30195=CARTESIAN_POINT('Ctrl Pts',(1.78245795881009,1.,1.16191881298499));
#30196=CARTESIAN_POINT('Ctrl Pts',(1.77938085564275,-1.,1.15639547194698));
#30197=CARTESIAN_POINT('Ctrl Pts',(1.77938085564275,1.,1.15639547194698));
#30198=CARTESIAN_POINT('Ctrl Pts',(1.7762742255701,-1.,1.15090197841515));
#30199=CARTESIAN_POINT('Ctrl Pts',(1.7762742255701,1.,1.15090197841515));
#30200=CARTESIAN_POINT('Ctrl Pts',(1.77313777896194,-1.,1.1454385822692));
#30201=CARTESIAN_POINT('Ctrl Pts',(1.77313777896194,1.,1.1454385822692));
#30202=CARTESIAN_POINT('Ctrl Pts',(1.76997111386769,-1.,1.14000548336975));
#30203=CARTESIAN_POINT('Ctrl Pts',(1.76997111386769,1.,1.14000548336975));
#30204=CARTESIAN_POINT('Ctrl Pts',(1.76677384551862,-1.,1.1346029180462));
#30205=CARTESIAN_POINT('Ctrl Pts',(1.76677384551862,1.,1.1346029180462));
#30206=CARTESIAN_POINT('Ctrl Pts',(1.7635457196617,-1.,1.12923123555075));
#30207=CARTESIAN_POINT('Ctrl Pts',(1.7635457196617,1.,1.12923123555075));
#30208=CARTESIAN_POINT('Ctrl Pts',(1.76028671825096,-1.,1.12389096855086));
#30209=CARTESIAN_POINT('Ctrl Pts',(1.76028671825096,1.,1.12389096855086));
#30210=CARTESIAN_POINT('Ctrl Pts',(1.75699720772105,-1.,1.11858293216763));
#30211=CARTESIAN_POINT('Ctrl Pts',(1.75699720772105,1.,1.11858293216763));
#30212=CARTESIAN_POINT('Ctrl Pts',(1.7536777209463,-1.,1.11330807582551));
#30213=CARTESIAN_POINT('Ctrl Pts',(1.7536777209463,1.,1.11330807582551));
#30214=CARTESIAN_POINT('Ctrl Pts',(1.7503286607592,-1.,1.10806728183007));
#30215=CARTESIAN_POINT('Ctrl Pts',(1.7503286607592,1.,1.10806728183007));
#30216=CARTESIAN_POINT('Ctrl Pts',(1.74695004214923,-1.,1.10286118991143));
#30217=CARTESIAN_POINT('Ctrl Pts',(1.74695004214923,1.,1.10286118991143));
#30218=CARTESIAN_POINT('Ctrl Pts',(1.74354119236208,-1.,1.09768999241226));
#30219=CARTESIAN_POINT('Ctrl Pts',(1.74354119236208,1.,1.09768999241226));
#30220=CARTESIAN_POINT('Ctrl Pts',(1.74010053962247,-1.,1.09255329056493));
#30221=CARTESIAN_POINT('Ctrl Pts',(1.74010053962247,1.,1.09255329056493));
#30222=CARTESIAN_POINT('Ctrl Pts',(1.73662628326091,-1.,1.08745056285427));
#30223=CARTESIAN_POINT('Ctrl Pts',(1.73662628326091,1.,1.08745056285427));
#30224=CARTESIAN_POINT('Ctrl Pts',(1.73311705663407,-1.,1.08238162784749));
#30225=CARTESIAN_POINT('Ctrl Pts',(1.73311705663407,1.,1.08238162784749));
#30226=CARTESIAN_POINT('Ctrl Pts',(1.72957248977424,-1.,1.0773470373727));
#30227=CARTESIAN_POINT('Ctrl Pts',(1.72957248977424,1.,1.0773470373727));
#30228=CARTESIAN_POINT('Ctrl Pts',(1.72599406198488,-1.,1.07234866990252));
#30229=CARTESIAN_POINT('Ctrl Pts',(1.72599406198488,1.,1.07234866990252));
#30230=CARTESIAN_POINT('Ctrl Pts',(1.72238500928453,-1.,1.06738966975462));
#30231=CARTESIAN_POINT('Ctrl Pts',(1.72238500928453,1.,1.06738966975462));
#30232=CARTESIAN_POINT('Ctrl Pts',(1.71874858456904,-1.,1.06247324680647));
#30233=CARTESIAN_POINT('Ctrl Pts',(1.71874858456904,1.,1.06247324680647));
#30234=CARTESIAN_POINT('Ctrl Pts',(1.7150865442702,-1.,1.05760163192479));
#30235=CARTESIAN_POINT('Ctrl Pts',(1.7150865442702,1.,1.05760163192479));
#30236=CARTESIAN_POINT('Ctrl Pts',(1.71139783543989,-1.,1.05277517202855));
#30237=CARTESIAN_POINT('Ctrl Pts',(1.71139783543989,1.,1.05277517202855));
#30238=CARTESIAN_POINT('Ctrl Pts',(1.70767646263649,-1.,1.04799085404995));
#30239=CARTESIAN_POINT('Ctrl Pts',(1.70767646263649,1.,1.04799085404995));
#30240=CARTESIAN_POINT('Ctrl Pts',(1.70391338707982,-1.,1.04324363334554));
#30241=CARTESIAN_POINT('Ctrl Pts',(1.70391338707982,1.,1.04324363334554));
#30242=CARTESIAN_POINT('Ctrl Pts',(1.70010052930962,-1.,1.03852922490789));
#30243=CARTESIAN_POINT('Ctrl Pts',(1.70010052930962,1.,1.03852922490789));
#30244=CARTESIAN_POINT('Ctrl Pts',(1.69623414782771,-1.,1.03384646003588));
#30245=CARTESIAN_POINT('Ctrl Pts',(1.69623414782771,1.,1.03384646003588));
#30246=CARTESIAN_POINT('Ctrl Pts',(1.69231840863458,-1.,1.02919977579147));
#30247=CARTESIAN_POINT('Ctrl Pts',(1.69231840863458,1.,1.02919977579147));
#30248=CARTESIAN_POINT('Ctrl Pts',(1.68836910178447,-1.,1.02460180535255));
#30249=CARTESIAN_POINT('Ctrl Pts',(1.68836910178447,1.,1.02460180535255));
#30250=CARTESIAN_POINT('Ctrl Pts',(1.68440578021706,-1.,1.02006795074201));
#30251=CARTESIAN_POINT('Ctrl Pts',(1.68440578021706,1.,1.02006795074201));
#30252=CARTESIAN_POINT('Ctrl Pts',(1.68044289894798,-1.,1.01561026162773));
#30253=CARTESIAN_POINT('Ctrl Pts',(1.68044289894798,1.,1.01561026162773));
#30254=CARTESIAN_POINT('Ctrl Pts',(1.67648246776464,-1.,1.01123236493511));
#30255=CARTESIAN_POINT('Ctrl Pts',(1.67648246776464,1.,1.01123236493511));
#30256=CARTESIAN_POINT('Ctrl Pts',(1.67250335383293,-1.,1.00692206696414));
#30257=CARTESIAN_POINT('Ctrl Pts',(1.67250335383293,1.,1.00692206696414));
#30258=CARTESIAN_POINT('Ctrl Pts',(1.66846059277303,-1.,1.00265091003727));
#30259=CARTESIAN_POINT('Ctrl Pts',(1.66846059277303,1.,1.00265091003727));
#30260=CARTESIAN_POINT('Ctrl Pts',(1.66430758030376,-1.,0.998389654952758));
#30261=CARTESIAN_POINT('Ctrl Pts',(1.66430758030376,1.,0.998389654952758));
#30262=CARTESIAN_POINT('Ctrl Pts',(1.66001553809947,-1.,0.994121836661306));
#30263=CARTESIAN_POINT('Ctrl Pts',(1.66001553809947,1.,0.994121836661306));
#30264=CARTESIAN_POINT('Ctrl Pts',(1.65559044289699,-1.,0.989855627854165));
#30265=CARTESIAN_POINT('Ctrl Pts',(1.65559044289699,1.,0.989855627854165));
#30266=CARTESIAN_POINT('Ctrl Pts',(1.65110016612638,-1.,0.985642622920821));
#30267=CARTESIAN_POINT('Ctrl Pts',(1.65110016612638,1.,0.985642622920821));
#30268=CARTESIAN_POINT('Ctrl Pts',(1.64665139190656,-1.,0.981562530939489));
#30269=CARTESIAN_POINT('Ctrl Pts',(1.64665139190656,1.,0.981562530939489));
#30270=CARTESIAN_POINT('Ctrl Pts',(1.64233990826687,-1.,0.977689794119417));
#30271=CARTESIAN_POINT('Ctrl Pts',(1.64233990826687,1.,0.977689794119417));
#30272=CARTESIAN_POINT('Ctrl Pts',(1.63820952658144,-1.,0.974066058287419));
#30273=CARTESIAN_POINT('Ctrl Pts',(1.63820952658144,1.,0.974066058287419));
#30274=CARTESIAN_POINT('Ctrl Pts',(1.63420665729798,-1.,0.970669715997509));
#30275=CARTESIAN_POINT('Ctrl Pts',(1.63420665729798,1.,0.970669715997509));
#30276=CARTESIAN_POINT('Ctrl Pts',(1.63013849959461,-1.,0.967387853230345));
#30277=CARTESIAN_POINT('Ctrl Pts',(1.63013849959461,1.,0.967387853230345));
#30278=CARTESIAN_POINT('Ctrl Pts',(1.62571930670187,-1.,0.964046107040536));
#30279=CARTESIAN_POINT('Ctrl Pts',(1.62571930670187,1.,0.964046107040536));
#30280=CARTESIAN_POINT('Ctrl Pts',(1.62061638140221,-1.,0.960438326101729));
#30281=CARTESIAN_POINT('Ctrl Pts',(1.62061638140221,1.,0.960438326101729));
#30282=CARTESIAN_POINT('Ctrl Pts',(1.61449324337085,-1.,0.956354422920671));
#30283=CARTESIAN_POINT('Ctrl Pts',(1.61449324337085,1.,0.956354422920671));
#30284=CARTESIAN_POINT('Ctrl Pts',(1.60706069896936,-1.,0.951613284356035));
#30285=CARTESIAN_POINT('Ctrl Pts',(1.60706069896936,1.,0.951613284356035));
#30286=CARTESIAN_POINT('Ctrl Pts',(1.59810042043673,-1.,0.946078063315257));
#30287=CARTESIAN_POINT('Ctrl Pts',(1.59810042043673,1.,0.946078063315257));
#30288=CARTESIAN_POINT('Ctrl Pts',(1.58744937487176,-1.,0.939646377893399));
#30289=CARTESIAN_POINT('Ctrl Pts',(1.58744937487176,1.,0.939646377893399));
#30290=CARTESIAN_POINT('Ctrl Pts',(1.57499388382243,-1.,0.932246680108685));
#30291=CARTESIAN_POINT('Ctrl Pts',(1.57499388382243,1.,0.932246680108685));
#30292=CARTESIAN_POINT('Ctrl Pts',(1.56065988578893,-1.,0.923832188944341));
#30293=CARTESIAN_POINT('Ctrl Pts',(1.56065988578893,1.,0.923832188944341));
#30294=CARTESIAN_POINT('Ctrl Pts',(1.54440491149498,-1.,0.914375919026456));
#30295=CARTESIAN_POINT('Ctrl Pts',(1.54440491149498,1.,0.914375919026456));
#30296=CARTESIAN_POINT('Ctrl Pts',(1.52984849887993,-1.,0.905967409625651));
#30297=CARTESIAN_POINT('Ctrl Pts',(1.52984849887993,1.,0.905967409625651));
#30298=CARTESIAN_POINT('Ctrl Pts',(1.51805569590094,-1.,0.899185047483511));
#30299=CARTESIAN_POINT('Ctrl Pts',(1.51805569590094,1.,0.899185047483511));
#30300=CARTESIAN_POINT('Ctrl Pts',(1.50980486806688,-1.,0.894452006964544));
#30301=CARTESIAN_POINT('Ctrl Pts',(1.50980486806688,1.,0.894452006964544));
#30302=CARTESIAN_POINT('Ctrl Pts',(1.5055822144029,-1.,0.892032620296856));
#30303=CARTESIAN_POINT('Ctrl Pts',(1.5055822144029,1.,0.892032620296856));
#30304=CARTESIAN_POINT('',(1.81978687191668,1.,1.23627494547115));
#30305=CARTESIAN_POINT('Ctrl Pts',(1.81978687191668,1.,1.23627494547115));
#30306=CARTESIAN_POINT('Ctrl Pts',(1.81925017193666,1.,1.23509651170476));
#30307=CARTESIAN_POINT('Ctrl Pts',(1.81817389921279,1.,1.2327422452705));
#30308=CARTESIAN_POINT('Ctrl Pts',(1.8165508718364,1.,1.2292186489137));
#30309=CARTESIAN_POINT('Ctrl Pts',(1.81436959210434,1.,1.2245361330495));
#30310=CARTESIAN_POINT('Ctrl Pts',(1.81161420806656,1.,1.21870906103557));
#30311=CARTESIAN_POINT('Ctrl Pts',(1.80882996917129,1.,1.21290815708314));
#30312=CARTESIAN_POINT('Ctrl Pts',(1.80601678480707,1.,1.20713356605475));
#30313=CARTESIAN_POINT('Ctrl Pts',(1.80317454838603,1.,1.20138548938974));
#30314=CARTESIAN_POINT('Ctrl Pts',(1.80030314369879,1.,1.19566418930242));
#30315=CARTESIAN_POINT('Ctrl Pts',(1.79740245923478,1.,1.18996997934445));
#30316=CARTESIAN_POINT('Ctrl Pts',(1.79447240321515,1.,1.18430321697432));
#30317=CARTESIAN_POINT('Ctrl Pts',(1.79151291552689,1.,1.17866429440809));
#30318=CARTESIAN_POINT('Ctrl Pts',(1.78852398877616,1.,1.17305363177328));
#30319=CARTESIAN_POINT('Ctrl Pts',(1.78550566040443,1.,1.16747166312303));
#30320=CARTESIAN_POINT('Ctrl Pts',(1.78245795881009,1.,1.16191881298499));
#30321=CARTESIAN_POINT('Ctrl Pts',(1.77938085564275,1.,1.15639547194698));
#30322=CARTESIAN_POINT('Ctrl Pts',(1.7762742255701,1.,1.15090197841515));
#30323=CARTESIAN_POINT('Ctrl Pts',(1.77313777896194,1.,1.1454385822692));
#30324=CARTESIAN_POINT('Ctrl Pts',(1.76997111386769,1.,1.14000548336975));
#30325=CARTESIAN_POINT('Ctrl Pts',(1.76677384551862,1.,1.1346029180462));
#30326=CARTESIAN_POINT('Ctrl Pts',(1.7635457196617,1.,1.12923123555075));
#30327=CARTESIAN_POINT('Ctrl Pts',(1.76028671825096,1.,1.12389096855086));
#30328=CARTESIAN_POINT('Ctrl Pts',(1.75699720772105,1.,1.11858293216763));
#30329=CARTESIAN_POINT('Ctrl Pts',(1.7536777209463,1.,1.11330807582551));
#30330=CARTESIAN_POINT('Ctrl Pts',(1.7503286607592,1.,1.10806728183007));
#30331=CARTESIAN_POINT('Ctrl Pts',(1.74695004214923,1.,1.10286118991143));
#30332=CARTESIAN_POINT('Ctrl Pts',(1.74354119236208,1.,1.09768999241226));
#30333=CARTESIAN_POINT('Ctrl Pts',(1.74010053962247,1.,1.09255329056493));
#30334=CARTESIAN_POINT('Ctrl Pts',(1.73662628326091,1.,1.08745056285427));
#30335=CARTESIAN_POINT('Ctrl Pts',(1.73311705663407,1.,1.08238162784749));
#30336=CARTESIAN_POINT('Ctrl Pts',(1.72957248977424,1.,1.0773470373727));
#30337=CARTESIAN_POINT('Ctrl Pts',(1.72599406198488,1.,1.07234866990252));
#30338=CARTESIAN_POINT('Ctrl Pts',(1.72238500928453,1.,1.06738966975462));
#30339=CARTESIAN_POINT('Ctrl Pts',(1.71874858456904,1.,1.06247324680647));
#30340=CARTESIAN_POINT('Ctrl Pts',(1.7150865442702,1.,1.05760163192479));
#30341=CARTESIAN_POINT('Ctrl Pts',(1.71139783543989,1.,1.05277517202855));
#30342=CARTESIAN_POINT('Ctrl Pts',(1.70767646263649,1.,1.04799085404995));
#30343=CARTESIAN_POINT('Ctrl Pts',(1.70391338707982,1.,1.04324363334554));
#30344=CARTESIAN_POINT('Ctrl Pts',(1.70010052930962,1.,1.03852922490789));
#30345=CARTESIAN_POINT('Ctrl Pts',(1.69623414782771,1.,1.03384646003588));
#30346=CARTESIAN_POINT('Ctrl Pts',(1.69231840863458,1.,1.02919977579147));
#30347=CARTESIAN_POINT('Ctrl Pts',(1.68836910178447,1.,1.02460180535255));
#30348=CARTESIAN_POINT('Ctrl Pts',(1.68440578021706,1.,1.02006795074201));
#30349=CARTESIAN_POINT('Ctrl Pts',(1.68044289894798,1.,1.01561026162773));
#30350=CARTESIAN_POINT('Ctrl Pts',(1.67648246776464,1.,1.01123236493511));
#30351=CARTESIAN_POINT('Ctrl Pts',(1.67250335383293,1.,1.00692206696414));
#30352=CARTESIAN_POINT('Ctrl Pts',(1.66846059277303,1.,1.00265091003727));
#30353=CARTESIAN_POINT('Ctrl Pts',(1.66430758030376,1.,0.998389654952758));
#30354=CARTESIAN_POINT('Ctrl Pts',(1.66001553809947,1.,0.994121836661306));
#30355=CARTESIAN_POINT('Ctrl Pts',(1.65559044289699,1.,0.989855627854165));
#30356=CARTESIAN_POINT('Ctrl Pts',(1.65110016612638,1.,0.985642622920821));
#30357=CARTESIAN_POINT('Ctrl Pts',(1.64665139190656,1.,0.981562530939489));
#30358=CARTESIAN_POINT('Ctrl Pts',(1.64233990826687,1.,0.977689794119417));
#30359=CARTESIAN_POINT('Ctrl Pts',(1.63820952658144,1.,0.974066058287419));
#30360=CARTESIAN_POINT('Ctrl Pts',(1.63420665729798,1.,0.970669715997509));
#30361=CARTESIAN_POINT('Ctrl Pts',(1.63013849959461,1.,0.967387853230345));
#30362=CARTESIAN_POINT('Ctrl Pts',(1.62571930670187,1.,0.964046107040536));
#30363=CARTESIAN_POINT('Ctrl Pts',(1.62061638140221,1.,0.960438326101729));
#30364=CARTESIAN_POINT('Ctrl Pts',(1.61449324337085,1.,0.956354422920671));
#30365=CARTESIAN_POINT('Ctrl Pts',(1.60706069896936,1.,0.951613284356035));
#30366=CARTESIAN_POINT('Ctrl Pts',(1.59810042043673,1.,0.946078063315257));
#30367=CARTESIAN_POINT('Ctrl Pts',(1.58744937487176,1.,0.939646377893399));
#30368=CARTESIAN_POINT('Ctrl Pts',(1.57499388382243,1.,0.932246680108685));
#30369=CARTESIAN_POINT('Ctrl Pts',(1.56065988578893,1.,0.923832188944341));
#30370=CARTESIAN_POINT('Ctrl Pts',(1.54440491149498,1.,0.914375919026456));
#30371=CARTESIAN_POINT('Ctrl Pts',(1.52984849887993,1.,0.905967409625651));
#30372=CARTESIAN_POINT('Ctrl Pts',(1.51805569590094,1.,0.899185047483511));
#30373=CARTESIAN_POINT('Ctrl Pts',(1.50980486806688,1.,0.894452006964544));
#30374=CARTESIAN_POINT('Ctrl Pts',(1.5055822144029,1.,0.892032620296856));
#30375=CARTESIAN_POINT('',(1.81978687191668,0.,1.23627494547115));
#30376=CARTESIAN_POINT('Origin',(1.73811241238545,0.,1.34869019493419));
#30377=CARTESIAN_POINT('',(1.73811241238545,1.,1.34869019493419));
#30378=CARTESIAN_POINT('',(1.81978687191668,1.,1.23627494547115));
#30379=CARTESIAN_POINT('',(1.73811241238545,0.,1.34869019493419));
#30380=CARTESIAN_POINT('Ctrl Pts',(1.31362392696032,-1.,1.15624053661742));
#30381=CARTESIAN_POINT('Ctrl Pts',(1.31362392696032,1.,1.15624053661742));
#30382=CARTESIAN_POINT('Ctrl Pts',(1.31722977216397,-1.,1.15950888730809));
#30383=CARTESIAN_POINT('Ctrl Pts',(1.31722977216397,1.,1.15950888730809));
#30384=CARTESIAN_POINT('Ctrl Pts',(1.32428080721772,-1.,1.16589330093588));
#30385=CARTESIAN_POINT('Ctrl Pts',(1.32428080721772,1.,1.16589330093588));
#30386=CARTESIAN_POINT('Ctrl Pts',(1.33437539347008,-1.,1.17501305789857));
#30387=CARTESIAN_POINT('Ctrl Pts',(1.33437539347008,1.,1.17501305789857));
#30388=CARTESIAN_POINT('Ctrl Pts',(1.34687054001093,-1.,1.18625865667441));
#30389=CARTESIAN_POINT('Ctrl Pts',(1.34687054001093,1.,1.18625865667441));
#30390=CARTESIAN_POINT('Ctrl Pts',(1.36088705043885,-1.,1.1987959077932));
#30391=CARTESIAN_POINT('Ctrl Pts',(1.36088705043885,1.,1.1987959077932));
#30392=CARTESIAN_POINT('Ctrl Pts',(1.37331915607905,-1.,1.20982812925645));
#30393=CARTESIAN_POINT('Ctrl Pts',(1.37331915607905,1.,1.20982812925645));
#30394=CARTESIAN_POINT('Ctrl Pts',(1.38420564527715,-1.,1.21938737280852));
#30395=CARTESIAN_POINT('Ctrl Pts',(1.38420564527715,1.,1.21938737280852));
#30396=CARTESIAN_POINT('Ctrl Pts',(1.39361389568796,-1.,1.22752961899387));
#30397=CARTESIAN_POINT('Ctrl Pts',(1.39361389568796,1.,1.22752961899387));
#30398=CARTESIAN_POINT('Ctrl Pts',(1.40164708206106,-1.,1.23434087290423));
#30399=CARTESIAN_POINT('Ctrl Pts',(1.40164708206106,1.,1.23434087290423));
#30400=CARTESIAN_POINT('Ctrl Pts',(1.40845295531283,-1.,1.23994455029534));
#30401=CARTESIAN_POINT('Ctrl Pts',(1.40845295531283,1.,1.23994455029534));
#30402=CARTESIAN_POINT('Ctrl Pts',(1.41422913175179,-1.,1.24450600513056));
#30403=CARTESIAN_POINT('Ctrl Pts',(1.41422913175179,1.,1.24450600513056));
#30404=CARTESIAN_POINT('Ctrl Pts',(1.41923722596025,-1.,1.24824430986571));
#30405=CARTESIAN_POINT('Ctrl Pts',(1.41923722596025,1.,1.24824430986571));
#30406=CARTESIAN_POINT('Ctrl Pts',(1.42378102115575,-1.,1.2514145557001));
#30407=CARTESIAN_POINT('Ctrl Pts',(1.42378102115575,1.,1.2514145557001));
#30408=CARTESIAN_POINT('Ctrl Pts',(1.42815938799387,-1.,1.25426945222639));
#30409=CARTESIAN_POINT('Ctrl Pts',(1.42815938799387,1.,1.25426945222639));
#30410=CARTESIAN_POINT('Ctrl Pts',(1.43262645609691,-1.,1.25702687965755));
#30411=CARTESIAN_POINT('Ctrl Pts',(1.43262645609691,1.,1.25702687965755));
#30412=CARTESIAN_POINT('Ctrl Pts',(1.43734919180847,-1.,1.25983531012005));
#30413=CARTESIAN_POINT('Ctrl Pts',(1.43734919180847,1.,1.25983531012005));
#30414=CARTESIAN_POINT('Ctrl Pts',(1.44236470511303,-1.,1.26273903323859));
#30415=CARTESIAN_POINT('Ctrl Pts',(1.44236470511303,1.,1.26273903323859));
#30416=CARTESIAN_POINT('Ctrl Pts',(1.44761985001662,-1.,1.26570925118868));
#30417=CARTESIAN_POINT('Ctrl Pts',(1.44761985001662,1.,1.26570925118868));
#30418=CARTESIAN_POINT('Ctrl Pts',(1.45301422764247,-1.,1.2686778680489));
#30419=CARTESIAN_POINT('Ctrl Pts',(1.45301422764247,1.,1.2686778680489));
#30420=CARTESIAN_POINT('Ctrl Pts',(1.45843906294697,-1.,1.27156805265289));
#30421=CARTESIAN_POINT('Ctrl Pts',(1.45843906294697,1.,1.27156805265289));
#30422=CARTESIAN_POINT('Ctrl Pts',(1.46382431332476,-1.,1.27433119897822));
#30423=CARTESIAN_POINT('Ctrl Pts',(1.46382431332476,1.,1.27433119897822));
#30424=CARTESIAN_POINT('Ctrl Pts',(1.46916035917133,-1.,1.2769641483109));
#30425=CARTESIAN_POINT('Ctrl Pts',(1.46916035917133,1.,1.2769641483109));
#30426=CARTESIAN_POINT('Ctrl Pts',(1.4744717526707,-1.,1.2794891824849));
#30427=CARTESIAN_POINT('Ctrl Pts',(1.4744717526707,1.,1.2794891824849));
#30428=CARTESIAN_POINT('Ctrl Pts',(1.47980070347095,-1.,1.28194158939517));
#30429=CARTESIAN_POINT('Ctrl Pts',(1.47980070347095,1.,1.28194158939517));
#30430=CARTESIAN_POINT('Ctrl Pts',(1.4851881711891,-1.,1.28435533880201));
#30431=CARTESIAN_POINT('Ctrl Pts',(1.4851881711891,1.,1.28435533880201));
#30432=CARTESIAN_POINT('Ctrl Pts',(1.4906522831278,-1.,1.2867467611644));
#30433=CARTESIAN_POINT('Ctrl Pts',(1.4906522831278,1.,1.2867467611644));
#30434=CARTESIAN_POINT('Ctrl Pts',(1.49618896881754,-1.,1.28911506584254));
#30435=CARTESIAN_POINT('Ctrl Pts',(1.49618896881754,1.,1.28911506584254));
#30436=CARTESIAN_POINT('Ctrl Pts',(1.50178230149776,-1.,1.29145022885181));
#30437=CARTESIAN_POINT('Ctrl Pts',(1.50178230149776,1.,1.29145022885181));
#30438=CARTESIAN_POINT('Ctrl Pts',(1.50741159078365,-1.,1.29373841372842));
#30439=CARTESIAN_POINT('Ctrl Pts',(1.50741159078365,1.,1.29373841372842));
#30440=CARTESIAN_POINT('Ctrl Pts',(1.51305994241402,-1.,1.29596850710509));
#30441=CARTESIAN_POINT('Ctrl Pts',(1.51305994241402,1.,1.29596850710509));
#30442=CARTESIAN_POINT('Ctrl Pts',(1.51872184912724,-1.,1.29813791800747));
#30443=CARTESIAN_POINT('Ctrl Pts',(1.51872184912724,1.,1.29813791800747));
#30444=CARTESIAN_POINT('Ctrl Pts',(1.52439957861062,-1.,1.30024984366328));
#30445=CARTESIAN_POINT('Ctrl Pts',(1.52439957861062,1.,1.30024984366328));
#30446=CARTESIAN_POINT('Ctrl Pts',(1.53009970283891,-1.,1.30231064395568));
#30447=CARTESIAN_POINT('Ctrl Pts',(1.53009970283891,1.,1.30231064395568));
#30448=CARTESIAN_POINT('Ctrl Pts',(1.53582981268977,-1.,1.30432735639489));
#30449=CARTESIAN_POINT('Ctrl Pts',(1.53582981268977,1.,1.30432735639489));
#30450=CARTESIAN_POINT('Ctrl Pts',(1.54159462645432,-1.,1.30630475189556));
#30451=CARTESIAN_POINT('Ctrl Pts',(1.54159462645432,1.,1.30630475189556));
#30452=CARTESIAN_POINT('Ctrl Pts',(1.54739413957185,-1.,1.30824393907473));
#30453=CARTESIAN_POINT('Ctrl Pts',(1.54739413957185,1.,1.30824393907473));
#30454=CARTESIAN_POINT('Ctrl Pts',(1.55322568759481,-1.,1.31014393684222));
#30455=CARTESIAN_POINT('Ctrl Pts',(1.55322568759481,1.,1.31014393684222));
#30456=CARTESIAN_POINT('Ctrl Pts',(1.55908521254821,-1.,1.31200264341696));
#30457=CARTESIAN_POINT('Ctrl Pts',(1.55908521254821,1.,1.31200264341696));
#30458=CARTESIAN_POINT('Ctrl Pts',(1.56496872402353,-1.,1.31381795281002));
#30459=CARTESIAN_POINT('Ctrl Pts',(1.56496872402353,1.,1.31381795281002));
#30460=CARTESIAN_POINT('Ctrl Pts',(1.57087397835723,-1.,1.31558903860016));
#30461=CARTESIAN_POINT('Ctrl Pts',(1.57087397835723,1.,1.31558903860016));
#30462=CARTESIAN_POINT('Ctrl Pts',(1.5768005650559,-1.,1.31731642317187));
#30463=CARTESIAN_POINT('Ctrl Pts',(1.5768005650559,1.,1.31731642317187));
#30464=CARTESIAN_POINT('Ctrl Pts',(1.58274907898834,-1.,1.31900135021432));
#30465=CARTESIAN_POINT('Ctrl Pts',(1.58274907898834,1.,1.31900135021432));
#30466=CARTESIAN_POINT('Ctrl Pts',(1.58872057258245,-1.,1.32064537110892));
#30467=CARTESIAN_POINT('Ctrl Pts',(1.58872057258245,1.,1.32064537110892));
#30468=CARTESIAN_POINT('Ctrl Pts',(1.59471591079403,-1.,1.32224985747682));
#30469=CARTESIAN_POINT('Ctrl Pts',(1.59471591079403,1.,1.32224985747682));
#30470=CARTESIAN_POINT('Ctrl Pts',(1.60073511858687,-1.,1.32381550858256));
#30471=CARTESIAN_POINT('Ctrl Pts',(1.60073511858687,1.,1.32381550858256));
#30472=CARTESIAN_POINT('Ctrl Pts',(1.60677758290954,-1.,1.32534250785782));
#30473=CARTESIAN_POINT('Ctrl Pts',(1.60677758290954,1.,1.32534250785782));
#30474=CARTESIAN_POINT('Ctrl Pts',(1.6128423401575,-1.,1.32683074483356));
#30475=CARTESIAN_POINT('Ctrl Pts',(1.6128423401575,1.,1.32683074483356));
#30476=CARTESIAN_POINT('Ctrl Pts',(1.61892832270724,-1.,1.32828000610449));
#30477=CARTESIAN_POINT('Ctrl Pts',(1.61892832270724,1.,1.32828000610449));
#30478=CARTESIAN_POINT('Ctrl Pts',(1.62503464209797,-1.,1.3296901950568));
#30479=CARTESIAN_POINT('Ctrl Pts',(1.62503464209797,1.,1.3296901950568));
#30480=CARTESIAN_POINT('Ctrl Pts',(1.63116079730923,-1.,1.33106149345645));
#30481=CARTESIAN_POINT('Ctrl Pts',(1.63116079730923,1.,1.33106149345645));
#30482=CARTESIAN_POINT('Ctrl Pts',(1.63730653475089,-1.,1.33239425103724));
#30483=CARTESIAN_POINT('Ctrl Pts',(1.63730653475089,1.,1.33239425103724));
#30484=CARTESIAN_POINT('Ctrl Pts',(1.6434717485603,-1.,1.33368890676572));
#30485=CARTESIAN_POINT('Ctrl Pts',(1.6434717485603,1.,1.33368890676572));
#30486=CARTESIAN_POINT('Ctrl Pts',(1.6496563728683,-1.,1.33494590467993));
#30487=CARTESIAN_POINT('Ctrl Pts',(1.6496563728683,1.,1.33494590467993));
#30488=CARTESIAN_POINT('Ctrl Pts',(1.65586025952593,-1.,1.33616559745172));
#30489=CARTESIAN_POINT('Ctrl Pts',(1.65586025952593,1.,1.33616559745172));
#30490=CARTESIAN_POINT('Ctrl Pts',(1.66208312541983,-1.,1.33734820885262));
#30491=CARTESIAN_POINT('Ctrl Pts',(1.66208312541983,1.,1.33734820885262));
#30492=CARTESIAN_POINT('Ctrl Pts',(1.66832460783989,-1.,1.33849388654388));
#30493=CARTESIAN_POINT('Ctrl Pts',(1.66832460783989,1.,1.33849388654388));
#30494=CARTESIAN_POINT('Ctrl Pts',(1.67458429426086,-1.,1.3396027347034));
#30495=CARTESIAN_POINT('Ctrl Pts',(1.67458429426086,1.,1.3396027347034));
#30496=CARTESIAN_POINT('Ctrl Pts',(1.68086176030362,-1.,1.34067485185203));
#30497=CARTESIAN_POINT('Ctrl Pts',(1.68086176030362,1.,1.34067485185203));
#30498=CARTESIAN_POINT('Ctrl Pts',(1.68715660868764,-1.,1.341710374848));
#30499=CARTESIAN_POINT('Ctrl Pts',(1.68715660868764,1.,1.341710374848));
#30500=CARTESIAN_POINT('Ctrl Pts',(1.6934684849687,-1.,1.34270948206319));
#30501=CARTESIAN_POINT('Ctrl Pts',(1.6934684849687,1.,1.34270948206319));
#30502=CARTESIAN_POINT('Ctrl Pts',(1.69979707754427,-1.,1.34367237124483));
#30503=CARTESIAN_POINT('Ctrl Pts',(1.69979707754427,1.,1.34367237124483));
#30504=CARTESIAN_POINT('Ctrl Pts',(1.70614212266738,-1.,1.34459924533831));
#30505=CARTESIAN_POINT('Ctrl Pts',(1.70614212266738,1.,1.34459924533831));
#30506=CARTESIAN_POINT('Ctrl Pts',(1.71250340686822,-1.,1.34549029589416));
#30507=CARTESIAN_POINT('Ctrl Pts',(1.71250340686822,1.,1.34549029589416));
#30508=CARTESIAN_POINT('Ctrl Pts',(1.7188807715049,-1.,1.34634568653227));
#30509=CARTESIAN_POINT('Ctrl Pts',(1.7188807715049,1.,1.34634568653227));
#30510=CARTESIAN_POINT('Ctrl Pts',(1.72527410680674,-1.,1.34716554819527));
#30511=CARTESIAN_POINT('Ctrl Pts',(1.72527410680674,1.,1.34716554819527));
#30512=CARTESIAN_POINT('Ctrl Pts',(1.7304014965394,-1.,1.34779309152035));
#30513=CARTESIAN_POINT('Ctrl Pts',(1.7304014965394,1.,1.34779309152035));
#30514=CARTESIAN_POINT('Ctrl Pts',(1.73425417885907,-1.,1.34824783112887));
#30515=CARTESIAN_POINT('Ctrl Pts',(1.73425417885907,1.,1.34824783112887));
#30516=CARTESIAN_POINT('Ctrl Pts',(1.73682580585691,-1.,1.34854391898045));
#30517=CARTESIAN_POINT('Ctrl Pts',(1.73682580585691,1.,1.34854391898045));
#30518=CARTESIAN_POINT('Ctrl Pts',(1.73811241238545,-1.,1.34869019493419));
#30519=CARTESIAN_POINT('Ctrl Pts',(1.73811241238545,1.,1.34869019493419));
#30520=CARTESIAN_POINT('',(1.31362392696032,1.,1.15624053661742));
#30521=CARTESIAN_POINT('Ctrl Pts',(1.31362392696032,1.,1.15624053661742));
#30522=CARTESIAN_POINT('Ctrl Pts',(1.31722977216397,1.,1.15950888730809));
#30523=CARTESIAN_POINT('Ctrl Pts',(1.32428080721772,1.,1.16589330093588));
#30524=CARTESIAN_POINT('Ctrl Pts',(1.33437539347008,1.,1.17501305789857));
#30525=CARTESIAN_POINT('Ctrl Pts',(1.34687054001093,1.,1.18625865667441));
#30526=CARTESIAN_POINT('Ctrl Pts',(1.36088705043885,1.,1.1987959077932));
#30527=CARTESIAN_POINT('Ctrl Pts',(1.37331915607905,1.,1.20982812925645));
#30528=CARTESIAN_POINT('Ctrl Pts',(1.38420564527715,1.,1.21938737280852));
#30529=CARTESIAN_POINT('Ctrl Pts',(1.39361389568796,1.,1.22752961899387));
#30530=CARTESIAN_POINT('Ctrl Pts',(1.40164708206106,1.,1.23434087290423));
#30531=CARTESIAN_POINT('Ctrl Pts',(1.40845295531283,1.,1.23994455029534));
#30532=CARTESIAN_POINT('Ctrl Pts',(1.41422913175179,1.,1.24450600513056));
#30533=CARTESIAN_POINT('Ctrl Pts',(1.41923722596025,1.,1.24824430986571));
#30534=CARTESIAN_POINT('Ctrl Pts',(1.42378102115575,1.,1.2514145557001));
#30535=CARTESIAN_POINT('Ctrl Pts',(1.42815938799387,1.,1.25426945222639));
#30536=CARTESIAN_POINT('Ctrl Pts',(1.43262645609691,1.,1.25702687965755));
#30537=CARTESIAN_POINT('Ctrl Pts',(1.43734919180847,1.,1.25983531012005));
#30538=CARTESIAN_POINT('Ctrl Pts',(1.44236470511303,1.,1.26273903323859));
#30539=CARTESIAN_POINT('Ctrl Pts',(1.44761985001662,1.,1.26570925118868));
#30540=CARTESIAN_POINT('Ctrl Pts',(1.45301422764247,1.,1.2686778680489));
#30541=CARTESIAN_POINT('Ctrl Pts',(1.45843906294697,1.,1.27156805265289));
#30542=CARTESIAN_POINT('Ctrl Pts',(1.46382431332476,1.,1.27433119897822));
#30543=CARTESIAN_POINT('Ctrl Pts',(1.46916035917133,1.,1.2769641483109));
#30544=CARTESIAN_POINT('Ctrl Pts',(1.4744717526707,1.,1.2794891824849));
#30545=CARTESIAN_POINT('Ctrl Pts',(1.47980070347095,1.,1.28194158939517));
#30546=CARTESIAN_POINT('Ctrl Pts',(1.4851881711891,1.,1.28435533880201));
#30547=CARTESIAN_POINT('Ctrl Pts',(1.4906522831278,1.,1.2867467611644));
#30548=CARTESIAN_POINT('Ctrl Pts',(1.49618896881754,1.,1.28911506584254));
#30549=CARTESIAN_POINT('Ctrl Pts',(1.50178230149776,1.,1.29145022885181));
#30550=CARTESIAN_POINT('Ctrl Pts',(1.50741159078365,1.,1.29373841372842));
#30551=CARTESIAN_POINT('Ctrl Pts',(1.51305994241402,1.,1.29596850710509));
#30552=CARTESIAN_POINT('Ctrl Pts',(1.51872184912724,1.,1.29813791800747));
#30553=CARTESIAN_POINT('Ctrl Pts',(1.52439957861062,1.,1.30024984366328));
#30554=CARTESIAN_POINT('Ctrl Pts',(1.53009970283891,1.,1.30231064395568));
#30555=CARTESIAN_POINT('Ctrl Pts',(1.53582981268977,1.,1.30432735639489));
#30556=CARTESIAN_POINT('Ctrl Pts',(1.54159462645432,1.,1.30630475189556));
#30557=CARTESIAN_POINT('Ctrl Pts',(1.54739413957185,1.,1.30824393907473));
#30558=CARTESIAN_POINT('Ctrl Pts',(1.55322568759481,1.,1.31014393684222));
#30559=CARTESIAN_POINT('Ctrl Pts',(1.55908521254821,1.,1.31200264341696));
#30560=CARTESIAN_POINT('Ctrl Pts',(1.56496872402353,1.,1.31381795281002));
#30561=CARTESIAN_POINT('Ctrl Pts',(1.57087397835723,1.,1.31558903860016));
#30562=CARTESIAN_POINT('Ctrl Pts',(1.5768005650559,1.,1.31731642317187));
#30563=CARTESIAN_POINT('Ctrl Pts',(1.58274907898834,1.,1.31900135021432));
#30564=CARTESIAN_POINT('Ctrl Pts',(1.58872057258245,1.,1.32064537110892));
#30565=CARTESIAN_POINT('Ctrl Pts',(1.59471591079403,1.,1.32224985747682));
#30566=CARTESIAN_POINT('Ctrl Pts',(1.60073511858687,1.,1.32381550858256));
#30567=CARTESIAN_POINT('Ctrl Pts',(1.60677758290954,1.,1.32534250785782));
#30568=CARTESIAN_POINT('Ctrl Pts',(1.6128423401575,1.,1.32683074483356));
#30569=CARTESIAN_POINT('Ctrl Pts',(1.61892832270724,1.,1.32828000610449));
#30570=CARTESIAN_POINT('Ctrl Pts',(1.62503464209797,1.,1.3296901950568));
#30571=CARTESIAN_POINT('Ctrl Pts',(1.63116079730923,1.,1.33106149345645));
#30572=CARTESIAN_POINT('Ctrl Pts',(1.63730653475089,1.,1.33239425103724));
#30573=CARTESIAN_POINT('Ctrl Pts',(1.6434717485603,1.,1.33368890676572));
#30574=CARTESIAN_POINT('Ctrl Pts',(1.6496563728683,1.,1.33494590467993));
#30575=CARTESIAN_POINT('Ctrl Pts',(1.65586025952593,1.,1.33616559745172));
#30576=CARTESIAN_POINT('Ctrl Pts',(1.66208312541983,1.,1.33734820885262));
#30577=CARTESIAN_POINT('Ctrl Pts',(1.66832460783989,1.,1.33849388654388));
#30578=CARTESIAN_POINT('Ctrl Pts',(1.67458429426086,1.,1.3396027347034));
#30579=CARTESIAN_POINT('Ctrl Pts',(1.68086176030362,1.,1.34067485185203));
#30580=CARTESIAN_POINT('Ctrl Pts',(1.68715660868764,1.,1.341710374848));
#30581=CARTESIAN_POINT('Ctrl Pts',(1.6934684849687,1.,1.34270948206319));
#30582=CARTESIAN_POINT('Ctrl Pts',(1.69979707754427,1.,1.34367237124483));
#30583=CARTESIAN_POINT('Ctrl Pts',(1.70614212266738,1.,1.34459924533831));
#30584=CARTESIAN_POINT('Ctrl Pts',(1.71250340686822,1.,1.34549029589416));
#30585=CARTESIAN_POINT('Ctrl Pts',(1.7188807715049,1.,1.34634568653227));
#30586=CARTESIAN_POINT('Ctrl Pts',(1.72527410680674,1.,1.34716554819527));
#30587=CARTESIAN_POINT('Ctrl Pts',(1.7304014965394,1.,1.34779309152035));
#30588=CARTESIAN_POINT('Ctrl Pts',(1.73425417885907,1.,1.34824783112887));
#30589=CARTESIAN_POINT('Ctrl Pts',(1.73682580585691,1.,1.34854391898045));
#30590=CARTESIAN_POINT('Ctrl Pts',(1.73811241238545,1.,1.34869019493419));
#30591=CARTESIAN_POINT('',(1.31362392696032,0.,1.15624053661742));
#30592=CARTESIAN_POINT('Origin',(0.,0.,0.));
#30593=CARTESIAN_POINT('',(1.15624053661742,1.,1.31362392696033));
#30594=CARTESIAN_POINT('Origin',(0.,1.,0.));
#30595=CARTESIAN_POINT('',(1.15624053661742,0.,1.31362392696032));
#30596=CARTESIAN_POINT('Ctrl Pts',(1.34869019493419,-1.,1.73811241238545));
#30597=CARTESIAN_POINT('Ctrl Pts',(1.34869019493419,1.,1.73811241238545));
#30598=CARTESIAN_POINT('Ctrl Pts',(1.34854391898145,-1.,1.73682580585819));
#30599=CARTESIAN_POINT('Ctrl Pts',(1.34854391898145,1.,1.73682580585819));
#30600=CARTESIAN_POINT('Ctrl Pts',(1.34824783113158,-1.,1.73425417886255));
#30601=CARTESIAN_POINT('Ctrl Pts',(1.34824783113158,1.,1.73425417886255));
#30602=CARTESIAN_POINT('Ctrl Pts',(1.3477930915247,-1.,1.73040149654497));
#30603=CARTESIAN_POINT('Ctrl Pts',(1.3477930915247,1.,1.73040149654497));
#30604=CARTESIAN_POINT('Ctrl Pts',(1.34716554820013,-1.,1.72527410681298));
#30605=CARTESIAN_POINT('Ctrl Pts',(1.34716554820013,1.,1.72527410681298));
#30606=CARTESIAN_POINT('Ctrl Pts',(1.34634568653586,-1.,1.7188807715095));
#30607=CARTESIAN_POINT('Ctrl Pts',(1.34634568653586,1.,1.7188807715095));
#30608=CARTESIAN_POINT('Ctrl Pts',(1.34549029589563,-1.,1.71250340687011));
#30609=CARTESIAN_POINT('Ctrl Pts',(1.34549029589563,1.,1.71250340687011));
#30610=CARTESIAN_POINT('Ctrl Pts',(1.34459924533783,-1.,1.70614212266676));
#30611=CARTESIAN_POINT('Ctrl Pts',(1.34459924533783,1.,1.70614212266676));
#30612=CARTESIAN_POINT('Ctrl Pts',(1.34367237124322,-1.,1.69979707754221));
#30613=CARTESIAN_POINT('Ctrl Pts',(1.34367237124322,1.,1.69979707754221));
#30614=CARTESIAN_POINT('Ctrl Pts',(1.34270948206139,-1.,1.6934684849664));
#30615=CARTESIAN_POINT('Ctrl Pts',(1.34270948206139,1.,1.6934684849664));
#30616=CARTESIAN_POINT('Ctrl Pts',(1.34171037484673,-1.,1.68715660868602));
#30617=CARTESIAN_POINT('Ctrl Pts',(1.34171037484673,1.,1.68715660868602));
#30618=CARTESIAN_POINT('Ctrl Pts',(1.3406748518516,-1.,1.68086176030308));
#30619=CARTESIAN_POINT('Ctrl Pts',(1.3406748518516,1.,1.68086176030308));
#30620=CARTESIAN_POINT('Ctrl Pts',(1.33960273470372,-1.,1.67458429426126));
#30621=CARTESIAN_POINT('Ctrl Pts',(1.33960273470372,1.,1.67458429426126));
#30622=CARTESIAN_POINT('Ctrl Pts',(1.33849388654458,-1.,1.66832460784078));
#30623=CARTESIAN_POINT('Ctrl Pts',(1.33849388654458,1.,1.66832460784078));
#30624=CARTESIAN_POINT('Ctrl Pts',(1.33734820885331,-1.,1.66208312542073));
#30625=CARTESIAN_POINT('Ctrl Pts',(1.33734820885331,1.,1.66208312542073));
#30626=CARTESIAN_POINT('Ctrl Pts',(1.33616559745217,-1.,1.65586025952651));
#30627=CARTESIAN_POINT('Ctrl Pts',(1.33616559745217,1.,1.65586025952651));
#30628=CARTESIAN_POINT('Ctrl Pts',(1.33494590468003,-1.,1.64965637286843));
#30629=CARTESIAN_POINT('Ctrl Pts',(1.33494590468003,1.,1.64965637286843));
#30630=CARTESIAN_POINT('Ctrl Pts',(1.33368890676554,-1.,1.64347174856007));
#30631=CARTESIAN_POINT('Ctrl Pts',(1.33368890676554,1.,1.64347174856007));
#30632=CARTESIAN_POINT('Ctrl Pts',(1.33239425103694,-1.,1.6373065347505));
#30633=CARTESIAN_POINT('Ctrl Pts',(1.33239425103694,1.,1.6373065347505));
#30634=CARTESIAN_POINT('Ctrl Pts',(1.33106149345618,-1.,1.63116079730887));
#30635=CARTESIAN_POINT('Ctrl Pts',(1.33106149345618,1.,1.63116079730887));
#30636=CARTESIAN_POINT('Ctrl Pts',(1.32969019505665,-1.,1.62503464209777));
#30637=CARTESIAN_POINT('Ctrl Pts',(1.32969019505665,1.,1.62503464209777));
#30638=CARTESIAN_POINT('Ctrl Pts',(1.32828000610448,-1.,1.61892832270723));
#30639=CARTESIAN_POINT('Ctrl Pts',(1.32828000610448,1.,1.61892832270723));
#30640=CARTESIAN_POINT('Ctrl Pts',(1.32683074483365,-1.,1.61284234015762));
#30641=CARTESIAN_POINT('Ctrl Pts',(1.32683074483365,1.,1.61284234015762));
#30642=CARTESIAN_POINT('Ctrl Pts',(1.32534250785794,-1.,1.6067775829097));
#30643=CARTESIAN_POINT('Ctrl Pts',(1.32534250785794,1.,1.6067775829097));
#30644=CARTESIAN_POINT('Ctrl Pts',(1.32381550858266,-1.,1.600735118587));
#30645=CARTESIAN_POINT('Ctrl Pts',(1.32381550858266,1.,1.600735118587));
#30646=CARTESIAN_POINT('Ctrl Pts',(1.32224985747686,-1.,1.59471591079408));
#30647=CARTESIAN_POINT('Ctrl Pts',(1.32224985747686,1.,1.59471591079408));
#30648=CARTESIAN_POINT('Ctrl Pts',(1.32064537110891,-1.,1.58872057258244));
#30649=CARTESIAN_POINT('Ctrl Pts',(1.32064537110891,1.,1.58872057258244));
#30650=CARTESIAN_POINT('Ctrl Pts',(1.31900135021428,-1.,1.58274907898829));
#30651=CARTESIAN_POINT('Ctrl Pts',(1.31900135021428,1.,1.58274907898829));
#30652=CARTESIAN_POINT('Ctrl Pts',(1.31731642317183,-1.,1.57680056505585));
#30653=CARTESIAN_POINT('Ctrl Pts',(1.31731642317183,1.,1.57680056505585));
#30654=CARTESIAN_POINT('Ctrl Pts',(1.31558903860015,-1.,1.57087397835721));
#30655=CARTESIAN_POINT('Ctrl Pts',(1.31558903860015,1.,1.57087397835721));
#30656=CARTESIAN_POINT('Ctrl Pts',(1.31381795281002,-1.,1.56496872402352));
#30657=CARTESIAN_POINT('Ctrl Pts',(1.31381795281002,1.,1.56496872402352));
#30658=CARTESIAN_POINT('Ctrl Pts',(1.31200264341696,-1.,1.55908521254822));
#30659=CARTESIAN_POINT('Ctrl Pts',(1.31200264341696,1.,1.55908521254822));
#30660=CARTESIAN_POINT('Ctrl Pts',(1.31014393684221,-1.,1.55322568759481));
#30661=CARTESIAN_POINT('Ctrl Pts',(1.31014393684221,1.,1.55322568759481));
#30662=CARTESIAN_POINT('Ctrl Pts',(1.30824393907471,-1.,1.54739413957183));
#30663=CARTESIAN_POINT('Ctrl Pts',(1.30824393907471,1.,1.54739413957183));
#30664=CARTESIAN_POINT('Ctrl Pts',(1.30630475189553,-1.,1.54159462645428));
#30665=CARTESIAN_POINT('Ctrl Pts',(1.30630475189553,1.,1.54159462645428));
#30666=CARTESIAN_POINT('Ctrl Pts',(1.30432735639487,-1.,1.53582981268976));
#30667=CARTESIAN_POINT('Ctrl Pts',(1.30432735639487,1.,1.53582981268976));
#30668=CARTESIAN_POINT('Ctrl Pts',(1.3023106439557,-1.,1.53009970283893));
#30669=CARTESIAN_POINT('Ctrl Pts',(1.3023106439557,1.,1.53009970283893));
#30670=CARTESIAN_POINT('Ctrl Pts',(1.30024984366334,-1.,1.5243995786107));
#30671=CARTESIAN_POINT('Ctrl Pts',(1.30024984366334,1.,1.5243995786107));
#30672=CARTESIAN_POINT('Ctrl Pts',(1.29813791800757,-1.,1.51872184912735));
#30673=CARTESIAN_POINT('Ctrl Pts',(1.29813791800757,1.,1.51872184912735));
#30674=CARTESIAN_POINT('Ctrl Pts',(1.29596850710518,-1.,1.51305994241412));
#30675=CARTESIAN_POINT('Ctrl Pts',(1.29596850710518,1.,1.51305994241412));
#30676=CARTESIAN_POINT('Ctrl Pts',(1.29373841372843,-1.,1.50741159078367));
#30677=CARTESIAN_POINT('Ctrl Pts',(1.29373841372843,1.,1.50741159078367));
#30678=CARTESIAN_POINT('Ctrl Pts',(1.29145022885171,-1.,1.50178230149764));
#30679=CARTESIAN_POINT('Ctrl Pts',(1.29145022885171,1.,1.50178230149764));
#30680=CARTESIAN_POINT('Ctrl Pts',(1.28911506584232,-1.,1.49618896881729));
#30681=CARTESIAN_POINT('Ctrl Pts',(1.28911506584232,1.,1.49618896881729));
#30682=CARTESIAN_POINT('Ctrl Pts',(1.28674676116415,-1.,1.4906522831275));
#30683=CARTESIAN_POINT('Ctrl Pts',(1.28674676116415,1.,1.4906522831275));
#30684=CARTESIAN_POINT('Ctrl Pts',(1.28435533880184,-1.,1.48518817118891));
#30685=CARTESIAN_POINT('Ctrl Pts',(1.28435533880184,1.,1.48518817118891));
#30686=CARTESIAN_POINT('Ctrl Pts',(1.28194158939522,-1.,1.47980070347102));
#30687=CARTESIAN_POINT('Ctrl Pts',(1.28194158939522,1.,1.47980070347102));
#30688=CARTESIAN_POINT('Ctrl Pts',(1.27948918248524,-1.,1.4744717526711));
#30689=CARTESIAN_POINT('Ctrl Pts',(1.27948918248524,1.,1.4744717526711));
#30690=CARTESIAN_POINT('Ctrl Pts',(1.27696414831144,-1.,1.46916035917197));
#30691=CARTESIAN_POINT('Ctrl Pts',(1.27696414831144,1.,1.46916035917197));
#30692=CARTESIAN_POINT('Ctrl Pts',(1.27433119897877,-1.,1.4638243133254));
#30693=CARTESIAN_POINT('Ctrl Pts',(1.27433119897877,1.,1.4638243133254));
#30694=CARTESIAN_POINT('Ctrl Pts',(1.27156805265312,-1.,1.45843906294725));
#30695=CARTESIAN_POINT('Ctrl Pts',(1.27156805265312,1.,1.45843906294725));
#30696=CARTESIAN_POINT('Ctrl Pts',(1.26867786804854,-1.,1.45301422764205));
#30697=CARTESIAN_POINT('Ctrl Pts',(1.26867786804854,1.,1.45301422764205));
#30698=CARTESIAN_POINT('Ctrl Pts',(1.26570925118767,-1.,1.44761985001544));
#30699=CARTESIAN_POINT('Ctrl Pts',(1.26570925118767,1.,1.44761985001544));
#30700=CARTESIAN_POINT('Ctrl Pts',(1.26273903323723,-1.,1.44236470511145));
#30701=CARTESIAN_POINT('Ctrl Pts',(1.26273903323723,1.,1.44236470511145));
#30702=CARTESIAN_POINT('Ctrl Pts',(1.25983531011894,-1.,1.43734919180719));
#30703=CARTESIAN_POINT('Ctrl Pts',(1.25983531011894,1.,1.43734919180719));
#30704=CARTESIAN_POINT('Ctrl Pts',(1.25702687965744,-1.,1.43262645609679));
#30705=CARTESIAN_POINT('Ctrl Pts',(1.25702687965744,1.,1.43262645609679));
#30706=CARTESIAN_POINT('Ctrl Pts',(1.25426945222783,-1.,1.42815938799555));
#30707=CARTESIAN_POINT('Ctrl Pts',(1.25426945222783,1.,1.42815938799555));
#30708=CARTESIAN_POINT('Ctrl Pts',(1.25141455570299,-1.,1.42378102115911));
#30709=CARTESIAN_POINT('Ctrl Pts',(1.25141455570299,1.,1.42378102115911));
#30710=CARTESIAN_POINT('Ctrl Pts',(1.24824430986911,-1.,1.41923722596421));
#30711=CARTESIAN_POINT('Ctrl Pts',(1.24824430986911,1.,1.41923722596421));
#30712=CARTESIAN_POINT('Ctrl Pts',(1.24450600513278,-1.,1.41422913175437));
#30713=CARTESIAN_POINT('Ctrl Pts',(1.24450600513278,1.,1.41422913175437));
#30714=CARTESIAN_POINT('Ctrl Pts',(1.23994455029421,-1.,1.40845295531151));
#30715=CARTESIAN_POINT('Ctrl Pts',(1.23994455029421,1.,1.40845295531151));
#30716=CARTESIAN_POINT('Ctrl Pts',(1.23434087289768,-1.,1.40164708205345));
#30717=CARTESIAN_POINT('Ctrl Pts',(1.23434087289768,1.,1.40164708205345));
#30718=CARTESIAN_POINT('Ctrl Pts',(1.22752961898063,-1.,1.39361389567257));
#30719=CARTESIAN_POINT('Ctrl Pts',(1.22752961898063,1.,1.39361389567257));
#30720=CARTESIAN_POINT('Ctrl Pts',(1.21938737278853,-1.,1.38420564525391));
#30721=CARTESIAN_POINT('Ctrl Pts',(1.21938737278853,1.,1.38420564525391));
#30722=CARTESIAN_POINT('Ctrl Pts',(1.20982812923113,-1.,1.37331915604962));
#30723=CARTESIAN_POINT('Ctrl Pts',(1.20982812923113,1.,1.37331915604962));
#30724=CARTESIAN_POINT('Ctrl Pts',(1.1987959077656,-1.,1.36088705040677));
#30725=CARTESIAN_POINT('Ctrl Pts',(1.1987959077656,1.,1.36088705040677));
#30726=CARTESIAN_POINT('Ctrl Pts',(1.18625865664915,-1.,1.34687053998157));
#30727=CARTESIAN_POINT('Ctrl Pts',(1.18625865664915,1.,1.34687053998157));
#30728=CARTESIAN_POINT('Ctrl Pts',(1.17501305787994,-1.,1.33437539344842));
#30729=CARTESIAN_POINT('Ctrl Pts',(1.17501305787994,1.,1.33437539344842));
#30730=CARTESIAN_POINT('Ctrl Pts',(1.16589330092532,-1.,1.32428080720544));
#30731=CARTESIAN_POINT('Ctrl Pts',(1.16589330092532,1.,1.32428080720544));
#30732=CARTESIAN_POINT('Ctrl Pts',(1.15950888730433,-1.,1.3172297721596));
#30733=CARTESIAN_POINT('Ctrl Pts',(1.15950888730433,1.,1.3172297721596));
#30734=CARTESIAN_POINT('Ctrl Pts',(1.15624053661742,-1.,1.31362392696033));
#30735=CARTESIAN_POINT('Ctrl Pts',(1.15624053661742,1.,1.31362392696033));
#30736=CARTESIAN_POINT('',(1.34869019493419,1.,1.73811241238545));
#30737=CARTESIAN_POINT('Ctrl Pts',(1.34869019493419,1.,1.73811241238545));
#30738=CARTESIAN_POINT('Ctrl Pts',(1.34854391898145,1.,1.73682580585819));
#30739=CARTESIAN_POINT('Ctrl Pts',(1.34824783113158,1.,1.73425417886255));
#30740=CARTESIAN_POINT('Ctrl Pts',(1.3477930915247,1.,1.73040149654497));
#30741=CARTESIAN_POINT('Ctrl Pts',(1.34716554820013,1.,1.72527410681298));
#30742=CARTESIAN_POINT('Ctrl Pts',(1.34634568653586,1.,1.7188807715095));
#30743=CARTESIAN_POINT('Ctrl Pts',(1.34549029589563,1.,1.71250340687011));
#30744=CARTESIAN_POINT('Ctrl Pts',(1.34459924533783,1.,1.70614212266676));
#30745=CARTESIAN_POINT('Ctrl Pts',(1.34367237124322,1.,1.69979707754221));
#30746=CARTESIAN_POINT('Ctrl Pts',(1.34270948206139,1.,1.6934684849664));
#30747=CARTESIAN_POINT('Ctrl Pts',(1.34171037484673,1.,1.68715660868602));
#30748=CARTESIAN_POINT('Ctrl Pts',(1.3406748518516,1.,1.68086176030308));
#30749=CARTESIAN_POINT('Ctrl Pts',(1.33960273470372,1.,1.67458429426126));
#30750=CARTESIAN_POINT('Ctrl Pts',(1.33849388654458,1.,1.66832460784078));
#30751=CARTESIAN_POINT('Ctrl Pts',(1.33734820885331,1.,1.66208312542073));
#30752=CARTESIAN_POINT('Ctrl Pts',(1.33616559745217,1.,1.65586025952651));
#30753=CARTESIAN_POINT('Ctrl Pts',(1.33494590468003,1.,1.64965637286843));
#30754=CARTESIAN_POINT('Ctrl Pts',(1.33368890676554,1.,1.64347174856007));
#30755=CARTESIAN_POINT('Ctrl Pts',(1.33239425103694,1.,1.6373065347505));
#30756=CARTESIAN_POINT('Ctrl Pts',(1.33106149345618,1.,1.63116079730887));
#30757=CARTESIAN_POINT('Ctrl Pts',(1.32969019505665,1.,1.62503464209777));
#30758=CARTESIAN_POINT('Ctrl Pts',(1.32828000610448,1.,1.61892832270723));
#30759=CARTESIAN_POINT('Ctrl Pts',(1.32683074483365,1.,1.61284234015762));
#30760=CARTESIAN_POINT('Ctrl Pts',(1.32534250785794,1.,1.6067775829097));
#30761=CARTESIAN_POINT('Ctrl Pts',(1.32381550858266,1.,1.600735118587));
#30762=CARTESIAN_POINT('Ctrl Pts',(1.32224985747686,1.,1.59471591079408));
#30763=CARTESIAN_POINT('Ctrl Pts',(1.32064537110891,1.,1.58872057258244));
#30764=CARTESIAN_POINT('Ctrl Pts',(1.31900135021428,1.,1.58274907898829));
#30765=CARTESIAN_POINT('Ctrl Pts',(1.31731642317183,1.,1.57680056505585));
#30766=CARTESIAN_POINT('Ctrl Pts',(1.31558903860015,1.,1.57087397835721));
#30767=CARTESIAN_POINT('Ctrl Pts',(1.31381795281002,1.,1.56496872402352));
#30768=CARTESIAN_POINT('Ctrl Pts',(1.31200264341696,1.,1.55908521254822));
#30769=CARTESIAN_POINT('Ctrl Pts',(1.31014393684221,1.,1.55322568759481));
#30770=CARTESIAN_POINT('Ctrl Pts',(1.30824393907471,1.,1.54739413957183));
#30771=CARTESIAN_POINT('Ctrl Pts',(1.30630475189553,1.,1.54159462645428));
#30772=CARTESIAN_POINT('Ctrl Pts',(1.30432735639487,1.,1.53582981268976));
#30773=CARTESIAN_POINT('Ctrl Pts',(1.3023106439557,1.,1.53009970283893));
#30774=CARTESIAN_POINT('Ctrl Pts',(1.30024984366334,1.,1.5243995786107));
#30775=CARTESIAN_POINT('Ctrl Pts',(1.29813791800757,1.,1.51872184912735));
#30776=CARTESIAN_POINT('Ctrl Pts',(1.29596850710518,1.,1.51305994241412));
#30777=CARTESIAN_POINT('Ctrl Pts',(1.29373841372843,1.,1.50741159078367));
#30778=CARTESIAN_POINT('Ctrl Pts',(1.29145022885171,1.,1.50178230149764));
#30779=CARTESIAN_POINT('Ctrl Pts',(1.28911506584232,1.,1.49618896881729));
#30780=CARTESIAN_POINT('Ctrl Pts',(1.28674676116415,1.,1.4906522831275));
#30781=CARTESIAN_POINT('Ctrl Pts',(1.28435533880184,1.,1.48518817118891));
#30782=CARTESIAN_POINT('Ctrl Pts',(1.28194158939522,1.,1.47980070347102));
#30783=CARTESIAN_POINT('Ctrl Pts',(1.27948918248524,1.,1.4744717526711));
#30784=CARTESIAN_POINT('Ctrl Pts',(1.27696414831144,1.,1.46916035917197));
#30785=CARTESIAN_POINT('Ctrl Pts',(1.27433119897877,1.,1.4638243133254));
#30786=CARTESIAN_POINT('Ctrl Pts',(1.27156805265312,1.,1.45843906294725));
#30787=CARTESIAN_POINT('Ctrl Pts',(1.26867786804854,1.,1.45301422764205));
#30788=CARTESIAN_POINT('Ctrl Pts',(1.26570925118767,1.,1.44761985001544));
#30789=CARTESIAN_POINT('Ctrl Pts',(1.26273903323723,1.,1.44236470511145));
#30790=CARTESIAN_POINT('Ctrl Pts',(1.25983531011894,1.,1.43734919180719));
#30791=CARTESIAN_POINT('Ctrl Pts',(1.25702687965744,1.,1.43262645609679));
#30792=CARTESIAN_POINT('Ctrl Pts',(1.25426945222783,1.,1.42815938799555));
#30793=CARTESIAN_POINT('Ctrl Pts',(1.25141455570299,1.,1.42378102115911));
#30794=CARTESIAN_POINT('Ctrl Pts',(1.24824430986911,1.,1.41923722596421));
#30795=CARTESIAN_POINT('Ctrl Pts',(1.24450600513278,1.,1.41422913175437));
#30796=CARTESIAN_POINT('Ctrl Pts',(1.23994455029421,1.,1.40845295531151));
#30797=CARTESIAN_POINT('Ctrl Pts',(1.23434087289768,1.,1.40164708205345));
#30798=CARTESIAN_POINT('Ctrl Pts',(1.22752961898063,1.,1.39361389567257));
#30799=CARTESIAN_POINT('Ctrl Pts',(1.21938737278853,1.,1.38420564525391));
#30800=CARTESIAN_POINT('Ctrl Pts',(1.20982812923113,1.,1.37331915604962));
#30801=CARTESIAN_POINT('Ctrl Pts',(1.1987959077656,1.,1.36088705040677));
#30802=CARTESIAN_POINT('Ctrl Pts',(1.18625865664915,1.,1.34687053998157));
#30803=CARTESIAN_POINT('Ctrl Pts',(1.17501305787994,1.,1.33437539344842));
#30804=CARTESIAN_POINT('Ctrl Pts',(1.16589330092532,1.,1.32428080720544));
#30805=CARTESIAN_POINT('Ctrl Pts',(1.15950888730433,1.,1.3172297721596));
#30806=CARTESIAN_POINT('Ctrl Pts',(1.15624053661742,1.,1.31362392696033));
#30807=CARTESIAN_POINT('',(1.34869019493419,0.,1.73811241238545));
#30808=CARTESIAN_POINT('Origin',(1.23627494547115,0.,1.81978687191668));
#30809=CARTESIAN_POINT('',(1.23627494547115,1.,1.81978687191668));
#30810=CARTESIAN_POINT('',(1.34869019493419,1.,1.73811241238545));
#30811=CARTESIAN_POINT('',(1.23627494547115,0.,1.81978687191668));
#30812=CARTESIAN_POINT('Ctrl Pts',(0.892032620296855,-1.,1.5055822144029));
#30813=CARTESIAN_POINT('Ctrl Pts',(0.892032620296855,1.,1.5055822144029));
#30814=CARTESIAN_POINT('Ctrl Pts',(0.894452006967538,-1.,1.50980486807181));
#30815=CARTESIAN_POINT('Ctrl Pts',(0.894452006967538,1.,1.50980486807181));
#30816=CARTESIAN_POINT('Ctrl Pts',(0.89918504749193,-1.,1.51805569591479));
#30817=CARTESIAN_POINT('Ctrl Pts',(0.89918504749193,1.,1.51805569591479));
#30818=CARTESIAN_POINT('Ctrl Pts',(0.905967409640498,-1.,1.52984849890434));
#30819=CARTESIAN_POINT('Ctrl Pts',(0.905967409640498,1.,1.52984849890434));
#30820=CARTESIAN_POINT('Ctrl Pts',(0.914375919046579,-1.,1.54440491152808));
#30821=CARTESIAN_POINT('Ctrl Pts',(0.914375919046579,1.,1.54440491152808));
#30822=CARTESIAN_POINT('Ctrl Pts',(0.923832188966322,-1.,1.56065988582509));
#30823=CARTESIAN_POINT('Ctrl Pts',(0.923832188966322,1.,1.56065988582509));
#30824=CARTESIAN_POINT('Ctrl Pts',(0.932246680128848,-1.,1.57499388385561));
#30825=CARTESIAN_POINT('Ctrl Pts',(0.932246680128848,1.,1.57499388385561));
#30826=CARTESIAN_POINT('Ctrl Pts',(0.939646377909319,-1.,1.58744937489796));
#30827=CARTESIAN_POINT('Ctrl Pts',(0.939646377909319,1.,1.58744937489796));
#30828=CARTESIAN_POINT('Ctrl Pts',(0.946078063325795,-1.,1.59810042045408));
#30829=CARTESIAN_POINT('Ctrl Pts',(0.946078063325795,1.,1.59810042045408));
#30830=CARTESIAN_POINT('Ctrl Pts',(0.951613284361247,-1.,1.60706069897794));
#30831=CARTESIAN_POINT('Ctrl Pts',(0.951613284361247,1.,1.60706069897794));
#30832=CARTESIAN_POINT('Ctrl Pts',(0.956354422921572,-1.,1.61449324337233));
#30833=CARTESIAN_POINT('Ctrl Pts',(0.956354422921572,1.,1.61449324337233));
#30834=CARTESIAN_POINT('Ctrl Pts',(0.960438326099958,-1.,1.62061638139929));
#30835=CARTESIAN_POINT('Ctrl Pts',(0.960438326099958,1.,1.62061638139929));
#30836=CARTESIAN_POINT('Ctrl Pts',(0.964046107037821,-1.,1.6257193066974));
#30837=CARTESIAN_POINT('Ctrl Pts',(0.964046107037821,1.,1.6257193066974));
#30838=CARTESIAN_POINT('Ctrl Pts',(0.967387853228041,-1.,1.63013849959083));
#30839=CARTESIAN_POINT('Ctrl Pts',(0.967387853228041,1.,1.63013849959083));
#30840=CARTESIAN_POINT('Ctrl Pts',(0.970669715996356,-1.,1.63420665729609));
#30841=CARTESIAN_POINT('Ctrl Pts',(0.970669715996356,1.,1.63420665729609));
#30842=CARTESIAN_POINT('Ctrl Pts',(0.974066058287501,-1.,1.63820952658157));
#30843=CARTESIAN_POINT('Ctrl Pts',(0.974066058287501,1.,1.63820952658157));
#30844=CARTESIAN_POINT('Ctrl Pts',(0.977689794120296,-1.,1.64233990826831));
#30845=CARTESIAN_POINT('Ctrl Pts',(0.977689794120296,1.,1.64233990826831));
#30846=CARTESIAN_POINT('Ctrl Pts',(0.981562530940574,-1.,1.64665139190834));
#30847=CARTESIAN_POINT('Ctrl Pts',(0.981562530940574,1.,1.64665139190834));
#30848=CARTESIAN_POINT('Ctrl Pts',(0.985642622921626,-1.,1.6511001661277));
#30849=CARTESIAN_POINT('Ctrl Pts',(0.985642622921626,1.,1.6511001661277));
#30850=CARTESIAN_POINT('Ctrl Pts',(0.98985562785445,-1.,1.65559044289746));
#30851=CARTESIAN_POINT('Ctrl Pts',(0.98985562785445,1.,1.65559044289746));
#30852=CARTESIAN_POINT('Ctrl Pts',(0.994121836661115,-1.,1.66001553809916));
#30853=CARTESIAN_POINT('Ctrl Pts',(0.994121836661115,1.,1.66001553809916));
#30854=CARTESIAN_POINT('Ctrl Pts',(0.998389654952317,-1.,1.66430758030304));
#30855=CARTESIAN_POINT('Ctrl Pts',(0.998389654952317,1.,1.66430758030304));
#30856=CARTESIAN_POINT('Ctrl Pts',(1.00265091003682,-1.,1.66846059277231));
#30857=CARTESIAN_POINT('Ctrl Pts',(1.00265091003682,1.,1.66846059277231));
#30858=CARTESIAN_POINT('Ctrl Pts',(1.00692206696387,-1.,1.67250335383248));
#30859=CARTESIAN_POINT('Ctrl Pts',(1.00692206696387,1.,1.67250335383248));
#30860=CARTESIAN_POINT('Ctrl Pts',(1.01123236493507,-1.,1.67648246776457));
#30861=CARTESIAN_POINT('Ctrl Pts',(1.01123236493507,1.,1.67648246776457));
#30862=CARTESIAN_POINT('Ctrl Pts',(1.01561026162786,-1.,1.6804428989482));
#30863=CARTESIAN_POINT('Ctrl Pts',(1.01561026162786,1.,1.6804428989482));
#30864=CARTESIAN_POINT('Ctrl Pts',(1.02006795074222,-1.,1.68440578021739));
#30865=CARTESIAN_POINT('Ctrl Pts',(1.02006795074222,1.,1.68440578021739));
#30866=CARTESIAN_POINT('Ctrl Pts',(1.02460180535272,-1.,1.68836910178475));
#30867=CARTESIAN_POINT('Ctrl Pts',(1.02460180535272,1.,1.68836910178475));
#30868=CARTESIAN_POINT('Ctrl Pts',(1.02919977579155,-1.,1.69231840863471));
#30869=CARTESIAN_POINT('Ctrl Pts',(1.02919977579155,1.,1.69231840863471));
#30870=CARTESIAN_POINT('Ctrl Pts',(1.03384646003587,-1.,1.69623414782769));
#30871=CARTESIAN_POINT('Ctrl Pts',(1.03384646003587,1.,1.69623414782769));
#30872=CARTESIAN_POINT('Ctrl Pts',(1.03852922490782,-1.,1.70010052930951));
#30873=CARTESIAN_POINT('Ctrl Pts',(1.03852922490782,1.,1.70010052930951));
#30874=CARTESIAN_POINT('Ctrl Pts',(1.04324363334546,-1.,1.70391338707969));
#30875=CARTESIAN_POINT('Ctrl Pts',(1.04324363334546,1.,1.70391338707969));
#30876=CARTESIAN_POINT('Ctrl Pts',(1.0479908540499,-1.,1.70767646263641));
#30877=CARTESIAN_POINT('Ctrl Pts',(1.0479908540499,1.,1.70767646263641));
#30878=CARTESIAN_POINT('Ctrl Pts',(1.05277517202853,-1.,1.71139783543986));
#30879=CARTESIAN_POINT('Ctrl Pts',(1.05277517202853,1.,1.71139783543986));
#30880=CARTESIAN_POINT('Ctrl Pts',(1.05760163192481,-1.,1.71508654427022));
#30881=CARTESIAN_POINT('Ctrl Pts',(1.05760163192481,1.,1.71508654427022));
#30882=CARTESIAN_POINT('Ctrl Pts',(1.06247324680649,-1.,1.71874858456908));
#30883=CARTESIAN_POINT('Ctrl Pts',(1.06247324680649,1.,1.71874858456908));
#30884=CARTESIAN_POINT('Ctrl Pts',(1.06738966975463,-1.,1.72238500928456));
#30885=CARTESIAN_POINT('Ctrl Pts',(1.06738966975463,1.,1.72238500928456));
#30886=CARTESIAN_POINT('Ctrl Pts',(1.07234866990252,-1.,1.72599406198489));
#30887=CARTESIAN_POINT('Ctrl Pts',(1.07234866990252,1.,1.72599406198489));
#30888=CARTESIAN_POINT('Ctrl Pts',(1.0773470373727,-1.,1.72957248977424));
#30889=CARTESIAN_POINT('Ctrl Pts',(1.0773470373727,1.,1.72957248977424));
#30890=CARTESIAN_POINT('Ctrl Pts',(1.08238162784749,-1.,1.73311705663407));
#30891=CARTESIAN_POINT('Ctrl Pts',(1.08238162784749,1.,1.73311705663407));
#30892=CARTESIAN_POINT('Ctrl Pts',(1.08745056285429,-1.,1.73662628326093));
#30893=CARTESIAN_POINT('Ctrl Pts',(1.08745056285429,1.,1.73662628326093));
#30894=CARTESIAN_POINT('Ctrl Pts',(1.09255329056496,-1.,1.74010053962252));
#30895=CARTESIAN_POINT('Ctrl Pts',(1.09255329056496,1.,1.74010053962252));
#30896=CARTESIAN_POINT('Ctrl Pts',(1.09768999241229,-1.,1.74354119236212));
#30897=CARTESIAN_POINT('Ctrl Pts',(1.09768999241229,1.,1.74354119236212));
#30898=CARTESIAN_POINT('Ctrl Pts',(1.10286118991144,-1.,1.74695004214924));
#30899=CARTESIAN_POINT('Ctrl Pts',(1.10286118991144,1.,1.74695004214924));
#30900=CARTESIAN_POINT('Ctrl Pts',(1.10806728183003,-1.,1.75032866075914));
#30901=CARTESIAN_POINT('Ctrl Pts',(1.10806728183003,1.,1.75032866075914));
#30902=CARTESIAN_POINT('Ctrl Pts',(1.11330807582542,-1.,1.75367772094617));
#30903=CARTESIAN_POINT('Ctrl Pts',(1.11330807582542,1.,1.75367772094617));
#30904=CARTESIAN_POINT('Ctrl Pts',(1.11858293216752,-1.,1.75699720772089));
#30905=CARTESIAN_POINT('Ctrl Pts',(1.11858293216752,1.,1.75699720772089));
#30906=CARTESIAN_POINT('Ctrl Pts',(1.12389096855078,-1.,1.76028671825084));
#30907=CARTESIAN_POINT('Ctrl Pts',(1.12389096855078,1.,1.76028671825084));
#30908=CARTESIAN_POINT('Ctrl Pts',(1.12923123555076,-1.,1.76354571966171));
#30909=CARTESIAN_POINT('Ctrl Pts',(1.12923123555076,1.,1.76354571966171));
#30910=CARTESIAN_POINT('Ctrl Pts',(1.13460291804634,-1.,1.76677384551883));
#30911=CARTESIAN_POINT('Ctrl Pts',(1.13460291804634,1.,1.76677384551883));
#30912=CARTESIAN_POINT('Ctrl Pts',(1.14000548337,-1.,1.76997111386806));
#30913=CARTESIAN_POINT('Ctrl Pts',(1.14000548337,1.,1.76997111386806));
#30914=CARTESIAN_POINT('Ctrl Pts',(1.14543858226948,-1.,1.77313777896234));
#30915=CARTESIAN_POINT('Ctrl Pts',(1.14543858226948,1.,1.77313777896234));
#30916=CARTESIAN_POINT('Ctrl Pts',(1.15090197841531,-1.,1.77627422557034));
#30917=CARTESIAN_POINT('Ctrl Pts',(1.15090197841531,1.,1.77627422557034));
#30918=CARTESIAN_POINT('Ctrl Pts',(1.15639547194689,-1.,1.77938085564261));
#30919=CARTESIAN_POINT('Ctrl Pts',(1.15639547194689,1.,1.77938085564261));
#30920=CARTESIAN_POINT('Ctrl Pts',(1.16191881298458,-1.,1.78245795880949));
#30921=CARTESIAN_POINT('Ctrl Pts',(1.16191881298458,1.,1.78245795880949));
#30922=CARTESIAN_POINT('Ctrl Pts',(1.16747166312239,-1.,1.78550566040349));
#30923=CARTESIAN_POINT('Ctrl Pts',(1.16747166312239,1.,1.78550566040349));
#30924=CARTESIAN_POINT('Ctrl Pts',(1.17305363177265,-1.,1.78852398877523));
#30925=CARTESIAN_POINT('Ctrl Pts',(1.17305363177265,1.,1.78852398877523));
#30926=CARTESIAN_POINT('Ctrl Pts',(1.17866429440781,-1.,1.79151291552646));
#30927=CARTESIAN_POINT('Ctrl Pts',(1.17866429440781,1.,1.79151291552646));
#30928=CARTESIAN_POINT('Ctrl Pts',(1.18430321697471,-1.,1.79447240321572));
#30929=CARTESIAN_POINT('Ctrl Pts',(1.18430321697471,1.,1.79447240321572));
#30930=CARTESIAN_POINT('Ctrl Pts',(1.1899699793456,-1.,1.79740245923649));
#30931=CARTESIAN_POINT('Ctrl Pts',(1.1899699793456,1.,1.79740245923649));
#30932=CARTESIAN_POINT('Ctrl Pts',(1.19566418930405,-1.,1.80030314370121));
#30933=CARTESIAN_POINT('Ctrl Pts',(1.19566418930405,1.,1.80030314370121));
#30934=CARTESIAN_POINT('Ctrl Pts',(1.2013854893912,-1.,1.8031745483882));
#30935=CARTESIAN_POINT('Ctrl Pts',(1.2013854893912,1.,1.8031745483882));
#30936=CARTESIAN_POINT('Ctrl Pts',(1.20713356605519,-1.,1.80601678480772));
#30937=CARTESIAN_POINT('Ctrl Pts',(1.20713356605519,1.,1.80601678480772));
#30938=CARTESIAN_POINT('Ctrl Pts',(1.2129081570818,-1.,1.80882996916931));
#30939=CARTESIAN_POINT('Ctrl Pts',(1.2129081570818,1.,1.80882996916931));
#30940=CARTESIAN_POINT('Ctrl Pts',(1.2187090610323,-1.,1.81161420806172));
#30941=CARTESIAN_POINT('Ctrl Pts',(1.2187090610323,1.,1.81161420806172));
#30942=CARTESIAN_POINT('Ctrl Pts',(1.22453613304507,-1.,1.81436959209778));
#30943=CARTESIAN_POINT('Ctrl Pts',(1.22453613304507,1.,1.81436959209778));
#30944=CARTESIAN_POINT('Ctrl Pts',(1.22921864890975,-1.,1.81655087183054));
#30945=CARTESIAN_POINT('Ctrl Pts',(1.22921864890975,1.,1.81655087183054));
#30946=CARTESIAN_POINT('Ctrl Pts',(1.23274224526804,-1.,1.81817389920914));
#30947=CARTESIAN_POINT('Ctrl Pts',(1.23274224526804,1.,1.81817389920914));
#30948=CARTESIAN_POINT('Ctrl Pts',(1.23509651170384,-1.,1.81925017193531));
#30949=CARTESIAN_POINT('Ctrl Pts',(1.23509651170384,1.,1.81925017193531));
#30950=CARTESIAN_POINT('Ctrl Pts',(1.23627494547115,-1.,1.81978687191668));
#30951=CARTESIAN_POINT('Ctrl Pts',(1.23627494547115,1.,1.81978687191668));
#30952=CARTESIAN_POINT('',(0.892032620296855,1.,1.5055822144029));
#30953=CARTESIAN_POINT('Ctrl Pts',(0.892032620296855,1.,1.5055822144029));
#30954=CARTESIAN_POINT('Ctrl Pts',(0.894452006967538,1.,1.50980486807181));
#30955=CARTESIAN_POINT('Ctrl Pts',(0.89918504749193,1.,1.51805569591479));
#30956=CARTESIAN_POINT('Ctrl Pts',(0.905967409640498,1.,1.52984849890434));
#30957=CARTESIAN_POINT('Ctrl Pts',(0.914375919046579,1.,1.54440491152808));
#30958=CARTESIAN_POINT('Ctrl Pts',(0.923832188966322,1.,1.56065988582509));
#30959=CARTESIAN_POINT('Ctrl Pts',(0.932246680128848,1.,1.57499388385561));
#30960=CARTESIAN_POINT('Ctrl Pts',(0.939646377909319,1.,1.58744937489796));
#30961=CARTESIAN_POINT('Ctrl Pts',(0.946078063325795,1.,1.59810042045408));
#30962=CARTESIAN_POINT('Ctrl Pts',(0.951613284361247,1.,1.60706069897794));
#30963=CARTESIAN_POINT('Ctrl Pts',(0.956354422921572,1.,1.61449324337233));
#30964=CARTESIAN_POINT('Ctrl Pts',(0.960438326099958,1.,1.62061638139929));
#30965=CARTESIAN_POINT('Ctrl Pts',(0.964046107037821,1.,1.6257193066974));
#30966=CARTESIAN_POINT('Ctrl Pts',(0.967387853228041,1.,1.63013849959083));
#30967=CARTESIAN_POINT('Ctrl Pts',(0.970669715996356,1.,1.63420665729609));
#30968=CARTESIAN_POINT('Ctrl Pts',(0.974066058287501,1.,1.63820952658157));
#30969=CARTESIAN_POINT('Ctrl Pts',(0.977689794120296,1.,1.64233990826831));
#30970=CARTESIAN_POINT('Ctrl Pts',(0.981562530940574,1.,1.64665139190834));
#30971=CARTESIAN_POINT('Ctrl Pts',(0.985642622921626,1.,1.6511001661277));
#30972=CARTESIAN_POINT('Ctrl Pts',(0.98985562785445,1.,1.65559044289746));
#30973=CARTESIAN_POINT('Ctrl Pts',(0.994121836661115,1.,1.66001553809916));
#30974=CARTESIAN_POINT('Ctrl Pts',(0.998389654952317,1.,1.66430758030304));
#30975=CARTESIAN_POINT('Ctrl Pts',(1.00265091003682,1.,1.66846059277231));
#30976=CARTESIAN_POINT('Ctrl Pts',(1.00692206696387,1.,1.67250335383248));
#30977=CARTESIAN_POINT('Ctrl Pts',(1.01123236493507,1.,1.67648246776457));
#30978=CARTESIAN_POINT('Ctrl Pts',(1.01561026162786,1.,1.6804428989482));
#30979=CARTESIAN_POINT('Ctrl Pts',(1.02006795074222,1.,1.68440578021739));
#30980=CARTESIAN_POINT('Ctrl Pts',(1.02460180535272,1.,1.68836910178475));
#30981=CARTESIAN_POINT('Ctrl Pts',(1.02919977579155,1.,1.69231840863471));
#30982=CARTESIAN_POINT('Ctrl Pts',(1.03384646003587,1.,1.69623414782769));
#30983=CARTESIAN_POINT('Ctrl Pts',(1.03852922490782,1.,1.70010052930951));
#30984=CARTESIAN_POINT('Ctrl Pts',(1.04324363334546,1.,1.70391338707969));
#30985=CARTESIAN_POINT('Ctrl Pts',(1.0479908540499,1.,1.70767646263641));
#30986=CARTESIAN_POINT('Ctrl Pts',(1.05277517202853,1.,1.71139783543986));
#30987=CARTESIAN_POINT('Ctrl Pts',(1.05760163192481,1.,1.71508654427022));
#30988=CARTESIAN_POINT('Ctrl Pts',(1.06247324680649,1.,1.71874858456908));
#30989=CARTESIAN_POINT('Ctrl Pts',(1.06738966975463,1.,1.72238500928456));
#30990=CARTESIAN_POINT('Ctrl Pts',(1.07234866990252,1.,1.72599406198489));
#30991=CARTESIAN_POINT('Ctrl Pts',(1.0773470373727,1.,1.72957248977424));
#30992=CARTESIAN_POINT('Ctrl Pts',(1.08238162784749,1.,1.73311705663407));
#30993=CARTESIAN_POINT('Ctrl Pts',(1.08745056285429,1.,1.73662628326093));
#30994=CARTESIAN_POINT('Ctrl Pts',(1.09255329056496,1.,1.74010053962252));
#30995=CARTESIAN_POINT('Ctrl Pts',(1.09768999241229,1.,1.74354119236212));
#30996=CARTESIAN_POINT('Ctrl Pts',(1.10286118991144,1.,1.74695004214924));
#30997=CARTESIAN_POINT('Ctrl Pts',(1.10806728183003,1.,1.75032866075914));
#30998=CARTESIAN_POINT('Ctrl Pts',(1.11330807582542,1.,1.75367772094617));
#30999=CARTESIAN_POINT('Ctrl Pts',(1.11858293216752,1.,1.75699720772089));
#31000=CARTESIAN_POINT('Ctrl Pts',(1.12389096855078,1.,1.76028671825084));
#31001=CARTESIAN_POINT('Ctrl Pts',(1.12923123555076,1.,1.76354571966171));
#31002=CARTESIAN_POINT('Ctrl Pts',(1.13460291804634,1.,1.76677384551883));
#31003=CARTESIAN_POINT('Ctrl Pts',(1.14000548337,1.,1.76997111386806));
#31004=CARTESIAN_POINT('Ctrl Pts',(1.14543858226948,1.,1.77313777896234));
#31005=CARTESIAN_POINT('Ctrl Pts',(1.15090197841531,1.,1.77627422557034));
#31006=CARTESIAN_POINT('Ctrl Pts',(1.15639547194689,1.,1.77938085564261));
#31007=CARTESIAN_POINT('Ctrl Pts',(1.16191881298458,1.,1.78245795880949));
#31008=CARTESIAN_POINT('Ctrl Pts',(1.16747166312239,1.,1.78550566040349));
#31009=CARTESIAN_POINT('Ctrl Pts',(1.17305363177265,1.,1.78852398877523));
#31010=CARTESIAN_POINT('Ctrl Pts',(1.17866429440781,1.,1.79151291552646));
#31011=CARTESIAN_POINT('Ctrl Pts',(1.18430321697471,1.,1.79447240321572));
#31012=CARTESIAN_POINT('Ctrl Pts',(1.1899699793456,1.,1.79740245923649));
#31013=CARTESIAN_POINT('Ctrl Pts',(1.19566418930405,1.,1.80030314370121));
#31014=CARTESIAN_POINT('Ctrl Pts',(1.2013854893912,1.,1.8031745483882));
#31015=CARTESIAN_POINT('Ctrl Pts',(1.20713356605519,1.,1.80601678480772));
#31016=CARTESIAN_POINT('Ctrl Pts',(1.2129081570818,1.,1.80882996916931));
#31017=CARTESIAN_POINT('Ctrl Pts',(1.2187090610323,1.,1.81161420806172));
#31018=CARTESIAN_POINT('Ctrl Pts',(1.22453613304507,1.,1.81436959209778));
#31019=CARTESIAN_POINT('Ctrl Pts',(1.22921864890975,1.,1.81655087183054));
#31020=CARTESIAN_POINT('Ctrl Pts',(1.23274224526804,1.,1.81817389920914));
#31021=CARTESIAN_POINT('Ctrl Pts',(1.23509651170384,1.,1.81925017193531));
#31022=CARTESIAN_POINT('Ctrl Pts',(1.23627494547115,1.,1.81978687191668));
#31023=CARTESIAN_POINT('',(0.892032620296854,0.,1.5055822144029));
#31024=CARTESIAN_POINT('Origin',(0.,0.,0.));
#31025=CARTESIAN_POINT('',(0.693717979106305,1.,1.60662857109684));
#31026=CARTESIAN_POINT('Origin',(0.,1.,0.));
#31027=CARTESIAN_POINT('',(0.693717979106305,0.,1.60662857109684));
#31028=CARTESIAN_POINT('Ctrl Pts',(0.7455743247944,-1.,2.0698113262342));
#31029=CARTESIAN_POINT('Ctrl Pts',(0.7455743247944,1.,2.0698113262342));
#31030=CARTESIAN_POINT('Ctrl Pts',(0.745832791378367,-1.,2.06854248895728));
#31031=CARTESIAN_POINT('Ctrl Pts',(0.745832791378367,1.,2.06854248895728));
#31032=CARTESIAN_POINT('Ctrl Pts',(0.7463458715442,-1.,2.06600523016815));
#31033=CARTESIAN_POINT('Ctrl Pts',(0.7463458715442,1.,2.06600523016815));
#31034=CARTESIAN_POINT('Ctrl Pts',(0.747103932787919,-1.,2.06220058927826));
#31035=CARTESIAN_POINT('Ctrl Pts',(0.747103932787919,1.,2.06220058927826));
#31036=CARTESIAN_POINT('Ctrl Pts',(0.748091554183802,-1.,2.05713023031007));
#31037=CARTESIAN_POINT('Ctrl Pts',(0.748091554183802,1.,2.05713023031007));
#31038=CARTESIAN_POINT('Ctrl Pts',(0.749287468665046,-1.,2.05079645592154));
#31039=CARTESIAN_POINT('Ctrl Pts',(0.749287468665046,1.,2.05079645592154));
#31040=CARTESIAN_POINT('Ctrl Pts',(0.750444657875575,-1.,2.04446689147979));
#31041=CARTESIAN_POINT('Ctrl Pts',(0.750444657875575,1.,2.04446689147979));
#31042=CARTESIAN_POINT('Ctrl Pts',(0.751562963361115,-1.,2.03814160092099));
#31043=CARTESIAN_POINT('Ctrl Pts',(0.751562963361115,1.,2.03814160092099));
#31044=CARTESIAN_POINT('Ctrl Pts',(0.75264218048721,-1.,2.03182068456221));
#31045=CARTESIAN_POINT('Ctrl Pts',(0.75264218048721,1.,2.03182068456221));
#31046=CARTESIAN_POINT('Ctrl Pts',(0.753682061112768,-1.,2.02550428623313));
#31047=CARTESIAN_POINT('Ctrl Pts',(0.753682061112768,1.,2.02550428623313));
#31048=CARTESIAN_POINT('Ctrl Pts',(0.754682330722816,-1.,2.01919259405809));
#31049=CARTESIAN_POINT('Ctrl Pts',(0.754682330722816,1.,2.01919259405809));
#31050=CARTESIAN_POINT('Ctrl Pts',(0.755642704957865,-1.,2.01288584328084));
#31051=CARTESIAN_POINT('Ctrl Pts',(0.755642704957865,1.,2.01288584328084));
#31052=CARTESIAN_POINT('Ctrl Pts',(0.75656290464667,-1.,2.0065843158773));
#31053=CARTESIAN_POINT('Ctrl Pts',(0.75656290464667,1.,2.0065843158773));
#31054=CARTESIAN_POINT('Ctrl Pts',(0.757442676862724,-1.,2.00028834739178));
#31055=CARTESIAN_POINT('Ctrl Pts',(0.757442676862724,1.,2.00028834739178));
#31056=CARTESIAN_POINT('Ctrl Pts',(0.758281796766761,-1.,1.99399831098817));
#31057=CARTESIAN_POINT('Ctrl Pts',(0.758281796766761,1.,1.99399831098817));
#31058=CARTESIAN_POINT('Ctrl Pts',(0.759080037802488,-1.,1.98771456680874));
#31059=CARTESIAN_POINT('Ctrl Pts',(0.759080037802488,1.,1.98771456680874));
#31060=CARTESIAN_POINT('Ctrl Pts',(0.75983714745219,-1.,1.98143741418172));
#31061=CARTESIAN_POINT('Ctrl Pts',(0.75983714745219,1.,1.98143741418172));
#31062=CARTESIAN_POINT('Ctrl Pts',(0.760552825409757,-1.,1.97516705321494));
#31063=CARTESIAN_POINT('Ctrl Pts',(0.760552825409757,1.,1.97516705321494));
#31064=CARTESIAN_POINT('Ctrl Pts',(0.76122669048382,-1.,1.96890351582499));
#31065=CARTESIAN_POINT('Ctrl Pts',(0.76122669048382,1.,1.96890351582499));
#31066=CARTESIAN_POINT('Ctrl Pts',(0.761858300014423,-1.,1.96264672744186));
#31067=CARTESIAN_POINT('Ctrl Pts',(0.761858300014423,1.,1.96264672744186));
#31068=CARTESIAN_POINT('Ctrl Pts',(0.762447203806178,-1.,1.95639665309869));
#31069=CARTESIAN_POINT('Ctrl Pts',(0.762447203806178,1.,1.95639665309869));
#31070=CARTESIAN_POINT('Ctrl Pts',(0.762992990878769,-1.,1.95015342590024));
#31071=CARTESIAN_POINT('Ctrl Pts',(0.762992990878769,1.,1.95015342590024));
#31072=CARTESIAN_POINT('Ctrl Pts',(0.763495333538629,-1.,1.9439174661764));
#31073=CARTESIAN_POINT('Ctrl Pts',(0.763495333538629,1.,1.9439174661764));
#31074=CARTESIAN_POINT('Ctrl Pts',(0.763954049121458,-1.,1.93768964875886));
#31075=CARTESIAN_POINT('Ctrl Pts',(0.763954049121458,1.,1.93768964875886));
#31076=CARTESIAN_POINT('Ctrl Pts',(0.76436901067394,-1.,1.93147105496382));
#31077=CARTESIAN_POINT('Ctrl Pts',(0.76436901067394,1.,1.93147105496382));
#31078=CARTESIAN_POINT('Ctrl Pts',(0.764740025488211,-1.,1.92526263537048));
#31079=CARTESIAN_POINT('Ctrl Pts',(0.764740025488211,1.,1.92526263537048));
#31080=CARTESIAN_POINT('Ctrl Pts',(0.765066729667088,-1.,1.91906491634196));
#31081=CARTESIAN_POINT('Ctrl Pts',(0.765066729667088,1.,1.91906491634196));
#31082=CARTESIAN_POINT('Ctrl Pts',(0.765348465884722,-1.,1.91287765805169));
#31083=CARTESIAN_POINT('Ctrl Pts',(0.765348465884722,1.,1.91287765805169));
#31084=CARTESIAN_POINT('Ctrl Pts',(0.765584196937919,-1.,1.90669961402356));
#31085=CARTESIAN_POINT('Ctrl Pts',(0.765584196937919,1.,1.90669961402356));
#31086=CARTESIAN_POINT('Ctrl Pts',(0.765772772593386,-1.,1.90052930393596));
#31087=CARTESIAN_POINT('Ctrl Pts',(0.765772772593386,1.,1.90052930393596));
#31088=CARTESIAN_POINT('Ctrl Pts',(0.765913193856978,-1.,1.89436577771388));
#31089=CARTESIAN_POINT('Ctrl Pts',(0.765913193856978,1.,1.89436577771388));
#31090=CARTESIAN_POINT('Ctrl Pts',(0.766004837062091,-1.,1.88820926433409));
#31091=CARTESIAN_POINT('Ctrl Pts',(0.766004837062091,1.,1.88820926433409));
#31092=CARTESIAN_POINT('Ctrl Pts',(0.766047794851864,-1.,1.88206215302561));
#31093=CARTESIAN_POINT('Ctrl Pts',(0.766047794851864,1.,1.88206215302561));
#31094=CARTESIAN_POINT('Ctrl Pts',(0.766042837036744,-1.,1.87592888967883));
#31095=CARTESIAN_POINT('Ctrl Pts',(0.766042837036744,1.,1.87592888967883));
#31096=CARTESIAN_POINT('Ctrl Pts',(0.765990708546091,-1.,1.86981398314341));
#31097=CARTESIAN_POINT('Ctrl Pts',(0.765990708546091,1.,1.86981398314341));
#31098=CARTESIAN_POINT('Ctrl Pts',(0.765891519092547,-1.,1.86372027063312));
#31099=CARTESIAN_POINT('Ctrl Pts',(0.765891519092547,1.,1.86372027063312));
#31100=CARTESIAN_POINT('Ctrl Pts',(0.765744212909318,-1.,1.85764741390394));
#31101=CARTESIAN_POINT('Ctrl Pts',(0.765744212909318,1.,1.85764741390394));
#31102=CARTESIAN_POINT('Ctrl Pts',(0.765545710619062,-1.,1.85158945130063));
#31103=CARTESIAN_POINT('Ctrl Pts',(0.765545710619062,1.,1.85158945130063));
#31104=CARTESIAN_POINT('Ctrl Pts',(0.765291664862029,-1.,1.84553698875924));
#31105=CARTESIAN_POINT('Ctrl Pts',(0.765291664862029,1.,1.84553698875924));
#31106=CARTESIAN_POINT('Ctrl Pts',(0.764978057881737,-1.,1.83948181064835));
#31107=CARTESIAN_POINT('Ctrl Pts',(0.764978057881737,1.,1.83948181064835));
#31108=CARTESIAN_POINT('Ctrl Pts',(0.764602549687853,-1.,1.83342077227142));
#31109=CARTESIAN_POINT('Ctrl Pts',(0.764602549687853,1.,1.83342077227142));
#31110=CARTESIAN_POINT('Ctrl Pts',(0.764165902605995,-1.,1.82735991200065));
#31111=CARTESIAN_POINT('Ctrl Pts',(0.764165902605995,1.,1.82735991200065));
#31112=CARTESIAN_POINT('Ctrl Pts',(0.763673465462726,-1.,1.82131873145266));
#31113=CARTESIAN_POINT('Ctrl Pts',(0.763673465462726,1.,1.82131873145266));
#31114=CARTESIAN_POINT('Ctrl Pts',(0.763132003836634,-1.,1.8153211840553));
#31115=CARTESIAN_POINT('Ctrl Pts',(0.763132003836634,1.,1.8153211840553));
#31116=CARTESIAN_POINT('Ctrl Pts',(0.762546129463938,-1.,1.80938551463965));
#31117=CARTESIAN_POINT('Ctrl Pts',(0.762546129463938,1.,1.80938551463965));
#31118=CARTESIAN_POINT('Ctrl Pts',(0.761915336443547,-1.,1.80351583877342));
#31119=CARTESIAN_POINT('Ctrl Pts',(0.761915336443547,1.,1.80351583877342));
#31120=CARTESIAN_POINT('Ctrl Pts',(0.761229695230558,-1.,1.79768986997783));
#31121=CARTESIAN_POINT('Ctrl Pts',(0.761229695230558,1.,1.79768986997783));
#31122=CARTESIAN_POINT('Ctrl Pts',(0.760469555880749,-1.,1.7918581561088));
#31123=CARTESIAN_POINT('Ctrl Pts',(0.760469555880749,1.,1.7918581561088));
#31124=CARTESIAN_POINT('Ctrl Pts',(0.759614401110189,-1.,1.78596964884604));
#31125=CARTESIAN_POINT('Ctrl Pts',(0.759614401110189,1.,1.78596964884604));
#31126=CARTESIAN_POINT('Ctrl Pts',(0.758650626677518,-1.,1.77999411220945));
#31127=CARTESIAN_POINT('Ctrl Pts',(0.758650626677518,1.,1.77999411220945));
#31128=CARTESIAN_POINT('Ctrl Pts',(0.757578264077028,-1.,1.77394167108292));
#31129=CARTESIAN_POINT('Ctrl Pts',(0.757578264077028,1.,1.77394167108292));
#31130=CARTESIAN_POINT('Ctrl Pts',(0.75642189602781,-1.,1.76789396002998));
#31131=CARTESIAN_POINT('Ctrl Pts',(0.75642189602781,1.,1.76789396002998));
#31132=CARTESIAN_POINT('Ctrl Pts',(0.755220979974461,-1.,1.76197817240128));
#31133=CARTESIAN_POINT('Ctrl Pts',(0.755220979974461,1.,1.76197817240128));
#31134=CARTESIAN_POINT('Ctrl Pts',(0.754009254027828,-1.,1.75631083600019));
#31135=CARTESIAN_POINT('Ctrl Pts',(0.754009254027828,1.,1.75631083600019));
#31136=CARTESIAN_POINT('Ctrl Pts',(0.752797683531314,-1.,1.75095139468794));
#31137=CARTESIAN_POINT('Ctrl Pts',(0.752797683531314,1.,1.75095139468794));
#31138=CARTESIAN_POINT('Ctrl Pts',(0.751555614164482,-1.,1.74585086852502));
#31139=CARTESIAN_POINT('Ctrl Pts',(0.751555614164482,1.,1.74585086852502));
#31140=CARTESIAN_POINT('Ctrl Pts',(0.750193435981249,-1.,1.74080458267114));
#31141=CARTESIAN_POINT('Ctrl Pts',(0.750193435981249,1.,1.74080458267114));
#31142=CARTESIAN_POINT('Ctrl Pts',(0.74858246295687,-1.,1.7355035168033));
#31143=CARTESIAN_POINT('Ctrl Pts',(0.74858246295687,1.,1.7355035168033));
#31144=CARTESIAN_POINT('Ctrl Pts',(0.746574710097752,-1.,1.72958533647714));
#31145=CARTESIAN_POINT('Ctrl Pts',(0.746574710097752,1.,1.72958533647714));
#31146=CARTESIAN_POINT('Ctrl Pts',(0.744021445433093,-1.,1.72268229916769));
#31147=CARTESIAN_POINT('Ctrl Pts',(0.744021445433093,1.,1.72268229916769));
#31148=CARTESIAN_POINT('Ctrl Pts',(0.74079516202821,-1.,1.71447789751001));
#31149=CARTESIAN_POINT('Ctrl Pts',(0.74079516202821,1.,1.71447789751001));
#31150=CARTESIAN_POINT('Ctrl Pts',(0.736799665716932,-1.,1.70473309004249));
#31151=CARTESIAN_POINT('Ctrl Pts',(0.736799665716932,1.,1.70473309004249));
#31152=CARTESIAN_POINT('Ctrl Pts',(0.731963238685357,-1.,1.69326921972915));
#31153=CARTESIAN_POINT('Ctrl Pts',(0.731963238685357,1.,1.69326921972915));
#31154=CARTESIAN_POINT('Ctrl Pts',(0.726235967982445,-1.,1.67996158451922));
#31155=CARTESIAN_POINT('Ctrl Pts',(0.726235967982445,1.,1.67996158451922));
#31156=CARTESIAN_POINT('Ctrl Pts',(0.719585433787949,-1.,1.66472880551777));
#31157=CARTESIAN_POINT('Ctrl Pts',(0.719585433787949,1.,1.66472880551777));
#31158=CARTESIAN_POINT('Ctrl Pts',(0.711993139340447,-1.,1.64752408828442));
#31159=CARTESIAN_POINT('Ctrl Pts',(0.711993139340447,1.,1.64752408828442));
#31160=CARTESIAN_POINT('Ctrl Pts',(0.705159151977294,-1.,1.6321654166204));
#31161=CARTESIAN_POINT('Ctrl Pts',(0.705159151977294,1.,1.6321654166204));
#31162=CARTESIAN_POINT('Ctrl Pts',(0.699605146398836,-1.,1.61974673471117));
#31163=CARTESIAN_POINT('Ctrl Pts',(0.699605146398836,1.,1.61974673471117));
#31164=CARTESIAN_POINT('Ctrl Pts',(0.69571209787897,-1.,1.61106790957619));
#31165=CARTESIAN_POINT('Ctrl Pts',(0.69571209787897,1.,1.61106790957619));
#31166=CARTESIAN_POINT('Ctrl Pts',(0.693717979106305,-1.,1.60662857109684));
#31167=CARTESIAN_POINT('Ctrl Pts',(0.693717979106305,1.,1.60662857109684));
#31168=CARTESIAN_POINT('',(0.7455743247944,1.,2.0698113262342));
#31169=CARTESIAN_POINT('Ctrl Pts',(0.7455743247944,1.,2.0698113262342));
#31170=CARTESIAN_POINT('Ctrl Pts',(0.745832791378367,1.,2.06854248895728));
#31171=CARTESIAN_POINT('Ctrl Pts',(0.7463458715442,1.,2.06600523016815));
#31172=CARTESIAN_POINT('Ctrl Pts',(0.747103932787919,1.,2.06220058927826));
#31173=CARTESIAN_POINT('Ctrl Pts',(0.748091554183802,1.,2.05713023031007));
#31174=CARTESIAN_POINT('Ctrl Pts',(0.749287468665046,1.,2.05079645592154));
#31175=CARTESIAN_POINT('Ctrl Pts',(0.750444657875575,1.,2.04446689147979));
#31176=CARTESIAN_POINT('Ctrl Pts',(0.751562963361115,1.,2.03814160092099));
#31177=CARTESIAN_POINT('Ctrl Pts',(0.75264218048721,1.,2.03182068456221));
#31178=CARTESIAN_POINT('Ctrl Pts',(0.753682061112768,1.,2.02550428623313));
#31179=CARTESIAN_POINT('Ctrl Pts',(0.754682330722816,1.,2.01919259405809));
#31180=CARTESIAN_POINT('Ctrl Pts',(0.755642704957865,1.,2.01288584328084));
#31181=CARTESIAN_POINT('Ctrl Pts',(0.75656290464667,1.,2.0065843158773));
#31182=CARTESIAN_POINT('Ctrl Pts',(0.757442676862724,1.,2.00028834739178));
#31183=CARTESIAN_POINT('Ctrl Pts',(0.758281796766761,1.,1.99399831098817));
#31184=CARTESIAN_POINT('Ctrl Pts',(0.759080037802488,1.,1.98771456680874));
#31185=CARTESIAN_POINT('Ctrl Pts',(0.75983714745219,1.,1.98143741418172));
#31186=CARTESIAN_POINT('Ctrl Pts',(0.760552825409757,1.,1.97516705321494));
#31187=CARTESIAN_POINT('Ctrl Pts',(0.76122669048382,1.,1.96890351582499));
#31188=CARTESIAN_POINT('Ctrl Pts',(0.761858300014423,1.,1.96264672744186));
#31189=CARTESIAN_POINT('Ctrl Pts',(0.762447203806178,1.,1.95639665309869));
#31190=CARTESIAN_POINT('Ctrl Pts',(0.762992990878769,1.,1.95015342590024));
#31191=CARTESIAN_POINT('Ctrl Pts',(0.763495333538629,1.,1.9439174661764));
#31192=CARTESIAN_POINT('Ctrl Pts',(0.763954049121458,1.,1.93768964875886));
#31193=CARTESIAN_POINT('Ctrl Pts',(0.76436901067394,1.,1.93147105496382));
#31194=CARTESIAN_POINT('Ctrl Pts',(0.764740025488211,1.,1.92526263537048));
#31195=CARTESIAN_POINT('Ctrl Pts',(0.765066729667088,1.,1.91906491634196));
#31196=CARTESIAN_POINT('Ctrl Pts',(0.765348465884722,1.,1.91287765805169));
#31197=CARTESIAN_POINT('Ctrl Pts',(0.765584196937919,1.,1.90669961402356));
#31198=CARTESIAN_POINT('Ctrl Pts',(0.765772772593386,1.,1.90052930393596));
#31199=CARTESIAN_POINT('Ctrl Pts',(0.765913193856978,1.,1.89436577771388));
#31200=CARTESIAN_POINT('Ctrl Pts',(0.766004837062091,1.,1.88820926433409));
#31201=CARTESIAN_POINT('Ctrl Pts',(0.766047794851864,1.,1.88206215302561));
#31202=CARTESIAN_POINT('Ctrl Pts',(0.766042837036744,1.,1.87592888967883));
#31203=CARTESIAN_POINT('Ctrl Pts',(0.765990708546091,1.,1.86981398314341));
#31204=CARTESIAN_POINT('Ctrl Pts',(0.765891519092547,1.,1.86372027063312));
#31205=CARTESIAN_POINT('Ctrl Pts',(0.765744212909318,1.,1.85764741390394));
#31206=CARTESIAN_POINT('Ctrl Pts',(0.765545710619062,1.,1.85158945130063));
#31207=CARTESIAN_POINT('Ctrl Pts',(0.765291664862029,1.,1.84553698875924));
#31208=CARTESIAN_POINT('Ctrl Pts',(0.764978057881737,1.,1.83948181064835));
#31209=CARTESIAN_POINT('Ctrl Pts',(0.764602549687853,1.,1.83342077227142));
#31210=CARTESIAN_POINT('Ctrl Pts',(0.764165902605995,1.,1.82735991200065));
#31211=CARTESIAN_POINT('Ctrl Pts',(0.763673465462726,1.,1.82131873145266));
#31212=CARTESIAN_POINT('Ctrl Pts',(0.763132003836634,1.,1.8153211840553));
#31213=CARTESIAN_POINT('Ctrl Pts',(0.762546129463938,1.,1.80938551463965));
#31214=CARTESIAN_POINT('Ctrl Pts',(0.761915336443547,1.,1.80351583877342));
#31215=CARTESIAN_POINT('Ctrl Pts',(0.761229695230558,1.,1.79768986997783));
#31216=CARTESIAN_POINT('Ctrl Pts',(0.760469555880749,1.,1.7918581561088));
#31217=CARTESIAN_POINT('Ctrl Pts',(0.759614401110189,1.,1.78596964884604));
#31218=CARTESIAN_POINT('Ctrl Pts',(0.758650626677518,1.,1.77999411220945));
#31219=CARTESIAN_POINT('Ctrl Pts',(0.757578264077028,1.,1.77394167108292));
#31220=CARTESIAN_POINT('Ctrl Pts',(0.75642189602781,1.,1.76789396002998));
#31221=CARTESIAN_POINT('Ctrl Pts',(0.755220979974461,1.,1.76197817240128));
#31222=CARTESIAN_POINT('Ctrl Pts',(0.754009254027828,1.,1.75631083600019));
#31223=CARTESIAN_POINT('Ctrl Pts',(0.752797683531314,1.,1.75095139468794));
#31224=CARTESIAN_POINT('Ctrl Pts',(0.751555614164482,1.,1.74585086852502));
#31225=CARTESIAN_POINT('Ctrl Pts',(0.750193435981249,1.,1.74080458267114));
#31226=CARTESIAN_POINT('Ctrl Pts',(0.74858246295687,1.,1.7355035168033));
#31227=CARTESIAN_POINT('Ctrl Pts',(0.746574710097752,1.,1.72958533647714));
#31228=CARTESIAN_POINT('Ctrl Pts',(0.744021445433093,1.,1.72268229916769));
#31229=CARTESIAN_POINT('Ctrl Pts',(0.74079516202821,1.,1.71447789751001));
#31230=CARTESIAN_POINT('Ctrl Pts',(0.736799665716932,1.,1.70473309004249));
#31231=CARTESIAN_POINT('Ctrl Pts',(0.731963238685357,1.,1.69326921972915));
#31232=CARTESIAN_POINT('Ctrl Pts',(0.726235967982445,1.,1.67996158451922));
#31233=CARTESIAN_POINT('Ctrl Pts',(0.719585433787949,1.,1.66472880551777));
#31234=CARTESIAN_POINT('Ctrl Pts',(0.711993139340447,1.,1.64752408828442));
#31235=CARTESIAN_POINT('Ctrl Pts',(0.705159151977294,1.,1.6321654166204));
#31236=CARTESIAN_POINT('Ctrl Pts',(0.699605146398836,1.,1.61974673471117));
#31237=CARTESIAN_POINT('Ctrl Pts',(0.69571209787897,1.,1.61106790957619));
#31238=CARTESIAN_POINT('Ctrl Pts',(0.693717979106305,1.,1.60662857109684));
#31239=CARTESIAN_POINT('',(0.7455743247944,0.,2.0698113262342));
#31240=CARTESIAN_POINT('Origin',(0.61342227326009,0.,2.11275013067528));
#31241=CARTESIAN_POINT('',(0.61342227326009,1.,2.11275013067528));
#31242=CARTESIAN_POINT('',(0.7455743247944,1.,2.0698113262342));
#31243=CARTESIAN_POINT('',(0.61342227326009,0.,2.11275013067528));
#31244=CARTESIAN_POINT('Ctrl Pts',(0.383122945602004,-1.,1.7075470150345));
#31245=CARTESIAN_POINT('Ctrl Pts',(0.383122945602004,1.,1.7075470150345));
#31246=CARTESIAN_POINT('Ctrl Pts',(0.384119047315541,-1.,1.71231062891958));
#31247=CARTESIAN_POINT('Ctrl Pts',(0.384119047315541,1.,1.71231062891958));
#31248=CARTESIAN_POINT('Ctrl Pts',(0.38607079032701,-1.,1.72162022246158));
#31249=CARTESIAN_POINT('Ctrl Pts',(0.38607079032701,1.,1.72162022246158));
#31250=CARTESIAN_POINT('Ctrl Pts',(0.388877023509191,-1.,1.7349317097561));
#31251=CARTESIAN_POINT('Ctrl Pts',(0.388877023509191,1.,1.7349317097561));
#31252=CARTESIAN_POINT('Ctrl Pts',(0.392375812294307,-1.,1.75137405313962));
#31253=CARTESIAN_POINT('Ctrl Pts',(0.392375812294307,1.,1.75137405313962));
#31254=CARTESIAN_POINT('Ctrl Pts',(0.39634619612042,-1.,1.7697556004756));
#31255=CARTESIAN_POINT('Ctrl Pts',(0.39634619612042,1.,1.7697556004756));
#31256=CARTESIAN_POINT('Ctrl Pts',(0.39991940378308,-1.,1.78598826347533));
#31257=CARTESIAN_POINT('Ctrl Pts',(0.39991940378308,1.,1.78598826347533));
#31258=CARTESIAN_POINT('Ctrl Pts',(0.403107976170441,-1.,1.80012077176221));
#31259=CARTESIAN_POINT('Ctrl Pts',(0.403107976170441,1.,1.80012077176221));
#31260=CARTESIAN_POINT('Ctrl Pts',(0.405933518411838,-1.,1.81223801813988));
#31261=CARTESIAN_POINT('Ctrl Pts',(0.405933518411838,1.,1.81223801813988));
#31262=CARTESIAN_POINT('Ctrl Pts',(0.408428948108533,-1.,1.8224702267854));
#31263=CARTESIAN_POINT('Ctrl Pts',(0.408428948108533,1.,1.8224702267854));
#31264=CARTESIAN_POINT('Ctrl Pts',(0.410641256301674,-1.,1.83100408895216));
#31265=CARTESIAN_POINT('Ctrl Pts',(0.410641256301674,1.,1.83100408895216));
#31266=CARTESIAN_POINT('Ctrl Pts',(0.412633125322161,-1.,1.83808953475839));
#31267=CARTESIAN_POINT('Ctrl Pts',(0.412633125322161,1.,1.83808953475839));
#31268=CARTESIAN_POINT('Ctrl Pts',(0.41448743825434,-1.,1.8440575707371));
#31269=CARTESIAN_POINT('Ctrl Pts',(0.41448743825434,1.,1.8440575707371));
#31270=CARTESIAN_POINT('Ctrl Pts',(0.416300022038864,-1.,1.84929312929882));
#31271=CARTESIAN_POINT('Ctrl Pts',(0.416300022038864,1.,1.84929312929882));
#31272=CARTESIAN_POINT('Ctrl Pts',(0.418164129143534,-1.,1.85417632856234));
#31273=CARTESIAN_POINT('Ctrl Pts',(0.418164129143534,1.,1.85417632856234));
#31274=CARTESIAN_POINT('Ctrl Pts',(0.420157287975619,-1.,1.85903281096686));
#31275=CARTESIAN_POINT('Ctrl Pts',(0.420157287975619,1.,1.85903281096686));
#31276=CARTESIAN_POINT('Ctrl Pts',(0.422327307418275,-1.,1.86408083334028));
#31277=CARTESIAN_POINT('Ctrl Pts',(0.422327307418275,1.,1.86408083334028));
#31278=CARTESIAN_POINT('Ctrl Pts',(0.424678177291358,-1.,1.86937803944323));
#31279=CARTESIAN_POINT('Ctrl Pts',(0.424678177291358,1.,1.86937803944323));
#31280=CARTESIAN_POINT('Ctrl Pts',(0.427183828519102,-1.,1.87486989291484));
#31281=CARTESIAN_POINT('Ctrl Pts',(0.427183828519102,1.,1.87486989291484));
#31282=CARTESIAN_POINT('Ctrl Pts',(0.429803062482344,-1.,1.88044229001832));
#31283=CARTESIAN_POINT('Ctrl Pts',(0.429803062482344,1.,1.88044229001832));
#31284=CARTESIAN_POINT('Ctrl Pts',(0.432493038548748,-1.,1.88596913666793));
#31285=CARTESIAN_POINT('Ctrl Pts',(0.432493038548748,1.,1.88596913666793));
#31286=CARTESIAN_POINT('Ctrl Pts',(0.435225660963383,-1.,1.89136993975504));
#31287=CARTESIAN_POINT('Ctrl Pts',(0.435225660963383,1.,1.89136993975504));
#31288=CARTESIAN_POINT('Ctrl Pts',(0.437995003948244,-1.,1.89663648956466));
#31289=CARTESIAN_POINT('Ctrl Pts',(0.437995003948244,1.,1.89663648956466));
#31290=CARTESIAN_POINT('Ctrl Pts',(0.440807833704038,-1.,1.90180124389086));
#31291=CARTESIAN_POINT('Ctrl Pts',(0.440807833704038,1.,1.90180124389086));
#31292=CARTESIAN_POINT('Ctrl Pts',(0.44367755684915,-1.,1.90691756144898));
#31293=CARTESIAN_POINT('Ctrl Pts',(0.44367755684915,1.,1.90691756144898));
#31294=CARTESIAN_POINT('Ctrl Pts',(0.446617343485711,-1.,1.9120369998112));
#31295=CARTESIAN_POINT('Ctrl Pts',(0.446617343485711,1.,1.9120369998112));
#31296=CARTESIAN_POINT('Ctrl Pts',(0.449632260106662,-1.,1.91718342555755));
#31297=CARTESIAN_POINT('Ctrl Pts',(0.449632260106662,1.,1.91718342555755));
#31298=CARTESIAN_POINT('Ctrl Pts',(0.452719478359432,-1.,1.92235380648502));
#31299=CARTESIAN_POINT('Ctrl Pts',(0.452719478359432,1.,1.92235380648502));
#31300=CARTESIAN_POINT('Ctrl Pts',(0.45587200517437,-1.,1.92753067150476));
#31301=CARTESIAN_POINT('Ctrl Pts',(0.45587200517437,1.,1.92753067150476));
#31302=CARTESIAN_POINT('Ctrl Pts',(0.459081234547926,-1.,1.93269066517934));
#31303=CARTESIAN_POINT('Ctrl Pts',(0.459081234547926,1.,1.93269066517934));
#31304=CARTESIAN_POINT('Ctrl Pts',(0.462340031009056,-1.,1.93781486640821));
#31305=CARTESIAN_POINT('Ctrl Pts',(0.462340031009056,1.,1.93781486640821));
#31306=CARTESIAN_POINT('Ctrl Pts',(0.46564546202603,-1.,1.9428979419619));
#31307=CARTESIAN_POINT('Ctrl Pts',(0.46564546202603,1.,1.9428979419619));
#31308=CARTESIAN_POINT('Ctrl Pts',(0.468997482913135,-1.,1.94794381136514));
#31309=CARTESIAN_POINT('Ctrl Pts',(0.468997482913135,1.,1.94794381136514));
#31310=CARTESIAN_POINT('Ctrl Pts',(0.472397672264072,-1.,1.95296148278133));
#31311=CARTESIAN_POINT('Ctrl Pts',(0.472397672264072,1.,1.95296148278133));
#31312=CARTESIAN_POINT('Ctrl Pts',(0.475848034683176,-1.,1.95796111148177));
#31313=CARTESIAN_POINT('Ctrl Pts',(0.475848034683176,1.,1.95796111148177));
#31314=CARTESIAN_POINT('Ctrl Pts',(0.479349583074855,-1.,1.96294933055943));
#31315=CARTESIAN_POINT('Ctrl Pts',(0.479349583074855,1.,1.96294933055943));
#31316=CARTESIAN_POINT('Ctrl Pts',(0.48290166212069,-1.,1.96792703422362));
#31317=CARTESIAN_POINT('Ctrl Pts',(0.48290166212069,1.,1.96792703422362));
#31318=CARTESIAN_POINT('Ctrl Pts',(0.486502692907658,-1.,1.97289186263272));
#31319=CARTESIAN_POINT('Ctrl Pts',(0.486502692907658,1.,1.97289186263272));
#31320=CARTESIAN_POINT('Ctrl Pts',(0.490150627860952,-1.,1.97783973019229));
#31321=CARTESIAN_POINT('Ctrl Pts',(0.490150627860952,1.,1.97783973019229));
#31322=CARTESIAN_POINT('Ctrl Pts',(0.493843476541494,-1.,1.98276658761821));
#31323=CARTESIAN_POINT('Ctrl Pts',(0.493843476541494,1.,1.98276658761821));
#31324=CARTESIAN_POINT('Ctrl Pts',(0.497579909545574,-1.,1.98767044752932));
#31325=CARTESIAN_POINT('Ctrl Pts',(0.497579909545574,1.,1.98767044752932));
#31326=CARTESIAN_POINT('Ctrl Pts',(0.501359287727146,-1.,1.99255149126155));
#31327=CARTESIAN_POINT('Ctrl Pts',(0.501359287727146,1.,1.99255149126155));
#31328=CARTESIAN_POINT('Ctrl Pts',(0.505181361323026,-1.,1.99741107463572));
#31329=CARTESIAN_POINT('Ctrl Pts',(0.505181361323026,1.,1.99741107463572));
#31330=CARTESIAN_POINT('Ctrl Pts',(0.509046069886157,-1.,2.00225107134734));
#31331=CARTESIAN_POINT('Ctrl Pts',(0.509046069886157,1.,2.00225107134734));
#31332=CARTESIAN_POINT('Ctrl Pts',(0.512953306961792,-1.,2.00707309946949));
#31333=CARTESIAN_POINT('Ctrl Pts',(0.512953306961792,1.,2.00707309946949));
#31334=CARTESIAN_POINT('Ctrl Pts',(0.516902681728687,-1.,2.01187773939242));
#31335=CARTESIAN_POINT('Ctrl Pts',(0.516902681728687,1.,2.01187773939242));
#31336=CARTESIAN_POINT('Ctrl Pts',(0.52089359039937,-1.,2.01666477917286));
#31337=CARTESIAN_POINT('Ctrl Pts',(0.52089359039937,1.,2.01666477917286));
#31338=CARTESIAN_POINT('Ctrl Pts',(0.524925318333476,-1.,2.02143356304698));
#31339=CARTESIAN_POINT('Ctrl Pts',(0.524925318333476,1.,2.02143356304698));
#31340=CARTESIAN_POINT('Ctrl Pts',(0.528997127241914,-1.,2.0261832908329));
#31341=CARTESIAN_POINT('Ctrl Pts',(0.528997127241914,1.,2.0261832908329));
#31342=CARTESIAN_POINT('Ctrl Pts',(0.533108355132976,-1.,2.03091336214426));
#31343=CARTESIAN_POINT('Ctrl Pts',(0.533108355132976,1.,2.03091336214426));
#31344=CARTESIAN_POINT('Ctrl Pts',(0.537258489833262,-1.,2.03562362954037));
#31345=CARTESIAN_POINT('Ctrl Pts',(0.537258489833262,1.,2.03562362954037));
#31346=CARTESIAN_POINT('Ctrl Pts',(0.541447120615659,-1.,2.04031422690527));
#31347=CARTESIAN_POINT('Ctrl Pts',(0.541447120615659,1.,2.04031422690527));
#31348=CARTESIAN_POINT('Ctrl Pts',(0.54567390381743,-1.,2.04498544714588));
#31349=CARTESIAN_POINT('Ctrl Pts',(0.54567390381743,1.,2.04498544714588));
#31350=CARTESIAN_POINT('Ctrl Pts',(0.549938525150295,-1.,2.04963761077958));
#31351=CARTESIAN_POINT('Ctrl Pts',(0.549938525150295,1.,2.04963761077958));
#31352=CARTESIAN_POINT('Ctrl Pts',(0.554240657463906,-1.,2.05427091604413));
#31353=CARTESIAN_POINT('Ctrl Pts',(0.554240657463906,1.,2.05427091604413));
#31354=CARTESIAN_POINT('Ctrl Pts',(0.558579940185151,-1.,2.05888537756462));
#31355=CARTESIAN_POINT('Ctrl Pts',(0.558579940185151,1.,2.05888537756462));
#31356=CARTESIAN_POINT('Ctrl Pts',(0.562955993082261,-1.,2.06348090160589));
#31357=CARTESIAN_POINT('Ctrl Pts',(0.562955993082261,1.,2.06348090160589));
#31358=CARTESIAN_POINT('Ctrl Pts',(0.567368421181087,-1.,2.06805732997334));
#31359=CARTESIAN_POINT('Ctrl Pts',(0.567368421181087,1.,2.06805732997334));
#31360=CARTESIAN_POINT('Ctrl Pts',(0.571816823242602,-1.,2.07261449292824));
#31361=CARTESIAN_POINT('Ctrl Pts',(0.571816823242602,1.,2.07261449292824));
#31362=CARTESIAN_POINT('Ctrl Pts',(0.576300797416844,-1.,2.07715226767559));
#31363=CARTESIAN_POINT('Ctrl Pts',(0.576300797416844,1.,2.07715226767559));
#31364=CARTESIAN_POINT('Ctrl Pts',(0.580819952108063,-1.,2.08167059018418));
#31365=CARTESIAN_POINT('Ctrl Pts',(0.580819952108063,1.,2.08167059018418));
#31366=CARTESIAN_POINT('Ctrl Pts',(0.585373918991617,-1.,2.08616943727951));
#31367=CARTESIAN_POINT('Ctrl Pts',(0.585373918991617,1.,2.08616943727951));
#31368=CARTESIAN_POINT('Ctrl Pts',(0.589962365403406,-1.,2.09064881812129));
#31369=CARTESIAN_POINT('Ctrl Pts',(0.589962365403406,1.,2.09064881812129));
#31370=CARTESIAN_POINT('Ctrl Pts',(0.594585006052162,-1.,2.0951087622027));
#31371=CARTESIAN_POINT('Ctrl Pts',(0.594585006052162,1.,2.0951087622027));
#31372=CARTESIAN_POINT('Ctrl Pts',(0.599241616420533,-1.,2.0995493086477));
#31373=CARTESIAN_POINT('Ctrl Pts',(0.599241616420533,1.,2.0995493086477));
#31374=CARTESIAN_POINT('Ctrl Pts',(0.60393203073603,-1.,2.10397049886949));
#31375=CARTESIAN_POINT('Ctrl Pts',(0.60393203073603,1.,2.10397049886949));
#31376=CARTESIAN_POINT('Ctrl Pts',(0.607711315454876,-1.,2.1074919961518));
#31377=CARTESIAN_POINT('Ctrl Pts',(0.607711315454876,1.,2.1074919961518));
#31378=CARTESIAN_POINT('Ctrl Pts',(0.610560911689898,-1.,2.11012443807238));
#31379=CARTESIAN_POINT('Ctrl Pts',(0.610560911689898,1.,2.11012443807238));
#31380=CARTESIAN_POINT('Ctrl Pts',(0.6124673655618,-1.,2.11187554259986));
#31381=CARTESIAN_POINT('Ctrl Pts',(0.6124673655618,1.,2.11187554259986));
#31382=CARTESIAN_POINT('Ctrl Pts',(0.61342227326009,-1.,2.11275013067528));
#31383=CARTESIAN_POINT('Ctrl Pts',(0.61342227326009,1.,2.11275013067528));
#31384=CARTESIAN_POINT('',(0.383122945602004,1.,1.7075470150345));
#31385=CARTESIAN_POINT('Ctrl Pts',(0.383122945602004,1.,1.7075470150345));
#31386=CARTESIAN_POINT('Ctrl Pts',(0.384119047315541,1.,1.71231062891958));
#31387=CARTESIAN_POINT('Ctrl Pts',(0.38607079032701,1.,1.72162022246158));
#31388=CARTESIAN_POINT('Ctrl Pts',(0.388877023509191,1.,1.7349317097561));
#31389=CARTESIAN_POINT('Ctrl Pts',(0.392375812294307,1.,1.75137405313962));
#31390=CARTESIAN_POINT('Ctrl Pts',(0.39634619612042,1.,1.7697556004756));
#31391=CARTESIAN_POINT('Ctrl Pts',(0.39991940378308,1.,1.78598826347533));
#31392=CARTESIAN_POINT('Ctrl Pts',(0.403107976170441,1.,1.80012077176221));
#31393=CARTESIAN_POINT('Ctrl Pts',(0.405933518411838,1.,1.81223801813988));
#31394=CARTESIAN_POINT('Ctrl Pts',(0.408428948108533,1.,1.8224702267854));
#31395=CARTESIAN_POINT('Ctrl Pts',(0.410641256301674,1.,1.83100408895216));
#31396=CARTESIAN_POINT('Ctrl Pts',(0.412633125322161,1.,1.83808953475839));
#31397=CARTESIAN_POINT('Ctrl Pts',(0.41448743825434,1.,1.8440575707371));
#31398=CARTESIAN_POINT('Ctrl Pts',(0.416300022038864,1.,1.84929312929882));
#31399=CARTESIAN_POINT('Ctrl Pts',(0.418164129143534,1.,1.85417632856234));
#31400=CARTESIAN_POINT('Ctrl Pts',(0.420157287975619,1.,1.85903281096686));
#31401=CARTESIAN_POINT('Ctrl Pts',(0.422327307418275,1.,1.86408083334028));
#31402=CARTESIAN_POINT('Ctrl Pts',(0.424678177291358,1.,1.86937803944323));
#31403=CARTESIAN_POINT('Ctrl Pts',(0.427183828519102,1.,1.87486989291484));
#31404=CARTESIAN_POINT('Ctrl Pts',(0.429803062482344,1.,1.88044229001832));
#31405=CARTESIAN_POINT('Ctrl Pts',(0.432493038548748,1.,1.88596913666793));
#31406=CARTESIAN_POINT('Ctrl Pts',(0.435225660963383,1.,1.89136993975504));
#31407=CARTESIAN_POINT('Ctrl Pts',(0.437995003948244,1.,1.89663648956466));
#31408=CARTESIAN_POINT('Ctrl Pts',(0.440807833704038,1.,1.90180124389086));
#31409=CARTESIAN_POINT('Ctrl Pts',(0.44367755684915,1.,1.90691756144898));
#31410=CARTESIAN_POINT('Ctrl Pts',(0.446617343485711,1.,1.9120369998112));
#31411=CARTESIAN_POINT('Ctrl Pts',(0.449632260106662,1.,1.91718342555755));
#31412=CARTESIAN_POINT('Ctrl Pts',(0.452719478359432,1.,1.92235380648502));
#31413=CARTESIAN_POINT('Ctrl Pts',(0.45587200517437,1.,1.92753067150476));
#31414=CARTESIAN_POINT('Ctrl Pts',(0.459081234547926,1.,1.93269066517934));
#31415=CARTESIAN_POINT('Ctrl Pts',(0.462340031009056,1.,1.93781486640821));
#31416=CARTESIAN_POINT('Ctrl Pts',(0.46564546202603,1.,1.9428979419619));
#31417=CARTESIAN_POINT('Ctrl Pts',(0.468997482913135,1.,1.94794381136514));
#31418=CARTESIAN_POINT('Ctrl Pts',(0.472397672264072,1.,1.95296148278133));
#31419=CARTESIAN_POINT('Ctrl Pts',(0.475848034683176,1.,1.95796111148177));
#31420=CARTESIAN_POINT('Ctrl Pts',(0.479349583074855,1.,1.96294933055943));
#31421=CARTESIAN_POINT('Ctrl Pts',(0.48290166212069,1.,1.96792703422362));
#31422=CARTESIAN_POINT('Ctrl Pts',(0.486502692907658,1.,1.97289186263272));
#31423=CARTESIAN_POINT('Ctrl Pts',(0.490150627860952,1.,1.97783973019229));
#31424=CARTESIAN_POINT('Ctrl Pts',(0.493843476541494,1.,1.98276658761821));
#31425=CARTESIAN_POINT('Ctrl Pts',(0.497579909545574,1.,1.98767044752932));
#31426=CARTESIAN_POINT('Ctrl Pts',(0.501359287727146,1.,1.99255149126155));
#31427=CARTESIAN_POINT('Ctrl Pts',(0.505181361323026,1.,1.99741107463572));
#31428=CARTESIAN_POINT('Ctrl Pts',(0.509046069886157,1.,2.00225107134734));
#31429=CARTESIAN_POINT('Ctrl Pts',(0.512953306961792,1.,2.00707309946949));
#31430=CARTESIAN_POINT('Ctrl Pts',(0.516902681728687,1.,2.01187773939242));
#31431=CARTESIAN_POINT('Ctrl Pts',(0.52089359039937,1.,2.01666477917286));
#31432=CARTESIAN_POINT('Ctrl Pts',(0.524925318333476,1.,2.02143356304698));
#31433=CARTESIAN_POINT('Ctrl Pts',(0.528997127241914,1.,2.0261832908329));
#31434=CARTESIAN_POINT('Ctrl Pts',(0.533108355132976,1.,2.03091336214426));
#31435=CARTESIAN_POINT('Ctrl Pts',(0.537258489833262,1.,2.03562362954037));
#31436=CARTESIAN_POINT('Ctrl Pts',(0.541447120615659,1.,2.04031422690527));
#31437=CARTESIAN_POINT('Ctrl Pts',(0.54567390381743,1.,2.04498544714588));
#31438=CARTESIAN_POINT('Ctrl Pts',(0.549938525150295,1.,2.04963761077958));
#31439=CARTESIAN_POINT('Ctrl Pts',(0.554240657463906,1.,2.05427091604413));
#31440=CARTESIAN_POINT('Ctrl Pts',(0.558579940185151,1.,2.05888537756462));
#31441=CARTESIAN_POINT('Ctrl Pts',(0.562955993082261,1.,2.06348090160589));
#31442=CARTESIAN_POINT('Ctrl Pts',(0.567368421181087,1.,2.06805732997334));
#31443=CARTESIAN_POINT('Ctrl Pts',(0.571816823242602,1.,2.07261449292824));
#31444=CARTESIAN_POINT('Ctrl Pts',(0.576300797416844,1.,2.07715226767559));
#31445=CARTESIAN_POINT('Ctrl Pts',(0.580819952108063,1.,2.08167059018418));
#31446=CARTESIAN_POINT('Ctrl Pts',(0.585373918991617,1.,2.08616943727951));
#31447=CARTESIAN_POINT('Ctrl Pts',(0.589962365403406,1.,2.09064881812129));
#31448=CARTESIAN_POINT('Ctrl Pts',(0.594585006052162,1.,2.0951087622027));
#31449=CARTESIAN_POINT('Ctrl Pts',(0.599241616420533,1.,2.0995493086477));
#31450=CARTESIAN_POINT('Ctrl Pts',(0.60393203073603,1.,2.10397049886949));
#31451=CARTESIAN_POINT('Ctrl Pts',(0.607711315454876,1.,2.1074919961518));
#31452=CARTESIAN_POINT('Ctrl Pts',(0.610560911689898,1.,2.11012443807238));
#31453=CARTESIAN_POINT('Ctrl Pts',(0.6124673655618,1.,2.11187554259986));
#31454=CARTESIAN_POINT('Ctrl Pts',(0.61342227326009,1.,2.11275013067528));
#31455=CARTESIAN_POINT('',(0.383122945602003,0.,1.7075470150345));
#31456=CARTESIAN_POINT('Origin',(0.,0.,0.));
#31457=CARTESIAN_POINT('',(0.163289472382896,1.,1.74236521665491));
#31458=CARTESIAN_POINT('Origin',(0.,1.,0.));
#31459=CARTESIAN_POINT('',(0.163289472382896,0.,1.74236521665491));
#31460=CARTESIAN_POINT('Ctrl Pts',(0.0694764450219578,-1.,2.19890268624765));
#31461=CARTESIAN_POINT('Ctrl Pts',(0.0694764450219578,1.,2.19890268624765));
#31462=CARTESIAN_POINT('Ctrl Pts',(0.0701143536325487,-1.,2.19777582085423));
#31463=CARTESIAN_POINT('Ctrl Pts',(0.0701143536325487,1.,2.19777582085423));
#31464=CARTESIAN_POINT('Ctrl Pts',(0.0713863779526151,-1.,2.19552129484002));
#31465=CARTESIAN_POINT('Ctrl Pts',(0.0713863779526151,1.,2.19552129484002));
#31466=CARTESIAN_POINT('Ctrl Pts',(0.0732830357306722,-1.,2.19213712013662));
#31467=CARTESIAN_POINT('Ctrl Pts',(0.0732830357306722,1.,2.19213712013662));
#31468=CARTESIAN_POINT('Ctrl Pts',(0.0757891465836145,-1.,2.1876201139953));
#31469=CARTESIAN_POINT('Ctrl Pts',(0.0757891465836145,1.,2.1876201139953));
#31470=CARTESIAN_POINT('Ctrl Pts',(0.078883772768524,-1.,2.18196589448887));
#31471=CARTESIAN_POINT('Ctrl Pts',(0.078883772768524,1.,2.18196589448887));
#31472=CARTESIAN_POINT('Ctrl Pts',(0.0819402680872763,-1.,2.176303712113));
#31473=CARTESIAN_POINT('Ctrl Pts',(0.0819402680872763,1.,2.176303712113));
#31474=CARTESIAN_POINT('Ctrl Pts',(0.084958462083537,-1.,2.17063357870952));
#31475=CARTESIAN_POINT('Ctrl Pts',(0.084958462083537,1.,2.17063357870952));
#31476=CARTESIAN_POINT('Ctrl Pts',(0.087938129138692,-1.,2.16495552645014));
#31477=CARTESIAN_POINT('Ctrl Pts',(0.087938129138692,1.,2.16495552645014));
#31478=CARTESIAN_POINT('Ctrl Pts',(0.0908789888107263,-1.,2.15926961544516));
#31479=CARTESIAN_POINT('Ctrl Pts',(0.0908789888107263,1.,2.15926961544516));
#31480=CARTESIAN_POINT('Ctrl Pts',(0.0937807218867641,-1.,2.1535759397817));
#31481=CARTESIAN_POINT('Ctrl Pts',(0.0937807218867641,1.,2.1535759397817));
#31482=CARTESIAN_POINT('Ctrl Pts',(0.0966429852305456,-1.,2.14787463531795));
#31483=CARTESIAN_POINT('Ctrl Pts',(0.0966429852305456,1.,2.14787463531795));
#31484=CARTESIAN_POINT('Ctrl Pts',(0.0994654261990913,-1.,2.14216588396025));
#31485=CARTESIAN_POINT('Ctrl Pts',(0.0994654261990913,1.,2.14216588396025));
#31486=CARTESIAN_POINT('Ctrl Pts',(0.1022477005561,-1.,2.13644992667165));
#31487=CARTESIAN_POINT('Ctrl Pts',(0.1022477005561,1.,2.13644992667165));
#31488=CARTESIAN_POINT('Ctrl Pts',(0.104989479152739,-1.,2.13072704887293));
#31489=CARTESIAN_POINT('Ctrl Pts',(0.104989479152739,1.,2.13072704887293));
#31490=CARTESIAN_POINT('Ctrl Pts',(0.10769043523109,-1.,2.12499752307));
#31491=CARTESIAN_POINT('Ctrl Pts',(0.10769043523109,1.,2.12499752307));
#31492=CARTESIAN_POINT('Ctrl Pts',(0.110350236135025,-1.,2.11926155590865));
#31493=CARTESIAN_POINT('Ctrl Pts',(0.110350236135025,1.,2.11926155590865));
#31494=CARTESIAN_POINT('Ctrl Pts',(0.112968534419737,-1.,2.11351924490306));
#31495=CARTESIAN_POINT('Ctrl Pts',(0.112968534419737,1.,2.11351924490306));
#31496=CARTESIAN_POINT('Ctrl Pts',(0.115544957687926,-1.,2.10777050261309));
#31497=CARTESIAN_POINT('Ctrl Pts',(0.115544957687926,1.,2.10777050261309));
#31498=CARTESIAN_POINT('Ctrl Pts',(0.118079107988355,-1.,2.102015121329));
#31499=CARTESIAN_POINT('Ctrl Pts',(0.118079107988355,1.,2.102015121329));
#31500=CARTESIAN_POINT('Ctrl Pts',(0.120570567965122,-1.,2.0962529286773));
#31501=CARTESIAN_POINT('Ctrl Pts',(0.120570567965122,1.,2.0962529286773));
#31502=CARTESIAN_POINT('Ctrl Pts',(0.123018905621083,-1.,2.09048392424825));
#31503=CARTESIAN_POINT('Ctrl Pts',(0.123018905621083,1.,2.09048392424825));
#31504=CARTESIAN_POINT('Ctrl Pts',(0.125423679412061,-1.,2.08470840653643));
#31505=CARTESIAN_POINT('Ctrl Pts',(0.125423679412061,1.,2.08470840653643));
#31506=CARTESIAN_POINT('Ctrl Pts',(0.12778444527612,-1.,2.07892715110987));
#31507=CARTESIAN_POINT('Ctrl Pts',(0.12778444527612,1.,2.07892715110987));
#31508=CARTESIAN_POINT('Ctrl Pts',(0.130100748328403,-1.,2.07314114713063));
#31509=CARTESIAN_POINT('Ctrl Pts',(0.130100748328403,1.,2.07314114713063));
#31510=CARTESIAN_POINT('Ctrl Pts',(0.13237211154771,-1.,2.06735123910326));
#31511=CARTESIAN_POINT('Ctrl Pts',(0.13237211154771,1.,2.06735123910326));
#31512=CARTESIAN_POINT('Ctrl Pts',(0.134598026192106,-1.,2.06155781517842));
#31513=CARTESIAN_POINT('Ctrl Pts',(0.134598026192106,1.,2.06155781517842));
#31514=CARTESIAN_POINT('Ctrl Pts',(0.136777941218043,-1.,2.05576044414264));
#31515=CARTESIAN_POINT('Ctrl Pts',(0.136777941218043,1.,2.05576044414264));
#31516=CARTESIAN_POINT('Ctrl Pts',(0.138911255368966,-1.,2.04995762001328));
#31517=CARTESIAN_POINT('Ctrl Pts',(0.138911255368966,1.,2.04995762001328));
#31518=CARTESIAN_POINT('Ctrl Pts',(0.140997332152546,-1.,2.04414757947916));
#31519=CARTESIAN_POINT('Ctrl Pts',(0.140997332152546,1.,2.04414757947916));
#31520=CARTESIAN_POINT('Ctrl Pts',(0.143035515058208,-1.,2.03832911025912));
#31521=CARTESIAN_POINT('Ctrl Pts',(0.143035515058208,1.,2.03832911025912));
#31522=CARTESIAN_POINT('Ctrl Pts',(0.145025140186057,-1.,2.03250223739942));
#31523=CARTESIAN_POINT('Ctrl Pts',(0.145025140186057,1.,2.03250223739942));
#31524=CARTESIAN_POINT('Ctrl Pts',(0.146965557332583,-1.,2.02666926182017));
#31525=CARTESIAN_POINT('Ctrl Pts',(0.146965557332583,1.,2.02666926182017));
#31526=CARTESIAN_POINT('Ctrl Pts',(0.148856124775337,-1.,2.02083464969894));
#31527=CARTESIAN_POINT('Ctrl Pts',(0.148856124775337,1.,2.02083464969894));
#31528=CARTESIAN_POINT('Ctrl Pts',(0.150696157673078,-1.,2.01500291940238));
#31529=CARTESIAN_POINT('Ctrl Pts',(0.150696157673078,1.,2.01500291940238));
#31530=CARTESIAN_POINT('Ctrl Pts',(0.152484883621449,-1.,2.00917680318424));
#31531=CARTESIAN_POINT('Ctrl Pts',(0.152484883621449,1.,2.00917680318424));
#31532=CARTESIAN_POINT('Ctrl Pts',(0.154221403049722,-1.,2.00335565310543));
#31533=CARTESIAN_POINT('Ctrl Pts',(0.154221403049722,1.,2.00335565310543));
#31534=CARTESIAN_POINT('Ctrl Pts',(0.155904629548783,-1.,1.99753284771497));
#31535=CARTESIAN_POINT('Ctrl Pts',(0.155904629548783,1.,1.99753284771497));
#31536=CARTESIAN_POINT('Ctrl Pts',(0.157533331459227,-1.,1.99169810931908));
#31537=CARTESIAN_POINT('Ctrl Pts',(0.157533331459227,1.,1.99169810931908));
#31538=CARTESIAN_POINT('Ctrl Pts',(0.159106226437299,-1.,1.98584238283292));
#31539=CARTESIAN_POINT('Ctrl Pts',(0.159106226437299,1.,1.98584238283292));
#31540=CARTESIAN_POINT('Ctrl Pts',(0.160622060784611,-1.,1.97996195437559));
#31541=CARTESIAN_POINT('Ctrl Pts',(0.160622060784611,1.,1.97996195437559));
#31542=CARTESIAN_POINT('Ctrl Pts',(0.162079693556288,-1.,1.97406280235188));
#31543=CARTESIAN_POINT('Ctrl Pts',(0.162079693556288,1.,1.97406280235188));
#31544=CARTESIAN_POINT('Ctrl Pts',(0.163478185457734,-1.,1.96816512677967));
#31545=CARTESIAN_POINT('Ctrl Pts',(0.163478185457734,1.,1.96816512677967));
#31546=CARTESIAN_POINT('Ctrl Pts',(0.164816568920269,-1.,1.96229379940136));
#31547=CARTESIAN_POINT('Ctrl Pts',(0.164816568920269,1.,1.96229379940136));
#31548=CARTESIAN_POINT('Ctrl Pts',(0.166093592002812,-1.,1.9564675971873));
#31549=CARTESIAN_POINT('Ctrl Pts',(0.166093592002812,1.,1.9564675971873));
#31550=CARTESIAN_POINT('Ctrl Pts',(0.167307501784475,-1.,1.95069027794294));
#31551=CARTESIAN_POINT('Ctrl Pts',(0.167307501784475,1.,1.95069027794294));
#31552=CARTESIAN_POINT('Ctrl Pts',(0.168455741607556,-1.,1.94493757756931));
#31553=CARTESIAN_POINT('Ctrl Pts',(0.168455741607556,1.,1.94493757756931));
#31554=CARTESIAN_POINT('Ctrl Pts',(0.16953490481749,-1.,1.93915639211581));
#31555=CARTESIAN_POINT('Ctrl Pts',(0.16953490481749,1.,1.93915639211581));
#31556=CARTESIAN_POINT('Ctrl Pts',(0.170541253116201,-1.,1.93329183155539));
#31557=CARTESIAN_POINT('Ctrl Pts',(0.170541253116201,1.,1.93329183155539));
#31558=CARTESIAN_POINT('Ctrl Pts',(0.171471191532988,-1.,1.92731093582036));
#31559=CARTESIAN_POINT('Ctrl Pts',(0.171471191532988,1.,1.92731093582036));
#31560=CARTESIAN_POINT('Ctrl Pts',(0.172321621259513,-1.,1.9212233439798));
#31561=CARTESIAN_POINT('Ctrl Pts',(0.172321621259513,1.,1.9212233439798));
#31562=CARTESIAN_POINT('Ctrl Pts',(0.173090695383496,-1.,1.91511429159527));
#31563=CARTESIAN_POINT('Ctrl Pts',(0.173090695383496,1.,1.91511429159527));
#31564=CARTESIAN_POINT('Ctrl Pts',(0.173776635257816,-1.,1.90911693975267));
#31565=CARTESIAN_POINT('Ctrl Pts',(0.173776635257816,1.,1.90911693975267));
#31566=CARTESIAN_POINT('Ctrl Pts',(0.174375518661085,-1.,1.90335253862834));
#31567=CARTESIAN_POINT('Ctrl Pts',(0.174375518661085,1.,1.90335253862834));
#31568=CARTESIAN_POINT('Ctrl Pts',(0.174879405091263,-1.,1.89788101117132));
#31569=CARTESIAN_POINT('Ctrl Pts',(0.174879405091263,1.,1.89788101117132));
#31570=CARTESIAN_POINT('Ctrl Pts',(0.175274276190844,-1.,1.892646301985));
#31571=CARTESIAN_POINT('Ctrl Pts',(0.175274276190844,1.,1.892646301985));
#31572=CARTESIAN_POINT('Ctrl Pts',(0.175538155840648,-1.,1.88742606273259));
#31573=CARTESIAN_POINT('Ctrl Pts',(0.175538155840648,1.,1.88742606273259));
#31574=CARTESIAN_POINT('Ctrl Pts',(0.175644148889698,-1.,1.88188663145367));
#31575=CARTESIAN_POINT('Ctrl Pts',(0.175644148889698,1.,1.88188663145367));
#31576=CARTESIAN_POINT('Ctrl Pts',(0.175563480746485,-1.,1.87563767773588));
#31577=CARTESIAN_POINT('Ctrl Pts',(0.175563480746485,1.,1.87563767773588));
#31578=CARTESIAN_POINT('Ctrl Pts',(0.175268337590757,-1.,1.86828349694799));
#31579=CARTESIAN_POINT('Ctrl Pts',(0.175268337590757,1.,1.86828349694799));
#31580=CARTESIAN_POINT('Ctrl Pts',(0.17473525927603,-1.,1.85948367088837));
#31581=CARTESIAN_POINT('Ctrl Pts',(0.17473525927603,1.,1.85948367088837));
#31582=CARTESIAN_POINT('Ctrl Pts',(0.173946627587731,-1.,1.8489811319852));
#31583=CARTESIAN_POINT('Ctrl Pts',(0.173946627587731,1.,1.8489811319852));
#31584=CARTESIAN_POINT('Ctrl Pts',(0.1728894428919,-1.,1.83658380527692));
#31585=CARTESIAN_POINT('Ctrl Pts',(0.1728894428919,1.,1.83658380527692));
#31586=CARTESIAN_POINT('Ctrl Pts',(0.171554770204119,-1.,1.82215766811545));
#31587=CARTESIAN_POINT('Ctrl Pts',(0.171554770204119,1.,1.82215766811545));
#31588=CARTESIAN_POINT('Ctrl Pts',(0.169936923904608,-1.,1.80561530629706));
#31589=CARTESIAN_POINT('Ctrl Pts',(0.169936923904608,1.,1.80561530629706));
#31590=CARTESIAN_POINT('Ctrl Pts',(0.168032772805197,-1.,1.7869064998507));
#31591=CARTESIAN_POINT('Ctrl Pts',(0.168032772805197,1.,1.7869064998507));
#31592=CARTESIAN_POINT('Ctrl Pts',(0.1662793551464,-1.,1.77018771684844));
#31593=CARTESIAN_POINT('Ctrl Pts',(0.1662793551464,1.,1.77018771684844));
#31594=CARTESIAN_POINT('Ctrl Pts',(0.164834765707158,-1.,1.75666056638427));
#31595=CARTESIAN_POINT('Ctrl Pts',(0.164834765707158,1.,1.75666056638427));
#31596=CARTESIAN_POINT('Ctrl Pts',(0.163814161002002,-1.,1.7472034950333));
#31597=CARTESIAN_POINT('Ctrl Pts',(0.163814161002002,1.,1.7472034950333));
#31598=CARTESIAN_POINT('Ctrl Pts',(0.163289472382896,-1.,1.74236521665491));
#31599=CARTESIAN_POINT('Ctrl Pts',(0.163289472382896,1.,1.74236521665491));
#31600=CARTESIAN_POINT('',(0.0694764450219578,1.,2.19890268624765));
#31601=CARTESIAN_POINT('Ctrl Pts',(0.0694764450219578,1.,2.19890268624765));
#31602=CARTESIAN_POINT('Ctrl Pts',(0.0701143536325487,1.,2.19777582085423));
#31603=CARTESIAN_POINT('Ctrl Pts',(0.0713863779526151,1.,2.19552129484002));
#31604=CARTESIAN_POINT('Ctrl Pts',(0.0732830357306722,1.,2.19213712013662));
#31605=CARTESIAN_POINT('Ctrl Pts',(0.0757891465836145,1.,2.1876201139953));
#31606=CARTESIAN_POINT('Ctrl Pts',(0.078883772768524,1.,2.18196589448887));
#31607=CARTESIAN_POINT('Ctrl Pts',(0.0819402680872763,1.,2.176303712113));
#31608=CARTESIAN_POINT('Ctrl Pts',(0.084958462083537,1.,2.17063357870952));
#31609=CARTESIAN_POINT('Ctrl Pts',(0.087938129138692,1.,2.16495552645014));
#31610=CARTESIAN_POINT('Ctrl Pts',(0.0908789888107263,1.,2.15926961544516));
#31611=CARTESIAN_POINT('Ctrl Pts',(0.0937807218867641,1.,2.1535759397817));
#31612=CARTESIAN_POINT('Ctrl Pts',(0.0966429852305456,1.,2.14787463531795));
#31613=CARTESIAN_POINT('Ctrl Pts',(0.0994654261990913,1.,2.14216588396025));
#31614=CARTESIAN_POINT('Ctrl Pts',(0.1022477005561,1.,2.13644992667165));
#31615=CARTESIAN_POINT('Ctrl Pts',(0.104989479152739,1.,2.13072704887293));
#31616=CARTESIAN_POINT('Ctrl Pts',(0.10769043523109,1.,2.12499752307));
#31617=CARTESIAN_POINT('Ctrl Pts',(0.110350236135025,1.,2.11926155590865));
#31618=CARTESIAN_POINT('Ctrl Pts',(0.112968534419737,1.,2.11351924490306));
#31619=CARTESIAN_POINT('Ctrl Pts',(0.115544957687926,1.,2.10777050261309));
#31620=CARTESIAN_POINT('Ctrl Pts',(0.118079107988355,1.,2.102015121329));
#31621=CARTESIAN_POINT('Ctrl Pts',(0.120570567965122,1.,2.0962529286773));
#31622=CARTESIAN_POINT('Ctrl Pts',(0.123018905621083,1.,2.09048392424825));
#31623=CARTESIAN_POINT('Ctrl Pts',(0.125423679412061,1.,2.08470840653643));
#31624=CARTESIAN_POINT('Ctrl Pts',(0.12778444527612,1.,2.07892715110987));
#31625=CARTESIAN_POINT('Ctrl Pts',(0.130100748328403,1.,2.07314114713063));
#31626=CARTESIAN_POINT('Ctrl Pts',(0.13237211154771,1.,2.06735123910326));
#31627=CARTESIAN_POINT('Ctrl Pts',(0.134598026192106,1.,2.06155781517842));
#31628=CARTESIAN_POINT('Ctrl Pts',(0.136777941218043,1.,2.05576044414264));
#31629=CARTESIAN_POINT('Ctrl Pts',(0.138911255368966,1.,2.04995762001328));
#31630=CARTESIAN_POINT('Ctrl Pts',(0.140997332152546,1.,2.04414757947916));
#31631=CARTESIAN_POINT('Ctrl Pts',(0.143035515058208,1.,2.03832911025912));
#31632=CARTESIAN_POINT('Ctrl Pts',(0.145025140186057,1.,2.03250223739942));
#31633=CARTESIAN_POINT('Ctrl Pts',(0.146965557332583,1.,2.02666926182017));
#31634=CARTESIAN_POINT('Ctrl Pts',(0.148856124775337,1.,2.02083464969894));
#31635=CARTESIAN_POINT('Ctrl Pts',(0.150696157673078,1.,2.01500291940238));
#31636=CARTESIAN_POINT('Ctrl Pts',(0.152484883621449,1.,2.00917680318424));
#31637=CARTESIAN_POINT('Ctrl Pts',(0.154221403049722,1.,2.00335565310543));
#31638=CARTESIAN_POINT('Ctrl Pts',(0.155904629548783,1.,1.99753284771497));
#31639=CARTESIAN_POINT('Ctrl Pts',(0.157533331459227,1.,1.99169810931908));
#31640=CARTESIAN_POINT('Ctrl Pts',(0.159106226437299,1.,1.98584238283292));
#31641=CARTESIAN_POINT('Ctrl Pts',(0.160622060784611,1.,1.97996195437559));
#31642=CARTESIAN_POINT('Ctrl Pts',(0.162079693556288,1.,1.97406280235188));
#31643=CARTESIAN_POINT('Ctrl Pts',(0.163478185457734,1.,1.96816512677967));
#31644=CARTESIAN_POINT('Ctrl Pts',(0.164816568920269,1.,1.96229379940136));
#31645=CARTESIAN_POINT('Ctrl Pts',(0.166093592002812,1.,1.9564675971873));
#31646=CARTESIAN_POINT('Ctrl Pts',(0.167307501784475,1.,1.95069027794294));
#31647=CARTESIAN_POINT('Ctrl Pts',(0.168455741607556,1.,1.94493757756931));
#31648=CARTESIAN_POINT('Ctrl Pts',(0.16953490481749,1.,1.93915639211581));
#31649=CARTESIAN_POINT('Ctrl Pts',(0.170541253116201,1.,1.93329183155539));
#31650=CARTESIAN_POINT('Ctrl Pts',(0.171471191532988,1.,1.92731093582036));
#31651=CARTESIAN_POINT('Ctrl Pts',(0.172321621259513,1.,1.9212233439798));
#31652=CARTESIAN_POINT('Ctrl Pts',(0.173090695383496,1.,1.91511429159527));
#31653=CARTESIAN_POINT('Ctrl Pts',(0.173776635257816,1.,1.90911693975267));
#31654=CARTESIAN_POINT('Ctrl Pts',(0.174375518661085,1.,1.90335253862834));
#31655=CARTESIAN_POINT('Ctrl Pts',(0.174879405091263,1.,1.89788101117132));
#31656=CARTESIAN_POINT('Ctrl Pts',(0.175274276190844,1.,1.892646301985));
#31657=CARTESIAN_POINT('Ctrl Pts',(0.175538155840648,1.,1.88742606273259));
#31658=CARTESIAN_POINT('Ctrl Pts',(0.175644148889698,1.,1.88188663145367));
#31659=CARTESIAN_POINT('Ctrl Pts',(0.175563480746485,1.,1.87563767773588));
#31660=CARTESIAN_POINT('Ctrl Pts',(0.175268337590757,1.,1.86828349694799));
#31661=CARTESIAN_POINT('Ctrl Pts',(0.17473525927603,1.,1.85948367088837));
#31662=CARTESIAN_POINT('Ctrl Pts',(0.173946627587731,1.,1.8489811319852));
#31663=CARTESIAN_POINT('Ctrl Pts',(0.1728894428919,1.,1.83658380527692));
#31664=CARTESIAN_POINT('Ctrl Pts',(0.171554770204119,1.,1.82215766811545));
#31665=CARTESIAN_POINT('Ctrl Pts',(0.169936923904608,1.,1.80561530629706));
#31666=CARTESIAN_POINT('Ctrl Pts',(0.168032772805197,1.,1.7869064998507));
#31667=CARTESIAN_POINT('Ctrl Pts',(0.1662793551464,1.,1.77018771684844));
#31668=CARTESIAN_POINT('Ctrl Pts',(0.164834765707158,1.,1.75666056638427));
#31669=CARTESIAN_POINT('Ctrl Pts',(0.163814161002002,1.,1.7472034950333));
#31670=CARTESIAN_POINT('Ctrl Pts',(0.163289472382896,1.,1.74236521665491));
#31671=CARTESIAN_POINT('',(0.0694764450219578,0.,2.19890268624765));
#31672=CARTESIAN_POINT('Origin',(-0.0694764450219586,0.,2.19890268624765));
#31673=CARTESIAN_POINT('',(-0.0694764450219586,1.,2.19890268624765));
#31674=CARTESIAN_POINT('',(0.0694764450219578,1.,2.19890268624765));
#31675=CARTESIAN_POINT('',(-0.0694764450219586,0.,2.19890268624765));
#31676=CARTESIAN_POINT('Ctrl Pts',(-0.163289472382896,-1.,1.74236521665491));
#31677=CARTESIAN_POINT('Ctrl Pts',(-0.163289472382896,1.,1.74236521665491));
#31678=CARTESIAN_POINT('Ctrl Pts',(-0.163814161002474,-1.,1.74720349503904));
#31679=CARTESIAN_POINT('Ctrl Pts',(-0.163814161002474,1.,1.74720349503904));
#31680=CARTESIAN_POINT('Ctrl Pts',(-0.164834765708484,-1.,1.75666056640041));
#31681=CARTESIAN_POINT('Ctrl Pts',(-0.164834765708484,1.,1.75666056640041));
#31682=CARTESIAN_POINT('Ctrl Pts',(-0.166279355148738,-1.,1.77018771687692));
#31683=CARTESIAN_POINT('Ctrl Pts',(-0.166279355148738,1.,1.77018771687692));
#31684=CARTESIAN_POINT('Ctrl Pts',(-0.16803277280837,-1.,1.78690649988931));
#31685=CARTESIAN_POINT('Ctrl Pts',(-0.16803277280837,1.,1.78690649988931));
#31686=CARTESIAN_POINT('Ctrl Pts',(-0.169936923908078,-1.,1.80561530633924));
#31687=CARTESIAN_POINT('Ctrl Pts',(-0.169936923908078,1.,1.80561530633924));
#31688=CARTESIAN_POINT('Ctrl Pts',(-0.171554770207306,-1.,1.82215766815414));
#31689=CARTESIAN_POINT('Ctrl Pts',(-0.171554770207306,1.,1.82215766815414));
#31690=CARTESIAN_POINT('Ctrl Pts',(-0.17288944289442,-1.,1.83658380530747));
#31691=CARTESIAN_POINT('Ctrl Pts',(-0.17288944289442,1.,1.83658380530747));
#31692=CARTESIAN_POINT('Ctrl Pts',(-0.173946627589401,-1.,1.84898113200543));
#31693=CARTESIAN_POINT('Ctrl Pts',(-0.173946627589401,1.,1.84898113200543));
#31694=CARTESIAN_POINT('Ctrl Pts',(-0.174735259276856,-1.,1.85948367089838));
#31695=CARTESIAN_POINT('Ctrl Pts',(-0.174735259276856,1.,1.85948367089838));
#31696=CARTESIAN_POINT('Ctrl Pts',(-0.175268337590901,-1.,1.86828349694972));
#31697=CARTESIAN_POINT('Ctrl Pts',(-0.175268337590901,1.,1.86828349694972));
#31698=CARTESIAN_POINT('Ctrl Pts',(-0.175563480746206,-1.,1.87563767773249));
#31699=CARTESIAN_POINT('Ctrl Pts',(-0.175563480746206,1.,1.87563767773249));
#31700=CARTESIAN_POINT('Ctrl Pts',(-0.175644148889271,-1.,1.88188663144846));
#31701=CARTESIAN_POINT('Ctrl Pts',(-0.175644148889271,1.,1.88188663144846));
#31702=CARTESIAN_POINT('Ctrl Pts',(-0.175538155840286,-1.,1.88742606272818));
#31703=CARTESIAN_POINT('Ctrl Pts',(-0.175538155840286,1.,1.88742606272818));
#31704=CARTESIAN_POINT('Ctrl Pts',(-0.175274276190664,-1.,1.89264630198279));
#31705=CARTESIAN_POINT('Ctrl Pts',(-0.175274276190664,1.,1.89264630198279));
#31706=CARTESIAN_POINT('Ctrl Pts',(-0.174879405091277,-1.,1.89788101117148));
#31707=CARTESIAN_POINT('Ctrl Pts',(-0.174879405091277,1.,1.89788101117148));
#31708=CARTESIAN_POINT('Ctrl Pts',(-0.174375518661222,-1.,1.90335253863003));
#31709=CARTESIAN_POINT('Ctrl Pts',(-0.174375518661222,1.,1.90335253863003));
#31710=CARTESIAN_POINT('Ctrl Pts',(-0.173776635257984,-1.,1.90911693975475));
#31711=CARTESIAN_POINT('Ctrl Pts',(-0.173776635257984,1.,1.90911693975475));
#31712=CARTESIAN_POINT('Ctrl Pts',(-0.173090695383619,-1.,1.91511429159681));
#31713=CARTESIAN_POINT('Ctrl Pts',(-0.173090695383619,1.,1.91511429159681));
#31714=CARTESIAN_POINT('Ctrl Pts',(-0.172321621259557,-1.,1.92122334398034));
#31715=CARTESIAN_POINT('Ctrl Pts',(-0.172321621259557,1.,1.92122334398034));
#31716=CARTESIAN_POINT('Ctrl Pts',(-0.17147119153296,-1.,1.92731093582));
#31717=CARTESIAN_POINT('Ctrl Pts',(-0.17147119153296,1.,1.92731093582));
#31718=CARTESIAN_POINT('Ctrl Pts',(-0.170541253116136,-1.,1.93329183155455));
#31719=CARTESIAN_POINT('Ctrl Pts',(-0.170541253116136,1.,1.93329183155455));
#31720=CARTESIAN_POINT('Ctrl Pts',(-0.169534904817425,-1.,1.93915639211497));
#31721=CARTESIAN_POINT('Ctrl Pts',(-0.169534904817425,1.,1.93915639211497));
#31722=CARTESIAN_POINT('Ctrl Pts',(-0.168455741607516,-1.,1.94493757756879));
#31723=CARTESIAN_POINT('Ctrl Pts',(-0.168455741607516,1.,1.94493757756879));
#31724=CARTESIAN_POINT('Ctrl Pts',(-0.167307501784469,-1.,1.95069027794286));
#31725=CARTESIAN_POINT('Ctrl Pts',(-0.167307501784469,1.,1.95069027794286));
#31726=CARTESIAN_POINT('Ctrl Pts',(-0.166093592002833,-1.,1.95646759718755));
#31727=CARTESIAN_POINT('Ctrl Pts',(-0.166093592002833,1.,1.95646759718755));
#31728=CARTESIAN_POINT('Ctrl Pts',(-0.1648165689203,-1.,1.96229379940174));
#31729=CARTESIAN_POINT('Ctrl Pts',(-0.1648165689203,1.,1.96229379940174));
#31730=CARTESIAN_POINT('Ctrl Pts',(-0.16347818545776,-1.,1.96816512678));
#31731=CARTESIAN_POINT('Ctrl Pts',(-0.16347818545776,1.,1.96816512678));
#31732=CARTESIAN_POINT('Ctrl Pts',(-0.162079693556302,-1.,1.97406280235204));
#31733=CARTESIAN_POINT('Ctrl Pts',(-0.162079693556302,1.,1.97406280235204));
#31734=CARTESIAN_POINT('Ctrl Pts',(-0.16062206078461,-1.,1.97996195437557));
#31735=CARTESIAN_POINT('Ctrl Pts',(-0.16062206078461,1.,1.97996195437557));
#31736=CARTESIAN_POINT('Ctrl Pts',(-0.159106226437289,-1.,1.98584238283279));
#31737=CARTESIAN_POINT('Ctrl Pts',(-0.159106226437289,1.,1.98584238283279));
#31738=CARTESIAN_POINT('Ctrl Pts',(-0.157533331459215,-1.,1.99169810931893));
#31739=CARTESIAN_POINT('Ctrl Pts',(-0.157533331459215,1.,1.99169810931893));
#31740=CARTESIAN_POINT('Ctrl Pts',(-0.155904629548775,-1.,1.99753284771487));
#31741=CARTESIAN_POINT('Ctrl Pts',(-0.155904629548775,1.,1.99753284771487));
#31742=CARTESIAN_POINT('Ctrl Pts',(-0.154221403049719,-1.,2.00335565310539));
#31743=CARTESIAN_POINT('Ctrl Pts',(-0.154221403049719,1.,2.00335565310539));
#31744=CARTESIAN_POINT('Ctrl Pts',(-0.152484883621452,-1.,2.00917680318426));
#31745=CARTESIAN_POINT('Ctrl Pts',(-0.152484883621452,1.,2.00917680318426));
#31746=CARTESIAN_POINT('Ctrl Pts',(-0.150696157673084,-1.,2.01500291940243));
#31747=CARTESIAN_POINT('Ctrl Pts',(-0.150696157673084,1.,2.01500291940243));
#31748=CARTESIAN_POINT('Ctrl Pts',(-0.148856124775343,-1.,2.02083464969897));
#31749=CARTESIAN_POINT('Ctrl Pts',(-0.148856124775343,1.,2.02083464969897));
#31750=CARTESIAN_POINT('Ctrl Pts',(-0.146965557332586,-1.,2.02666926182017));
#31751=CARTESIAN_POINT('Ctrl Pts',(-0.146965557332586,1.,2.02666926182017));
#31752=CARTESIAN_POINT('Ctrl Pts',(-0.145025140186058,-1.,2.03250223739941));
#31753=CARTESIAN_POINT('Ctrl Pts',(-0.145025140186058,1.,2.03250223739941));
#31754=CARTESIAN_POINT('Ctrl Pts',(-0.143035515058208,-1.,2.03832911025913));
#31755=CARTESIAN_POINT('Ctrl Pts',(-0.143035515058208,1.,2.03832911025913));
#31756=CARTESIAN_POINT('Ctrl Pts',(-0.140997332152546,-1.,2.04414757947919));
#31757=CARTESIAN_POINT('Ctrl Pts',(-0.140997332152546,1.,2.04414757947919));
#31758=CARTESIAN_POINT('Ctrl Pts',(-0.138911255368966,-1.,2.04995762001333));
#31759=CARTESIAN_POINT('Ctrl Pts',(-0.138911255368966,1.,2.04995762001333));
#31760=CARTESIAN_POINT('Ctrl Pts',(-0.136777941218044,-1.,2.0557604441427));
#31761=CARTESIAN_POINT('Ctrl Pts',(-0.136777941218044,1.,2.0557604441427));
#31762=CARTESIAN_POINT('Ctrl Pts',(-0.134598026192107,-1.,2.06155781517844));
#31763=CARTESIAN_POINT('Ctrl Pts',(-0.134598026192107,1.,2.06155781517844));
#31764=CARTESIAN_POINT('Ctrl Pts',(-0.13237211154771,-1.,2.06735123910319));
#31765=CARTESIAN_POINT('Ctrl Pts',(-0.13237211154771,1.,2.06735123910319));
#31766=CARTESIAN_POINT('Ctrl Pts',(-0.130100748328401,-1.,2.07314114713047));
#31767=CARTESIAN_POINT('Ctrl Pts',(-0.130100748328401,1.,2.07314114713047));
#31768=CARTESIAN_POINT('Ctrl Pts',(-0.127784445276116,-1.,2.07892715110967));
#31769=CARTESIAN_POINT('Ctrl Pts',(-0.127784445276116,1.,2.07892715110967));
#31770=CARTESIAN_POINT('Ctrl Pts',(-0.125423679412058,-1.,2.08470840653628));
#31771=CARTESIAN_POINT('Ctrl Pts',(-0.125423679412058,1.,2.08470840653628));
#31772=CARTESIAN_POINT('Ctrl Pts',(-0.123018905621083,-1.,2.09048392424826));
#31773=CARTESIAN_POINT('Ctrl Pts',(-0.123018905621083,1.,2.09048392424826));
#31774=CARTESIAN_POINT('Ctrl Pts',(-0.120570567965129,-1.,2.09625292867756));
#31775=CARTESIAN_POINT('Ctrl Pts',(-0.120570567965129,1.,2.09625292867756));
#31776=CARTESIAN_POINT('Ctrl Pts',(-0.118079107988368,-1.,2.10201512132945));
#31777=CARTESIAN_POINT('Ctrl Pts',(-0.118079107988368,1.,2.10201512132945));
#31778=CARTESIAN_POINT('Ctrl Pts',(-0.115544957687941,-1.,2.10777050261359));
#31779=CARTESIAN_POINT('Ctrl Pts',(-0.115544957687941,1.,2.10777050261359));
#31780=CARTESIAN_POINT('Ctrl Pts',(-0.112968534419746,-1.,2.11351924490335));
#31781=CARTESIAN_POINT('Ctrl Pts',(-0.112968534419746,1.,2.11351924490335));
#31782=CARTESIAN_POINT('Ctrl Pts',(-0.11035023613502,-1.,2.11926155590849));
#31783=CARTESIAN_POINT('Ctrl Pts',(-0.11035023613502,1.,2.11926155590849));
#31784=CARTESIAN_POINT('Ctrl Pts',(-0.107690435231068,-1.,2.12499752306927));
#31785=CARTESIAN_POINT('Ctrl Pts',(-0.107690435231068,1.,2.12499752306927));
#31786=CARTESIAN_POINT('Ctrl Pts',(-0.104989479152703,-1.,2.1307270488718));
#31787=CARTESIAN_POINT('Ctrl Pts',(-0.104989479152703,1.,2.1307270488718));
#31788=CARTESIAN_POINT('Ctrl Pts',(-0.102247700556064,-1.,2.13644992667052));
#31789=CARTESIAN_POINT('Ctrl Pts',(-0.102247700556064,1.,2.13644992667052));
#31790=CARTESIAN_POINT('Ctrl Pts',(-0.0994654261990745,-1.,2.14216588395974));
#31791=CARTESIAN_POINT('Ctrl Pts',(-0.0994654261990745,1.,2.14216588395974));
#31792=CARTESIAN_POINT('Ctrl Pts',(-0.0966429852305691,-1.,2.14787463531864));
#31793=CARTESIAN_POINT('Ctrl Pts',(-0.0966429852305691,1.,2.14787463531864));
#31794=CARTESIAN_POINT('Ctrl Pts',(-0.0937807218868348,-1.,2.15357593978377));
#31795=CARTESIAN_POINT('Ctrl Pts',(-0.0937807218868348,1.,2.15357593978377));
#31796=CARTESIAN_POINT('Ctrl Pts',(-0.0908789888108269,-1.,2.15926961544808));
#31797=CARTESIAN_POINT('Ctrl Pts',(-0.0908789888108269,1.,2.15926961544808));
#31798=CARTESIAN_POINT('Ctrl Pts',(-0.0879381291387825,-1.,2.16495552645275));
#31799=CARTESIAN_POINT('Ctrl Pts',(-0.0879381291387825,1.,2.16495552645275));
#31800=CARTESIAN_POINT('Ctrl Pts',(-0.0849584620835646,-1.,2.17063357871031));
#31801=CARTESIAN_POINT('Ctrl Pts',(-0.0849584620835646,1.,2.17063357871031));
#31802=CARTESIAN_POINT('Ctrl Pts',(-0.0819402680871942,-1.,2.1763037121106));
#31803=CARTESIAN_POINT('Ctrl Pts',(-0.0819402680871942,1.,2.1763037121106));
#31804=CARTESIAN_POINT('Ctrl Pts',(-0.078883772768323,-1.,2.18196589448304));
#31805=CARTESIAN_POINT('Ctrl Pts',(-0.078883772768323,1.,2.18196589448304));
#31806=CARTESIAN_POINT('Ctrl Pts',(-0.0757891465833414,-1.,2.1876201139874));
#31807=CARTESIAN_POINT('Ctrl Pts',(-0.0757891465833414,1.,2.1876201139874));
#31808=CARTESIAN_POINT('Ctrl Pts',(-0.0732830357304279,-1.,2.19213712012956));
#31809=CARTESIAN_POINT('Ctrl Pts',(-0.0732830357304279,1.,2.19213712012956));
#31810=CARTESIAN_POINT('Ctrl Pts',(-0.071386377952463,-1.,2.19552129483562));
#31811=CARTESIAN_POINT('Ctrl Pts',(-0.071386377952463,1.,2.19552129483562));
#31812=CARTESIAN_POINT('Ctrl Pts',(-0.0701143536324929,-1.,2.19777582085261));
#31813=CARTESIAN_POINT('Ctrl Pts',(-0.0701143536324929,1.,2.19777582085261));
#31814=CARTESIAN_POINT('Ctrl Pts',(-0.0694764450219586,-1.,2.19890268624765));
#31815=CARTESIAN_POINT('Ctrl Pts',(-0.0694764450219586,1.,2.19890268624765));
#31816=CARTESIAN_POINT('',(-0.163289472382896,1.,1.74236521665491));
#31817=CARTESIAN_POINT('Ctrl Pts',(-0.163289472382896,1.,1.74236521665491));
#31818=CARTESIAN_POINT('Ctrl Pts',(-0.163814161002474,1.,1.74720349503904));
#31819=CARTESIAN_POINT('Ctrl Pts',(-0.164834765708484,1.,1.75666056640041));
#31820=CARTESIAN_POINT('Ctrl Pts',(-0.166279355148738,1.,1.77018771687692));
#31821=CARTESIAN_POINT('Ctrl Pts',(-0.16803277280837,1.,1.78690649988931));
#31822=CARTESIAN_POINT('Ctrl Pts',(-0.169936923908078,1.,1.80561530633924));
#31823=CARTESIAN_POINT('Ctrl Pts',(-0.171554770207306,1.,1.82215766815414));
#31824=CARTESIAN_POINT('Ctrl Pts',(-0.17288944289442,1.,1.83658380530747));
#31825=CARTESIAN_POINT('Ctrl Pts',(-0.173946627589401,1.,1.84898113200543));
#31826=CARTESIAN_POINT('Ctrl Pts',(-0.174735259276856,1.,1.85948367089838));
#31827=CARTESIAN_POINT('Ctrl Pts',(-0.175268337590901,1.,1.86828349694972));
#31828=CARTESIAN_POINT('Ctrl Pts',(-0.175563480746206,1.,1.87563767773249));
#31829=CARTESIAN_POINT('Ctrl Pts',(-0.175644148889271,1.,1.88188663144846));
#31830=CARTESIAN_POINT('Ctrl Pts',(-0.175538155840286,1.,1.88742606272818));
#31831=CARTESIAN_POINT('Ctrl Pts',(-0.175274276190664,1.,1.89264630198279));
#31832=CARTESIAN_POINT('Ctrl Pts',(-0.174879405091277,1.,1.89788101117148));
#31833=CARTESIAN_POINT('Ctrl Pts',(-0.174375518661222,1.,1.90335253863003));
#31834=CARTESIAN_POINT('Ctrl Pts',(-0.173776635257984,1.,1.90911693975475));
#31835=CARTESIAN_POINT('Ctrl Pts',(-0.173090695383619,1.,1.91511429159681));
#31836=CARTESIAN_POINT('Ctrl Pts',(-0.172321621259557,1.,1.92122334398034));
#31837=CARTESIAN_POINT('Ctrl Pts',(-0.17147119153296,1.,1.92731093582));
#31838=CARTESIAN_POINT('Ctrl Pts',(-0.170541253116136,1.,1.93329183155455));
#31839=CARTESIAN_POINT('Ctrl Pts',(-0.169534904817425,1.,1.93915639211497));
#31840=CARTESIAN_POINT('Ctrl Pts',(-0.168455741607516,1.,1.94493757756879));
#31841=CARTESIAN_POINT('Ctrl Pts',(-0.167307501784469,1.,1.95069027794286));
#31842=CARTESIAN_POINT('Ctrl Pts',(-0.166093592002833,1.,1.95646759718755));
#31843=CARTESIAN_POINT('Ctrl Pts',(-0.1648165689203,1.,1.96229379940174));
#31844=CARTESIAN_POINT('Ctrl Pts',(-0.16347818545776,1.,1.96816512678));
#31845=CARTESIAN_POINT('Ctrl Pts',(-0.162079693556302,1.,1.97406280235204));
#31846=CARTESIAN_POINT('Ctrl Pts',(-0.16062206078461,1.,1.97996195437557));
#31847=CARTESIAN_POINT('Ctrl Pts',(-0.159106226437289,1.,1.98584238283279));
#31848=CARTESIAN_POINT('Ctrl Pts',(-0.157533331459215,1.,1.99169810931893));
#31849=CARTESIAN_POINT('Ctrl Pts',(-0.155904629548775,1.,1.99753284771487));
#31850=CARTESIAN_POINT('Ctrl Pts',(-0.154221403049719,1.,2.00335565310539));
#31851=CARTESIAN_POINT('Ctrl Pts',(-0.152484883621452,1.,2.00917680318426));
#31852=CARTESIAN_POINT('Ctrl Pts',(-0.150696157673084,1.,2.01500291940243));
#31853=CARTESIAN_POINT('Ctrl Pts',(-0.148856124775343,1.,2.02083464969897));
#31854=CARTESIAN_POINT('Ctrl Pts',(-0.146965557332586,1.,2.02666926182017));
#31855=CARTESIAN_POINT('Ctrl Pts',(-0.145025140186058,1.,2.03250223739941));
#31856=CARTESIAN_POINT('Ctrl Pts',(-0.143035515058208,1.,2.03832911025913));
#31857=CARTESIAN_POINT('Ctrl Pts',(-0.140997332152546,1.,2.04414757947919));
#31858=CARTESIAN_POINT('Ctrl Pts',(-0.138911255368966,1.,2.04995762001333));
#31859=CARTESIAN_POINT('Ctrl Pts',(-0.136777941218044,1.,2.0557604441427));
#31860=CARTESIAN_POINT('Ctrl Pts',(-0.134598026192107,1.,2.06155781517844));
#31861=CARTESIAN_POINT('Ctrl Pts',(-0.13237211154771,1.,2.06735123910319));
#31862=CARTESIAN_POINT('Ctrl Pts',(-0.130100748328401,1.,2.07314114713047));
#31863=CARTESIAN_POINT('Ctrl Pts',(-0.127784445276116,1.,2.07892715110967));
#31864=CARTESIAN_POINT('Ctrl Pts',(-0.125423679412058,1.,2.08470840653628));
#31865=CARTESIAN_POINT('Ctrl Pts',(-0.123018905621083,1.,2.09048392424826));
#31866=CARTESIAN_POINT('Ctrl Pts',(-0.120570567965129,1.,2.09625292867756));
#31867=CARTESIAN_POINT('Ctrl Pts',(-0.118079107988368,1.,2.10201512132945));
#31868=CARTESIAN_POINT('Ctrl Pts',(-0.115544957687941,1.,2.10777050261359));
#31869=CARTESIAN_POINT('Ctrl Pts',(-0.112968534419746,1.,2.11351924490335));
#31870=CARTESIAN_POINT('Ctrl Pts',(-0.11035023613502,1.,2.11926155590849));
#31871=CARTESIAN_POINT('Ctrl Pts',(-0.107690435231068,1.,2.12499752306927));
#31872=CARTESIAN_POINT('Ctrl Pts',(-0.104989479152703,1.,2.1307270488718));
#31873=CARTESIAN_POINT('Ctrl Pts',(-0.102247700556064,1.,2.13644992667052));
#31874=CARTESIAN_POINT('Ctrl Pts',(-0.0994654261990745,1.,2.14216588395974));
#31875=CARTESIAN_POINT('Ctrl Pts',(-0.0966429852305691,1.,2.14787463531864));
#31876=CARTESIAN_POINT('Ctrl Pts',(-0.0937807218868348,1.,2.15357593978377));
#31877=CARTESIAN_POINT('Ctrl Pts',(-0.0908789888108269,1.,2.15926961544808));
#31878=CARTESIAN_POINT('Ctrl Pts',(-0.0879381291387825,1.,2.16495552645275));
#31879=CARTESIAN_POINT('Ctrl Pts',(-0.0849584620835646,1.,2.17063357871031));
#31880=CARTESIAN_POINT('Ctrl Pts',(-0.0819402680871942,1.,2.1763037121106));
#31881=CARTESIAN_POINT('Ctrl Pts',(-0.078883772768323,1.,2.18196589448304));
#31882=CARTESIAN_POINT('Ctrl Pts',(-0.0757891465833414,1.,2.1876201139874));
#31883=CARTESIAN_POINT('Ctrl Pts',(-0.0732830357304279,1.,2.19213712012956));
#31884=CARTESIAN_POINT('Ctrl Pts',(-0.071386377952463,1.,2.19552129483562));
#31885=CARTESIAN_POINT('Ctrl Pts',(-0.0701143536324929,1.,2.19777582085261));
#31886=CARTESIAN_POINT('Ctrl Pts',(-0.0694764450219586,1.,2.19890268624765));
#31887=CARTESIAN_POINT('',(-0.163289472382897,0.,1.74236521665491));
#31888=CARTESIAN_POINT('Origin',(0.,0.,0.));
#31889=CARTESIAN_POINT('',(-0.383122945602004,1.,1.7075470150345));
#31890=CARTESIAN_POINT('Origin',(0.,1.,0.));
#31891=CARTESIAN_POINT('',(-0.383122945602004,0.,1.7075470150345));
#31892=CARTESIAN_POINT('Ctrl Pts',(-0.61342227326009,-1.,2.11275013067528));
#31893=CARTESIAN_POINT('Ctrl Pts',(-0.61342227326009,1.,2.11275013067528));
#31894=CARTESIAN_POINT('Ctrl Pts',(-0.61246736556225,-1.,2.11187554260142));
#31895=CARTESIAN_POINT('Ctrl Pts',(-0.61246736556225,1.,2.11187554260142));
#31896=CARTESIAN_POINT('Ctrl Pts',(-0.610560911691113,-1.,2.11012443807661));
#31897=CARTESIAN_POINT('Ctrl Pts',(-0.610560911691113,1.,2.11012443807661));
#31898=CARTESIAN_POINT('Ctrl Pts',(-0.607711315456826,-1.,2.10749199615859));
#31899=CARTESIAN_POINT('Ctrl Pts',(-0.607711315456826,1.,2.10749199615859));
#31900=CARTESIAN_POINT('Ctrl Pts',(-0.603932030738212,-1.,2.10397049887709));
#31901=CARTESIAN_POINT('Ctrl Pts',(-0.603932030738212,1.,2.10397049887709));
#31902=CARTESIAN_POINT('Ctrl Pts',(-0.599241616422144,-1.,2.09954930865331));
#31903=CARTESIAN_POINT('Ctrl Pts',(-0.599241616422144,1.,2.09954930865331));
#31904=CARTESIAN_POINT('Ctrl Pts',(-0.594585006052824,-1.,2.09510876220501));
#31905=CARTESIAN_POINT('Ctrl Pts',(-0.594585006052824,1.,2.09510876220501));
#31906=CARTESIAN_POINT('Ctrl Pts',(-0.589962365403189,-1.,2.09064881812053));
#31907=CARTESIAN_POINT('Ctrl Pts',(-0.589962365403189,1.,2.09064881812053));
#31908=CARTESIAN_POINT('Ctrl Pts',(-0.585373918990895,-1.,2.086169437277));
#31909=CARTESIAN_POINT('Ctrl Pts',(-0.585373918990895,1.,2.086169437277));
#31910=CARTESIAN_POINT('Ctrl Pts',(-0.580819952107257,-1.,2.08167059018138));
#31911=CARTESIAN_POINT('Ctrl Pts',(-0.580819952107257,1.,2.08167059018138));
#31912=CARTESIAN_POINT('Ctrl Pts',(-0.576300797416275,-1.,2.07715226767361));
#31913=CARTESIAN_POINT('Ctrl Pts',(-0.576300797416275,1.,2.07715226767361));
#31914=CARTESIAN_POINT('Ctrl Pts',(-0.571816823242411,-1.,2.07261449292757));
#31915=CARTESIAN_POINT('Ctrl Pts',(-0.571816823242411,1.,2.07261449292757));
#31916=CARTESIAN_POINT('Ctrl Pts',(-0.567368421181229,-1.,2.06805732997383));
#31917=CARTESIAN_POINT('Ctrl Pts',(-0.567368421181229,1.,2.06805732997383));
#31918=CARTESIAN_POINT('Ctrl Pts',(-0.562955993082574,-1.,2.06348090160697));
#31919=CARTESIAN_POINT('Ctrl Pts',(-0.562955993082574,1.,2.06348090160697));
#31920=CARTESIAN_POINT('Ctrl Pts',(-0.558579940185467,-1.,2.05888537756571));
#31921=CARTESIAN_POINT('Ctrl Pts',(-0.558579940185467,1.,2.05888537756571));
#31922=CARTESIAN_POINT('Ctrl Pts',(-0.55424065746411,-1.,2.05427091604482));
#31923=CARTESIAN_POINT('Ctrl Pts',(-0.55424065746411,1.,2.05427091604482));
#31924=CARTESIAN_POINT('Ctrl Pts',(-0.549938525150342,-1.,2.04963761077974));
#31925=CARTESIAN_POINT('Ctrl Pts',(-0.549938525150342,1.,2.04963761077974));
#31926=CARTESIAN_POINT('Ctrl Pts',(-0.545673903817348,-1.,2.0449854471456));
#31927=CARTESIAN_POINT('Ctrl Pts',(-0.545673903817348,1.,2.0449854471456));
#31928=CARTESIAN_POINT('Ctrl Pts',(-0.54144712061552,-1.,2.0403142269048));
#31929=CARTESIAN_POINT('Ctrl Pts',(-0.54144712061552,1.,2.0403142269048));
#31930=CARTESIAN_POINT('Ctrl Pts',(-0.537258489833134,-1.,2.03562362953993));
#31931=CARTESIAN_POINT('Ctrl Pts',(-0.537258489833134,1.,2.03562362953993));
#31932=CARTESIAN_POINT('Ctrl Pts',(-0.533108355132905,-1.,2.03091336214401));
#31933=CARTESIAN_POINT('Ctrl Pts',(-0.533108355132905,1.,2.03091336214401));
#31934=CARTESIAN_POINT('Ctrl Pts',(-0.528997127241911,-1.,2.02618329083289));
#31935=CARTESIAN_POINT('Ctrl Pts',(-0.528997127241911,1.,2.02618329083289));
#31936=CARTESIAN_POINT('Ctrl Pts',(-0.524925318333518,-1.,2.02143356304712));
#31937=CARTESIAN_POINT('Ctrl Pts',(-0.524925318333518,1.,2.02143356304712));
#31938=CARTESIAN_POINT('Ctrl Pts',(-0.520893590399428,-1.,2.01666477917305));
#31939=CARTESIAN_POINT('Ctrl Pts',(-0.520893590399428,1.,2.01666477917305));
#31940=CARTESIAN_POINT('Ctrl Pts',(-0.516902681728733,-1.,2.01187773939257));
#31941=CARTESIAN_POINT('Ctrl Pts',(-0.516902681728733,1.,2.01187773939257));
#31942=CARTESIAN_POINT('Ctrl Pts',(-0.512953306961814,-1.,2.00707309946955));
#31943=CARTESIAN_POINT('Ctrl Pts',(-0.512953306961814,1.,2.00707309946955));
#31944=CARTESIAN_POINT('Ctrl Pts',(-0.509046069886152,-1.,2.00225107134733));
#31945=CARTESIAN_POINT('Ctrl Pts',(-0.509046069886152,1.,2.00225107134733));
#31946=CARTESIAN_POINT('Ctrl Pts',(-0.505181361323011,-1.,1.99741107463567));
#31947=CARTESIAN_POINT('Ctrl Pts',(-0.505181361323011,1.,1.99741107463567));
#31948=CARTESIAN_POINT('Ctrl Pts',(-0.501359287727129,-1.,1.9925514912615));
#31949=CARTESIAN_POINT('Ctrl Pts',(-0.501359287727129,1.,1.9925514912615));
#31950=CARTESIAN_POINT('Ctrl Pts',(-0.497579909545564,-1.,1.98767044752929));
#31951=CARTESIAN_POINT('Ctrl Pts',(-0.497579909545564,1.,1.98767044752929));
#31952=CARTESIAN_POINT('Ctrl Pts',(-0.493843476541492,-1.,1.9827665876182));
#31953=CARTESIAN_POINT('Ctrl Pts',(-0.493843476541492,1.,1.9827665876182));
#31954=CARTESIAN_POINT('Ctrl Pts',(-0.490150627860955,-1.,1.97783973019229));
#31955=CARTESIAN_POINT('Ctrl Pts',(-0.490150627860955,1.,1.97783973019229));
#31956=CARTESIAN_POINT('Ctrl Pts',(-0.486502692907661,-1.,1.97289186263272));
#31957=CARTESIAN_POINT('Ctrl Pts',(-0.486502692907661,1.,1.97289186263272));
#31958=CARTESIAN_POINT('Ctrl Pts',(-0.482901662120687,-1.,1.96792703422358));
#31959=CARTESIAN_POINT('Ctrl Pts',(-0.482901662120687,1.,1.96792703422358));
#31960=CARTESIAN_POINT('Ctrl Pts',(-0.479349583074846,-1.,1.96294933055938));
#31961=CARTESIAN_POINT('Ctrl Pts',(-0.479349583074846,1.,1.96294933055938));
#31962=CARTESIAN_POINT('Ctrl Pts',(-0.475848034683172,-1.,1.95796111148175));
#31963=CARTESIAN_POINT('Ctrl Pts',(-0.475848034683172,1.,1.95796111148175));
#31964=CARTESIAN_POINT('Ctrl Pts',(-0.47239767226408,-1.,1.95296148278136));
#31965=CARTESIAN_POINT('Ctrl Pts',(-0.47239767226408,1.,1.95296148278136));
#31966=CARTESIAN_POINT('Ctrl Pts',(-0.468997482913158,-1.,1.94794381136524));
#31967=CARTESIAN_POINT('Ctrl Pts',(-0.468997482913158,1.,1.94794381136524));
#31968=CARTESIAN_POINT('Ctrl Pts',(-0.465645462026065,-1.,1.94289794196205));
#31969=CARTESIAN_POINT('Ctrl Pts',(-0.465645462026065,1.,1.94289794196205));
#31970=CARTESIAN_POINT('Ctrl Pts',(-0.462340031009087,-1.,1.93781486640834));
#31971=CARTESIAN_POINT('Ctrl Pts',(-0.462340031009087,1.,1.93781486640834));
#31972=CARTESIAN_POINT('Ctrl Pts',(-0.459081234547931,-1.,1.93269066517936));
#31973=CARTESIAN_POINT('Ctrl Pts',(-0.459081234547931,1.,1.93269066517936));
#31974=CARTESIAN_POINT('Ctrl Pts',(-0.455872005174335,-1.,1.92753067150461));
#31975=CARTESIAN_POINT('Ctrl Pts',(-0.455872005174335,1.,1.92753067150461));
#31976=CARTESIAN_POINT('Ctrl Pts',(-0.452719478359356,-1.,1.9223538064847));
#31977=CARTESIAN_POINT('Ctrl Pts',(-0.452719478359356,1.,1.9223538064847));
#31978=CARTESIAN_POINT('Ctrl Pts',(-0.449632260106572,-1.,1.91718342555717));
#31979=CARTESIAN_POINT('Ctrl Pts',(-0.449632260106572,1.,1.91718342555717));
#31980=CARTESIAN_POINT('Ctrl Pts',(-0.446617343485651,-1.,1.91203699981095));
#31981=CARTESIAN_POINT('Ctrl Pts',(-0.446617343485651,1.,1.91203699981095));
#31982=CARTESIAN_POINT('Ctrl Pts',(-0.44367755684917,-1.,1.90691756144906));
#31983=CARTESIAN_POINT('Ctrl Pts',(-0.44367755684917,1.,1.90691756144906));
#31984=CARTESIAN_POINT('Ctrl Pts',(-0.440807833704161,-1.,1.90180124389137));
#31985=CARTESIAN_POINT('Ctrl Pts',(-0.440807833704161,1.,1.90180124389137));
#31986=CARTESIAN_POINT('Ctrl Pts',(-0.437995003948443,-1.,1.89663648956549));
#31987=CARTESIAN_POINT('Ctrl Pts',(-0.437995003948443,1.,1.89663648956549));
#31988=CARTESIAN_POINT('Ctrl Pts',(-0.43522566096358,-1.,1.89136993975585));
#31989=CARTESIAN_POINT('Ctrl Pts',(-0.43522566096358,1.,1.89136993975585));
#31990=CARTESIAN_POINT('Ctrl Pts',(-0.432493038548833,-1.,1.88596913666828));
#31991=CARTESIAN_POINT('Ctrl Pts',(-0.432493038548833,1.,1.88596913666828));
#31992=CARTESIAN_POINT('Ctrl Pts',(-0.429803062482217,-1.,1.88044229001778));
#31993=CARTESIAN_POINT('Ctrl Pts',(-0.429803062482217,1.,1.88044229001778));
#31994=CARTESIAN_POINT('Ctrl Pts',(-0.427183828518743,-1.,1.87486989291333));
#31995=CARTESIAN_POINT('Ctrl Pts',(-0.427183828518743,1.,1.87486989291333));
#31996=CARTESIAN_POINT('Ctrl Pts',(-0.424678177290876,-1.,1.8693780394412));
#31997=CARTESIAN_POINT('Ctrl Pts',(-0.424678177290876,1.,1.8693780394412));
#31998=CARTESIAN_POINT('Ctrl Pts',(-0.422327307417885,-1.,1.86408083333863));
#31999=CARTESIAN_POINT('Ctrl Pts',(-0.422327307417885,1.,1.86408083333863));
#32000=CARTESIAN_POINT('Ctrl Pts',(-0.420157287975583,-1.,1.8590328109667));
#32001=CARTESIAN_POINT('Ctrl Pts',(-0.420157287975583,1.,1.8590328109667));
#32002=CARTESIAN_POINT('Ctrl Pts',(-0.418164129144045,-1.,1.8541763285645));
#32003=CARTESIAN_POINT('Ctrl Pts',(-0.418164129144045,1.,1.8541763285645));
#32004=CARTESIAN_POINT('Ctrl Pts',(-0.416300022039885,-1.,1.84929312930314));
#32005=CARTESIAN_POINT('Ctrl Pts',(-0.416300022039885,1.,1.84929312930314));
#32006=CARTESIAN_POINT('Ctrl Pts',(-0.414487438255542,-1.,1.84405757074218));
#32007=CARTESIAN_POINT('Ctrl Pts',(-0.414487438255542,1.,1.84405757074218));
#32008=CARTESIAN_POINT('Ctrl Pts',(-0.412633125322945,-1.,1.8380895347617));
#32009=CARTESIAN_POINT('Ctrl Pts',(-0.412633125322945,1.,1.8380895347617));
#32010=CARTESIAN_POINT('Ctrl Pts',(-0.410641256301276,-1.,1.83100408895047));
#32011=CARTESIAN_POINT('Ctrl Pts',(-0.410641256301276,1.,1.83100408895047));
#32012=CARTESIAN_POINT('Ctrl Pts',(-0.408428948106227,-1.,1.82247022677562));
#32013=CARTESIAN_POINT('Ctrl Pts',(-0.408428948106227,1.,1.82247022677562));
#32014=CARTESIAN_POINT('Ctrl Pts',(-0.405933518407175,-1.,1.81223801812013));
#32015=CARTESIAN_POINT('Ctrl Pts',(-0.405933518407175,1.,1.81223801812013));
#32016=CARTESIAN_POINT('Ctrl Pts',(-0.403107976163396,-1.,1.80012077173238));
#32017=CARTESIAN_POINT('Ctrl Pts',(-0.403107976163396,1.,1.80012077173238));
#32018=CARTESIAN_POINT('Ctrl Pts',(-0.399919403774155,-1.,1.78598826343754));
#32019=CARTESIAN_POINT('Ctrl Pts',(-0.399919403774155,1.,1.78598826343754));
#32020=CARTESIAN_POINT('Ctrl Pts',(-0.396346196110688,-1.,1.76975560043442));
#32021=CARTESIAN_POINT('Ctrl Pts',(-0.396346196110688,1.,1.76975560043442));
#32022=CARTESIAN_POINT('Ctrl Pts',(-0.392375812285395,-1.,1.75137405310193));
#32023=CARTESIAN_POINT('Ctrl Pts',(-0.392375812285395,1.,1.75137405310193));
#32024=CARTESIAN_POINT('Ctrl Pts',(-0.388877023502615,-1.,1.73493170972829));
#32025=CARTESIAN_POINT('Ctrl Pts',(-0.388877023502615,1.,1.73493170972829));
#32026=CARTESIAN_POINT('Ctrl Pts',(-0.386070790323281,-1.,1.72162022244582));
#32027=CARTESIAN_POINT('Ctrl Pts',(-0.386070790323281,1.,1.72162022244582));
#32028=CARTESIAN_POINT('Ctrl Pts',(-0.384119047314215,-1.,1.71231062891398));
#32029=CARTESIAN_POINT('Ctrl Pts',(-0.384119047314215,1.,1.71231062891398));
#32030=CARTESIAN_POINT('Ctrl Pts',(-0.383122945602004,-1.,1.7075470150345));
#32031=CARTESIAN_POINT('Ctrl Pts',(-0.383122945602004,1.,1.7075470150345));
#32032=CARTESIAN_POINT('',(-0.61342227326009,1.,2.11275013067528));
#32033=CARTESIAN_POINT('Ctrl Pts',(-0.61342227326009,1.,2.11275013067528));
#32034=CARTESIAN_POINT('Ctrl Pts',(-0.61246736556225,1.,2.11187554260142));
#32035=CARTESIAN_POINT('Ctrl Pts',(-0.610560911691113,1.,2.11012443807661));
#32036=CARTESIAN_POINT('Ctrl Pts',(-0.607711315456826,1.,2.10749199615859));
#32037=CARTESIAN_POINT('Ctrl Pts',(-0.603932030738212,1.,2.10397049887709));
#32038=CARTESIAN_POINT('Ctrl Pts',(-0.599241616422144,1.,2.09954930865331));
#32039=CARTESIAN_POINT('Ctrl Pts',(-0.594585006052824,1.,2.09510876220501));
#32040=CARTESIAN_POINT('Ctrl Pts',(-0.589962365403189,1.,2.09064881812053));
#32041=CARTESIAN_POINT('Ctrl Pts',(-0.585373918990895,1.,2.086169437277));
#32042=CARTESIAN_POINT('Ctrl Pts',(-0.580819952107257,1.,2.08167059018138));
#32043=CARTESIAN_POINT('Ctrl Pts',(-0.576300797416275,1.,2.07715226767361));
#32044=CARTESIAN_POINT('Ctrl Pts',(-0.571816823242411,1.,2.07261449292757));
#32045=CARTESIAN_POINT('Ctrl Pts',(-0.567368421181229,1.,2.06805732997383));
#32046=CARTESIAN_POINT('Ctrl Pts',(-0.562955993082574,1.,2.06348090160697));
#32047=CARTESIAN_POINT('Ctrl Pts',(-0.558579940185467,1.,2.05888537756571));
#32048=CARTESIAN_POINT('Ctrl Pts',(-0.55424065746411,1.,2.05427091604482));
#32049=CARTESIAN_POINT('Ctrl Pts',(-0.549938525150342,1.,2.04963761077974));
#32050=CARTESIAN_POINT('Ctrl Pts',(-0.545673903817348,1.,2.0449854471456));
#32051=CARTESIAN_POINT('Ctrl Pts',(-0.54144712061552,1.,2.0403142269048));
#32052=CARTESIAN_POINT('Ctrl Pts',(-0.537258489833134,1.,2.03562362953993));
#32053=CARTESIAN_POINT('Ctrl Pts',(-0.533108355132905,1.,2.03091336214401));
#32054=CARTESIAN_POINT('Ctrl Pts',(-0.528997127241911,1.,2.02618329083289));
#32055=CARTESIAN_POINT('Ctrl Pts',(-0.524925318333518,1.,2.02143356304712));
#32056=CARTESIAN_POINT('Ctrl Pts',(-0.520893590399428,1.,2.01666477917305));
#32057=CARTESIAN_POINT('Ctrl Pts',(-0.516902681728733,1.,2.01187773939257));
#32058=CARTESIAN_POINT('Ctrl Pts',(-0.512953306961814,1.,2.00707309946955));
#32059=CARTESIAN_POINT('Ctrl Pts',(-0.509046069886152,1.,2.00225107134733));
#32060=CARTESIAN_POINT('Ctrl Pts',(-0.505181361323011,1.,1.99741107463567));
#32061=CARTESIAN_POINT('Ctrl Pts',(-0.501359287727129,1.,1.9925514912615));
#32062=CARTESIAN_POINT('Ctrl Pts',(-0.497579909545564,1.,1.98767044752929));
#32063=CARTESIAN_POINT('Ctrl Pts',(-0.493843476541492,1.,1.9827665876182));
#32064=CARTESIAN_POINT('Ctrl Pts',(-0.490150627860955,1.,1.97783973019229));
#32065=CARTESIAN_POINT('Ctrl Pts',(-0.486502692907661,1.,1.97289186263272));
#32066=CARTESIAN_POINT('Ctrl Pts',(-0.482901662120687,1.,1.96792703422358));
#32067=CARTESIAN_POINT('Ctrl Pts',(-0.479349583074846,1.,1.96294933055938));
#32068=CARTESIAN_POINT('Ctrl Pts',(-0.475848034683172,1.,1.95796111148175));
#32069=CARTESIAN_POINT('Ctrl Pts',(-0.47239767226408,1.,1.95296148278136));
#32070=CARTESIAN_POINT('Ctrl Pts',(-0.468997482913158,1.,1.94794381136524));
#32071=CARTESIAN_POINT('Ctrl Pts',(-0.465645462026065,1.,1.94289794196205));
#32072=CARTESIAN_POINT('Ctrl Pts',(-0.462340031009087,1.,1.93781486640834));
#32073=CARTESIAN_POINT('Ctrl Pts',(-0.459081234547931,1.,1.93269066517936));
#32074=CARTESIAN_POINT('Ctrl Pts',(-0.455872005174335,1.,1.92753067150461));
#32075=CARTESIAN_POINT('Ctrl Pts',(-0.452719478359356,1.,1.9223538064847));
#32076=CARTESIAN_POINT('Ctrl Pts',(-0.449632260106572,1.,1.91718342555717));
#32077=CARTESIAN_POINT('Ctrl Pts',(-0.446617343485651,1.,1.91203699981095));
#32078=CARTESIAN_POINT('Ctrl Pts',(-0.44367755684917,1.,1.90691756144906));
#32079=CARTESIAN_POINT('Ctrl Pts',(-0.440807833704161,1.,1.90180124389137));
#32080=CARTESIAN_POINT('Ctrl Pts',(-0.437995003948443,1.,1.89663648956549));
#32081=CARTESIAN_POINT('Ctrl Pts',(-0.43522566096358,1.,1.89136993975585));
#32082=CARTESIAN_POINT('Ctrl Pts',(-0.432493038548833,1.,1.88596913666828));
#32083=CARTESIAN_POINT('Ctrl Pts',(-0.429803062482217,1.,1.88044229001778));
#32084=CARTESIAN_POINT('Ctrl Pts',(-0.427183828518743,1.,1.87486989291333));
#32085=CARTESIAN_POINT('Ctrl Pts',(-0.424678177290876,1.,1.8693780394412));
#32086=CARTESIAN_POINT('Ctrl Pts',(-0.422327307417885,1.,1.86408083333863));
#32087=CARTESIAN_POINT('Ctrl Pts',(-0.420157287975583,1.,1.8590328109667));
#32088=CARTESIAN_POINT('Ctrl Pts',(-0.418164129144045,1.,1.8541763285645));
#32089=CARTESIAN_POINT('Ctrl Pts',(-0.416300022039885,1.,1.84929312930314));
#32090=CARTESIAN_POINT('Ctrl Pts',(-0.414487438255542,1.,1.84405757074218));
#32091=CARTESIAN_POINT('Ctrl Pts',(-0.412633125322945,1.,1.8380895347617));
#32092=CARTESIAN_POINT('Ctrl Pts',(-0.410641256301276,1.,1.83100408895047));
#32093=CARTESIAN_POINT('Ctrl Pts',(-0.408428948106227,1.,1.82247022677562));
#32094=CARTESIAN_POINT('Ctrl Pts',(-0.405933518407175,1.,1.81223801812013));
#32095=CARTESIAN_POINT('Ctrl Pts',(-0.403107976163396,1.,1.80012077173238));
#32096=CARTESIAN_POINT('Ctrl Pts',(-0.399919403774155,1.,1.78598826343754));
#32097=CARTESIAN_POINT('Ctrl Pts',(-0.396346196110688,1.,1.76975560043442));
#32098=CARTESIAN_POINT('Ctrl Pts',(-0.392375812285395,1.,1.75137405310193));
#32099=CARTESIAN_POINT('Ctrl Pts',(-0.388877023502615,1.,1.73493170972829));
#32100=CARTESIAN_POINT('Ctrl Pts',(-0.386070790323281,1.,1.72162022244582));
#32101=CARTESIAN_POINT('Ctrl Pts',(-0.384119047314215,1.,1.71231062891398));
#32102=CARTESIAN_POINT('Ctrl Pts',(-0.383122945602004,1.,1.7075470150345));
#32103=CARTESIAN_POINT('',(-0.61342227326009,0.,2.11275013067528));
#32104=CARTESIAN_POINT('Origin',(-0.745574324794401,0.,2.0698113262342));
#32105=CARTESIAN_POINT('',(-0.745574324794401,1.,2.0698113262342));
#32106=CARTESIAN_POINT('',(-0.61342227326009,1.,2.11275013067528));
#32107=CARTESIAN_POINT('',(-0.745574324794401,0.,2.0698113262342));
#32108=CARTESIAN_POINT('Ctrl Pts',(-0.693717979106306,-1.,1.60662857109684));
#32109=CARTESIAN_POINT('Ctrl Pts',(-0.693717979106306,1.,1.60662857109684));
#32110=CARTESIAN_POINT('Ctrl Pts',(-0.695712097881194,-1.,1.61106790958151));
#32111=CARTESIAN_POINT('Ctrl Pts',(-0.695712097881194,1.,1.61106790958151));
#32112=CARTESIAN_POINT('Ctrl Pts',(-0.699605146405088,-1.,1.61974673472612));
#32113=CARTESIAN_POINT('Ctrl Pts',(-0.699605146405088,1.,1.61974673472612));
#32114=CARTESIAN_POINT('Ctrl Pts',(-0.705159151988319,-1.,1.63216541664676));
#32115=CARTESIAN_POINT('Ctrl Pts',(-0.705159151988319,1.,1.63216541664676));
#32116=CARTESIAN_POINT('Ctrl Pts',(-0.711993139355394,-1.,1.64752408832016));
#32117=CARTESIAN_POINT('Ctrl Pts',(-0.711993139355394,1.,1.64752408832016));
#32118=CARTESIAN_POINT('Ctrl Pts',(-0.719585433804282,-1.,1.6647288055568));
#32119=CARTESIAN_POINT('Ctrl Pts',(-0.719585433804282,1.,1.6647288055568));
#32120=CARTESIAN_POINT('Ctrl Pts',(-0.726235967997433,-1.,1.67996158455503));
#32121=CARTESIAN_POINT('Ctrl Pts',(-0.726235967997433,1.,1.67996158455503));
#32122=CARTESIAN_POINT('Ctrl Pts',(-0.731963238697195,-1.,1.69326921975743));
#32123=CARTESIAN_POINT('Ctrl Pts',(-0.731963238697195,1.,1.69326921975743));
#32124=CARTESIAN_POINT('Ctrl Pts',(-0.736799665724771,-1.,1.70473309006121));
#32125=CARTESIAN_POINT('Ctrl Pts',(-0.736799665724771,1.,1.70473309006121));
#32126=CARTESIAN_POINT('Ctrl Pts',(-0.740795162032088,-1.,1.71447789751927));
#32127=CARTESIAN_POINT('Ctrl Pts',(-0.740795162032088,1.,1.71447789751927));
#32128=CARTESIAN_POINT('Ctrl Pts',(-0.744021445433764,-1.,1.7226822991693));
#32129=CARTESIAN_POINT('Ctrl Pts',(-0.744021445433764,1.,1.7226822991693));
#32130=CARTESIAN_POINT('Ctrl Pts',(-0.746574710096436,-1.,1.72958533647399));
#32131=CARTESIAN_POINT('Ctrl Pts',(-0.746574710096436,1.,1.72958533647399));
#32132=CARTESIAN_POINT('Ctrl Pts',(-0.748582462954855,-1.,1.73550351679848));
#32133=CARTESIAN_POINT('Ctrl Pts',(-0.748582462954855,1.,1.73550351679848));
#32134=CARTESIAN_POINT('Ctrl Pts',(-0.75019343597954,-1.,1.74080458266705));
#32135=CARTESIAN_POINT('Ctrl Pts',(-0.75019343597954,1.,1.74080458266705));
#32136=CARTESIAN_POINT('Ctrl Pts',(-0.751555614163629,-1.,1.74585086852298));
#32137=CARTESIAN_POINT('Ctrl Pts',(-0.751555614163629,1.,1.74585086852298));
#32138=CARTESIAN_POINT('Ctrl Pts',(-0.752797683531377,-1.,1.75095139468809));
#32139=CARTESIAN_POINT('Ctrl Pts',(-0.752797683531377,1.,1.75095139468809));
#32140=CARTESIAN_POINT('Ctrl Pts',(-0.75400925402848,-1.,1.75631083600175));
#32141=CARTESIAN_POINT('Ctrl Pts',(-0.75400925402848,1.,1.75631083600175));
#32142=CARTESIAN_POINT('Ctrl Pts',(-0.755220979975262,-1.,1.7619781724032));
#32143=CARTESIAN_POINT('Ctrl Pts',(-0.755220979975262,1.,1.7619781724032));
#32144=CARTESIAN_POINT('Ctrl Pts',(-0.756421896028403,-1.,1.76789396003141));
#32145=CARTESIAN_POINT('Ctrl Pts',(-0.756421896028403,1.,1.76789396003141));
#32146=CARTESIAN_POINT('Ctrl Pts',(-0.757578264077238,-1.,1.77394167108342));
#32147=CARTESIAN_POINT('Ctrl Pts',(-0.757578264077238,1.,1.77394167108342));
#32148=CARTESIAN_POINT('Ctrl Pts',(-0.75865062667738,-1.,1.77999411220912));
#32149=CARTESIAN_POINT('Ctrl Pts',(-0.75865062667738,1.,1.77999411220912));
#32150=CARTESIAN_POINT('Ctrl Pts',(-0.759614401109868,-1.,1.78596964884526));
#32151=CARTESIAN_POINT('Ctrl Pts',(-0.759614401109868,1.,1.78596964884526));
#32152=CARTESIAN_POINT('Ctrl Pts',(-0.760469555880425,-1.,1.79185815610802));
#32153=CARTESIAN_POINT('Ctrl Pts',(-0.760469555880425,1.,1.79185815610802));
#32154=CARTESIAN_POINT('Ctrl Pts',(-0.761229695230359,-1.,1.79768986997735));
#32155=CARTESIAN_POINT('Ctrl Pts',(-0.761229695230359,1.,1.79768986997735));
#32156=CARTESIAN_POINT('Ctrl Pts',(-0.761915336443516,-1.,1.80351583877334));
#32157=CARTESIAN_POINT('Ctrl Pts',(-0.761915336443516,1.,1.80351583877334));
#32158=CARTESIAN_POINT('Ctrl Pts',(-0.762546129464036,-1.,1.80938551463989));
#32159=CARTESIAN_POINT('Ctrl Pts',(-0.762546129464036,1.,1.80938551463989));
#32160=CARTESIAN_POINT('Ctrl Pts',(-0.763132003836783,-1.,1.81532118405566));
#32161=CARTESIAN_POINT('Ctrl Pts',(-0.763132003836783,1.,1.81532118405566));
#32162=CARTESIAN_POINT('Ctrl Pts',(-0.763673465462854,-1.,1.82131873145297));
#32163=CARTESIAN_POINT('Ctrl Pts',(-0.763673465462854,1.,1.82131873145297));
#32164=CARTESIAN_POINT('Ctrl Pts',(-0.764165902606055,-1.,1.8273599120008));
#32165=CARTESIAN_POINT('Ctrl Pts',(-0.764165902606055,1.,1.8273599120008));
#32166=CARTESIAN_POINT('Ctrl Pts',(-0.764602549687845,-1.,1.8334207722714));
#32167=CARTESIAN_POINT('Ctrl Pts',(-0.764602549687845,1.,1.8334207722714));
#32168=CARTESIAN_POINT('Ctrl Pts',(-0.764978057881687,-1.,1.83948181064823));
#32169=CARTESIAN_POINT('Ctrl Pts',(-0.764978057881687,1.,1.83948181064823));
#32170=CARTESIAN_POINT('Ctrl Pts',(-0.765291664861971,-1.,1.8455369887591));
#32171=CARTESIAN_POINT('Ctrl Pts',(-0.765291664861971,1.,1.8455369887591));
#32172=CARTESIAN_POINT('Ctrl Pts',(-0.765545710619023,-1.,1.85158945130054));
#32173=CARTESIAN_POINT('Ctrl Pts',(-0.765545710619023,1.,1.85158945130054));
#32174=CARTESIAN_POINT('Ctrl Pts',(-0.765744212909305,-1.,1.85764741390391));
#32175=CARTESIAN_POINT('Ctrl Pts',(-0.765744212909305,1.,1.85764741390391));
#32176=CARTESIAN_POINT('Ctrl Pts',(-0.765891519092557,-1.,1.86372027063314));
#32177=CARTESIAN_POINT('Ctrl Pts',(-0.765891519092557,1.,1.86372027063314));
#32178=CARTESIAN_POINT('Ctrl Pts',(-0.765990708546111,-1.,1.86981398314345));
#32179=CARTESIAN_POINT('Ctrl Pts',(-0.765990708546111,1.,1.86981398314345));
#32180=CARTESIAN_POINT('Ctrl Pts',(-0.766042837036759,-1.,1.87592888967886));
#32181=CARTESIAN_POINT('Ctrl Pts',(-0.766042837036759,1.,1.87592888967886));
#32182=CARTESIAN_POINT('Ctrl Pts',(-0.766047794851869,-1.,1.88206215302561));
#32183=CARTESIAN_POINT('Ctrl Pts',(-0.766047794851869,1.,1.88206215302561));
#32184=CARTESIAN_POINT('Ctrl Pts',(-0.76600483706209,-1.,1.88820926433409));
#32185=CARTESIAN_POINT('Ctrl Pts',(-0.76600483706209,1.,1.88820926433409));
#32186=CARTESIAN_POINT('Ctrl Pts',(-0.765913193856979,-1.,1.89436577771389));
#32187=CARTESIAN_POINT('Ctrl Pts',(-0.765913193856979,1.,1.89436577771389));
#32188=CARTESIAN_POINT('Ctrl Pts',(-0.765772772593395,-1.,1.90052930393599));
#32189=CARTESIAN_POINT('Ctrl Pts',(-0.765772772593395,1.,1.90052930393599));
#32190=CARTESIAN_POINT('Ctrl Pts',(-0.765584196937936,-1.,1.90669961402362));
#32191=CARTESIAN_POINT('Ctrl Pts',(-0.765584196937936,1.,1.90669961402362));
#32192=CARTESIAN_POINT('Ctrl Pts',(-0.765348465884739,-1.,1.91287765805174));
#32193=CARTESIAN_POINT('Ctrl Pts',(-0.765348465884739,1.,1.91287765805174));
#32194=CARTESIAN_POINT('Ctrl Pts',(-0.765066729667095,-1.,1.91906491634197));
#32195=CARTESIAN_POINT('Ctrl Pts',(-0.765066729667095,1.,1.91906491634197));
#32196=CARTESIAN_POINT('Ctrl Pts',(-0.764740025488189,-1.,1.92526263537041));
#32197=CARTESIAN_POINT('Ctrl Pts',(-0.764740025488189,1.,1.92526263537041));
#32198=CARTESIAN_POINT('Ctrl Pts',(-0.764369010673889,-1.,1.93147105496367));
#32199=CARTESIAN_POINT('Ctrl Pts',(-0.764369010673889,1.,1.93147105496367));
#32200=CARTESIAN_POINT('Ctrl Pts',(-0.763954049121393,-1.,1.93768964875867));
#32201=CARTESIAN_POINT('Ctrl Pts',(-0.763954049121393,1.,1.93768964875867));
#32202=CARTESIAN_POINT('Ctrl Pts',(-0.76349533353858,-1.,1.94391746617626));
#32203=CARTESIAN_POINT('Ctrl Pts',(-0.76349533353858,1.,1.94391746617626));
#32204=CARTESIAN_POINT('Ctrl Pts',(-0.762992990878774,-1.,1.95015342590025));
#32205=CARTESIAN_POINT('Ctrl Pts',(-0.762992990878774,1.,1.95015342590025));
#32206=CARTESIAN_POINT('Ctrl Pts',(-0.762447203806263,-1.,1.95639665309893));
#32207=CARTESIAN_POINT('Ctrl Pts',(-0.762447203806263,1.,1.95639665309893));
#32208=CARTESIAN_POINT('Ctrl Pts',(-0.761858300014575,-1.,1.96264672744229));
#32209=CARTESIAN_POINT('Ctrl Pts',(-0.761858300014575,1.,1.96264672744229));
#32210=CARTESIAN_POINT('Ctrl Pts',(-0.761226690483986,-1.,1.96890351582545));
#32211=CARTESIAN_POINT('Ctrl Pts',(-0.761226690483986,1.,1.96890351582545));
#32212=CARTESIAN_POINT('Ctrl Pts',(-0.760552825409855,-1.,1.97516705321521));
#32213=CARTESIAN_POINT('Ctrl Pts',(-0.760552825409855,1.,1.97516705321521));
#32214=CARTESIAN_POINT('Ctrl Pts',(-0.759837147452135,-1.,1.98143741418156));
#32215=CARTESIAN_POINT('Ctrl Pts',(-0.759837147452135,1.,1.98143741418156));
#32216=CARTESIAN_POINT('Ctrl Pts',(-0.759080037802243,-1.,1.98771456680806));
#32217=CARTESIAN_POINT('Ctrl Pts',(-0.759080037802243,1.,1.98771456680806));
#32218=CARTESIAN_POINT('Ctrl Pts',(-0.758281796766377,-1.,1.9939983109871));
#32219=CARTESIAN_POINT('Ctrl Pts',(-0.758281796766377,1.,1.9939983109871));
#32220=CARTESIAN_POINT('Ctrl Pts',(-0.757442676862341,-1.,2.00028834739072));
#32221=CARTESIAN_POINT('Ctrl Pts',(-0.757442676862341,1.,2.00028834739072));
#32222=CARTESIAN_POINT('Ctrl Pts',(-0.756562904646496,-1.,2.00658431587682));
#32223=CARTESIAN_POINT('Ctrl Pts',(-0.756562904646496,1.,2.00658431587682));
#32224=CARTESIAN_POINT('Ctrl Pts',(-0.7556427049581,-1.,2.01288584328149));
#32225=CARTESIAN_POINT('Ctrl Pts',(-0.7556427049581,1.,2.01288584328149));
#32226=CARTESIAN_POINT('Ctrl Pts',(-0.75468233072352,-1.,2.01919259406003));
#32227=CARTESIAN_POINT('Ctrl Pts',(-0.75468233072352,1.,2.01919259406003));
#32228=CARTESIAN_POINT('Ctrl Pts',(-0.753682061113766,-1.,2.02550428623587));
#32229=CARTESIAN_POINT('Ctrl Pts',(-0.753682061113766,1.,2.02550428623587));
#32230=CARTESIAN_POINT('Ctrl Pts',(-0.752642180488104,-1.,2.03182068456467));
#32231=CARTESIAN_POINT('Ctrl Pts',(-0.752642180488104,1.,2.03182068456467));
#32232=CARTESIAN_POINT('Ctrl Pts',(-0.751562963361384,-1.,2.03814160092173));
#32233=CARTESIAN_POINT('Ctrl Pts',(-0.751562963361384,1.,2.03814160092173));
#32234=CARTESIAN_POINT('Ctrl Pts',(-0.750444657874758,-1.,2.04446689147754));
#32235=CARTESIAN_POINT('Ctrl Pts',(-0.750444657874758,1.,2.04446689147754));
#32236=CARTESIAN_POINT('Ctrl Pts',(-0.749287468663053,-1.,2.05079645591606));
#32237=CARTESIAN_POINT('Ctrl Pts',(-0.749287468663053,1.,2.05079645591606));
#32238=CARTESIAN_POINT('Ctrl Pts',(-0.748091554181101,-1.,2.05713023030263));
#32239=CARTESIAN_POINT('Ctrl Pts',(-0.748091554181101,1.,2.05713023030263));
#32240=CARTESIAN_POINT('Ctrl Pts',(-0.747103932785504,-1.,2.06220058927162));
#32241=CARTESIAN_POINT('Ctrl Pts',(-0.747103932785504,1.,2.06220058927162));
#32242=CARTESIAN_POINT('Ctrl Pts',(-0.746345871542696,-1.,2.06600523016401));
#32243=CARTESIAN_POINT('Ctrl Pts',(-0.746345871542696,1.,2.06600523016401));
#32244=CARTESIAN_POINT('Ctrl Pts',(-0.74583279137781,-1.,2.06854248895575));
#32245=CARTESIAN_POINT('Ctrl Pts',(-0.74583279137781,1.,2.06854248895575));
#32246=CARTESIAN_POINT('Ctrl Pts',(-0.745574324794401,-1.,2.0698113262342));
#32247=CARTESIAN_POINT('Ctrl Pts',(-0.745574324794401,1.,2.0698113262342));
#32248=CARTESIAN_POINT('',(-0.693717979106306,1.,1.60662857109684));
#32249=CARTESIAN_POINT('Ctrl Pts',(-0.693717979106306,1.,1.60662857109684));
#32250=CARTESIAN_POINT('Ctrl Pts',(-0.695712097881194,1.,1.61106790958151));
#32251=CARTESIAN_POINT('Ctrl Pts',(-0.699605146405088,1.,1.61974673472612));
#32252=CARTESIAN_POINT('Ctrl Pts',(-0.705159151988319,1.,1.63216541664676));
#32253=CARTESIAN_POINT('Ctrl Pts',(-0.711993139355394,1.,1.64752408832016));
#32254=CARTESIAN_POINT('Ctrl Pts',(-0.719585433804282,1.,1.6647288055568));
#32255=CARTESIAN_POINT('Ctrl Pts',(-0.726235967997433,1.,1.67996158455503));
#32256=CARTESIAN_POINT('Ctrl Pts',(-0.731963238697195,1.,1.69326921975743));
#32257=CARTESIAN_POINT('Ctrl Pts',(-0.736799665724771,1.,1.70473309006121));
#32258=CARTESIAN_POINT('Ctrl Pts',(-0.740795162032088,1.,1.71447789751927));
#32259=CARTESIAN_POINT('Ctrl Pts',(-0.744021445433764,1.,1.7226822991693));
#32260=CARTESIAN_POINT('Ctrl Pts',(-0.746574710096436,1.,1.72958533647399));
#32261=CARTESIAN_POINT('Ctrl Pts',(-0.748582462954855,1.,1.73550351679848));
#32262=CARTESIAN_POINT('Ctrl Pts',(-0.75019343597954,1.,1.74080458266705));
#32263=CARTESIAN_POINT('Ctrl Pts',(-0.751555614163629,1.,1.74585086852298));
#32264=CARTESIAN_POINT('Ctrl Pts',(-0.752797683531377,1.,1.75095139468809));
#32265=CARTESIAN_POINT('Ctrl Pts',(-0.75400925402848,1.,1.75631083600175));
#32266=CARTESIAN_POINT('Ctrl Pts',(-0.755220979975262,1.,1.7619781724032));
#32267=CARTESIAN_POINT('Ctrl Pts',(-0.756421896028403,1.,1.76789396003141));
#32268=CARTESIAN_POINT('Ctrl Pts',(-0.757578264077238,1.,1.77394167108342));
#32269=CARTESIAN_POINT('Ctrl Pts',(-0.75865062667738,1.,1.77999411220912));
#32270=CARTESIAN_POINT('Ctrl Pts',(-0.759614401109868,1.,1.78596964884526));
#32271=CARTESIAN_POINT('Ctrl Pts',(-0.760469555880425,1.,1.79185815610802));
#32272=CARTESIAN_POINT('Ctrl Pts',(-0.761229695230359,1.,1.79768986997735));
#32273=CARTESIAN_POINT('Ctrl Pts',(-0.761915336443516,1.,1.80351583877334));
#32274=CARTESIAN_POINT('Ctrl Pts',(-0.762546129464036,1.,1.80938551463989));
#32275=CARTESIAN_POINT('Ctrl Pts',(-0.763132003836783,1.,1.81532118405566));
#32276=CARTESIAN_POINT('Ctrl Pts',(-0.763673465462854,1.,1.82131873145297));
#32277=CARTESIAN_POINT('Ctrl Pts',(-0.764165902606055,1.,1.8273599120008));
#32278=CARTESIAN_POINT('Ctrl Pts',(-0.764602549687845,1.,1.8334207722714));
#32279=CARTESIAN_POINT('Ctrl Pts',(-0.764978057881687,1.,1.83948181064823));
#32280=CARTESIAN_POINT('Ctrl Pts',(-0.765291664861971,1.,1.8455369887591));
#32281=CARTESIAN_POINT('Ctrl Pts',(-0.765545710619023,1.,1.85158945130054));
#32282=CARTESIAN_POINT('Ctrl Pts',(-0.765744212909305,1.,1.85764741390391));
#32283=CARTESIAN_POINT('Ctrl Pts',(-0.765891519092557,1.,1.86372027063314));
#32284=CARTESIAN_POINT('Ctrl Pts',(-0.765990708546111,1.,1.86981398314345));
#32285=CARTESIAN_POINT('Ctrl Pts',(-0.766042837036759,1.,1.87592888967886));
#32286=CARTESIAN_POINT('Ctrl Pts',(-0.766047794851869,1.,1.88206215302561));
#32287=CARTESIAN_POINT('Ctrl Pts',(-0.76600483706209,1.,1.88820926433409));
#32288=CARTESIAN_POINT('Ctrl Pts',(-0.765913193856979,1.,1.89436577771389));
#32289=CARTESIAN_POINT('Ctrl Pts',(-0.765772772593395,1.,1.90052930393599));
#32290=CARTESIAN_POINT('Ctrl Pts',(-0.765584196937936,1.,1.90669961402362));
#32291=CARTESIAN_POINT('Ctrl Pts',(-0.765348465884739,1.,1.91287765805174));
#32292=CARTESIAN_POINT('Ctrl Pts',(-0.765066729667095,1.,1.91906491634197));
#32293=CARTESIAN_POINT('Ctrl Pts',(-0.764740025488189,1.,1.92526263537041));
#32294=CARTESIAN_POINT('Ctrl Pts',(-0.764369010673889,1.,1.93147105496367));
#32295=CARTESIAN_POINT('Ctrl Pts',(-0.763954049121393,1.,1.93768964875867));
#32296=CARTESIAN_POINT('Ctrl Pts',(-0.76349533353858,1.,1.94391746617626));
#32297=CARTESIAN_POINT('Ctrl Pts',(-0.762992990878774,1.,1.95015342590025));
#32298=CARTESIAN_POINT('Ctrl Pts',(-0.762447203806263,1.,1.95639665309893));
#32299=CARTESIAN_POINT('Ctrl Pts',(-0.761858300014575,1.,1.96264672744229));
#32300=CARTESIAN_POINT('Ctrl Pts',(-0.761226690483986,1.,1.96890351582545));
#32301=CARTESIAN_POINT('Ctrl Pts',(-0.760552825409855,1.,1.97516705321521));
#32302=CARTESIAN_POINT('Ctrl Pts',(-0.759837147452135,1.,1.98143741418156));
#32303=CARTESIAN_POINT('Ctrl Pts',(-0.759080037802243,1.,1.98771456680806));
#32304=CARTESIAN_POINT('Ctrl Pts',(-0.758281796766377,1.,1.9939983109871));
#32305=CARTESIAN_POINT('Ctrl Pts',(-0.757442676862341,1.,2.00028834739072));
#32306=CARTESIAN_POINT('Ctrl Pts',(-0.756562904646496,1.,2.00658431587682));
#32307=CARTESIAN_POINT('Ctrl Pts',(-0.7556427049581,1.,2.01288584328149));
#32308=CARTESIAN_POINT('Ctrl Pts',(-0.75468233072352,1.,2.01919259406003));
#32309=CARTESIAN_POINT('Ctrl Pts',(-0.753682061113766,1.,2.02550428623587));
#32310=CARTESIAN_POINT('Ctrl Pts',(-0.752642180488104,1.,2.03182068456467));
#32311=CARTESIAN_POINT('Ctrl Pts',(-0.751562963361384,1.,2.03814160092173));
#32312=CARTESIAN_POINT('Ctrl Pts',(-0.750444657874758,1.,2.04446689147754));
#32313=CARTESIAN_POINT('Ctrl Pts',(-0.749287468663053,1.,2.05079645591606));
#32314=CARTESIAN_POINT('Ctrl Pts',(-0.748091554181101,1.,2.05713023030263));
#32315=CARTESIAN_POINT('Ctrl Pts',(-0.747103932785504,1.,2.06220058927162));
#32316=CARTESIAN_POINT('Ctrl Pts',(-0.746345871542696,1.,2.06600523016401));
#32317=CARTESIAN_POINT('Ctrl Pts',(-0.74583279137781,1.,2.06854248895575));
#32318=CARTESIAN_POINT('Ctrl Pts',(-0.745574324794401,1.,2.0698113262342));
#32319=CARTESIAN_POINT('',(-0.693717979106306,0.,1.60662857109684));
#32320=CARTESIAN_POINT('Origin',(0.,0.,0.));
#32321=CARTESIAN_POINT('',(-0.892032620296855,1.,1.5055822144029));
#32322=CARTESIAN_POINT('Origin',(0.,1.,0.));
#32323=CARTESIAN_POINT('',(-0.892032620296855,0.,1.5055822144029));
#32324=CARTESIAN_POINT('Ctrl Pts',(-1.23627494547115,-1.,1.81978687191668));
#32325=CARTESIAN_POINT('Ctrl Pts',(-1.23627494547115,1.,1.81978687191668));
#32326=CARTESIAN_POINT('Ctrl Pts',(-1.23509651170476,-1.,1.81925017193666));
#32327=CARTESIAN_POINT('Ctrl Pts',(-1.23509651170476,1.,1.81925017193666));
#32328=CARTESIAN_POINT('Ctrl Pts',(-1.2327422452705,-1.,1.81817389921279));
#32329=CARTESIAN_POINT('Ctrl Pts',(-1.2327422452705,1.,1.81817389921279));
#32330=CARTESIAN_POINT('Ctrl Pts',(-1.2292186489137,-1.,1.8165508718364));
#32331=CARTESIAN_POINT('Ctrl Pts',(-1.2292186489137,1.,1.8165508718364));
#32332=CARTESIAN_POINT('Ctrl Pts',(-1.2245361330495,-1.,1.81436959210434));
#32333=CARTESIAN_POINT('Ctrl Pts',(-1.2245361330495,1.,1.81436959210434));
#32334=CARTESIAN_POINT('Ctrl Pts',(-1.21870906103557,-1.,1.81161420806656));
#32335=CARTESIAN_POINT('Ctrl Pts',(-1.21870906103557,1.,1.81161420806656));
#32336=CARTESIAN_POINT('Ctrl Pts',(-1.21290815708314,-1.,1.80882996917129));
#32337=CARTESIAN_POINT('Ctrl Pts',(-1.21290815708314,1.,1.80882996917129));
#32338=CARTESIAN_POINT('Ctrl Pts',(-1.20713356605475,-1.,1.80601678480707));
#32339=CARTESIAN_POINT('Ctrl Pts',(-1.20713356605475,1.,1.80601678480707));
#32340=CARTESIAN_POINT('Ctrl Pts',(-1.20138548938974,-1.,1.80317454838603));
#32341=CARTESIAN_POINT('Ctrl Pts',(-1.20138548938974,1.,1.80317454838603));
#32342=CARTESIAN_POINT('Ctrl Pts',(-1.19566418930242,-1.,1.80030314369879));
#32343=CARTESIAN_POINT('Ctrl Pts',(-1.19566418930242,1.,1.80030314369879));
#32344=CARTESIAN_POINT('Ctrl Pts',(-1.18996997934445,-1.,1.79740245923478));
#32345=CARTESIAN_POINT('Ctrl Pts',(-1.18996997934445,1.,1.79740245923478));
#32346=CARTESIAN_POINT('Ctrl Pts',(-1.18430321697432,-1.,1.79447240321515));
#32347=CARTESIAN_POINT('Ctrl Pts',(-1.18430321697432,1.,1.79447240321515));
#32348=CARTESIAN_POINT('Ctrl Pts',(-1.17866429440809,-1.,1.79151291552689));
#32349=CARTESIAN_POINT('Ctrl Pts',(-1.17866429440809,1.,1.79151291552689));
#32350=CARTESIAN_POINT('Ctrl Pts',(-1.17305363177328,-1.,1.78852398877616));
#32351=CARTESIAN_POINT('Ctrl Pts',(-1.17305363177328,1.,1.78852398877616));
#32352=CARTESIAN_POINT('Ctrl Pts',(-1.16747166312303,-1.,1.78550566040443));
#32353=CARTESIAN_POINT('Ctrl Pts',(-1.16747166312303,1.,1.78550566040443));
#32354=CARTESIAN_POINT('Ctrl Pts',(-1.16191881298499,-1.,1.78245795881009));
#32355=CARTESIAN_POINT('Ctrl Pts',(-1.16191881298499,1.,1.78245795881009));
#32356=CARTESIAN_POINT('Ctrl Pts',(-1.15639547194698,-1.,1.77938085564275));
#32357=CARTESIAN_POINT('Ctrl Pts',(-1.15639547194698,1.,1.77938085564275));
#32358=CARTESIAN_POINT('Ctrl Pts',(-1.15090197841515,-1.,1.7762742255701));
#32359=CARTESIAN_POINT('Ctrl Pts',(-1.15090197841515,1.,1.7762742255701));
#32360=CARTESIAN_POINT('Ctrl Pts',(-1.1454385822692,-1.,1.77313777896194));
#32361=CARTESIAN_POINT('Ctrl Pts',(-1.1454385822692,1.,1.77313777896194));
#32362=CARTESIAN_POINT('Ctrl Pts',(-1.14000548336975,-1.,1.76997111386769));
#32363=CARTESIAN_POINT('Ctrl Pts',(-1.14000548336975,1.,1.76997111386769));
#32364=CARTESIAN_POINT('Ctrl Pts',(-1.1346029180462,-1.,1.76677384551862));
#32365=CARTESIAN_POINT('Ctrl Pts',(-1.1346029180462,1.,1.76677384551862));
#32366=CARTESIAN_POINT('Ctrl Pts',(-1.12923123555075,-1.,1.7635457196617));
#32367=CARTESIAN_POINT('Ctrl Pts',(-1.12923123555075,1.,1.7635457196617));
#32368=CARTESIAN_POINT('Ctrl Pts',(-1.12389096855086,-1.,1.76028671825096));
#32369=CARTESIAN_POINT('Ctrl Pts',(-1.12389096855086,1.,1.76028671825096));
#32370=CARTESIAN_POINT('Ctrl Pts',(-1.11858293216763,-1.,1.75699720772105));
#32371=CARTESIAN_POINT('Ctrl Pts',(-1.11858293216763,1.,1.75699720772105));
#32372=CARTESIAN_POINT('Ctrl Pts',(-1.11330807582551,-1.,1.7536777209463));
#32373=CARTESIAN_POINT('Ctrl Pts',(-1.11330807582551,1.,1.7536777209463));
#32374=CARTESIAN_POINT('Ctrl Pts',(-1.10806728183007,-1.,1.7503286607592));
#32375=CARTESIAN_POINT('Ctrl Pts',(-1.10806728183007,1.,1.7503286607592));
#32376=CARTESIAN_POINT('Ctrl Pts',(-1.10286118991143,-1.,1.74695004214923));
#32377=CARTESIAN_POINT('Ctrl Pts',(-1.10286118991143,1.,1.74695004214923));
#32378=CARTESIAN_POINT('Ctrl Pts',(-1.09768999241225,-1.,1.74354119236208));
#32379=CARTESIAN_POINT('Ctrl Pts',(-1.09768999241225,1.,1.74354119236208));
#32380=CARTESIAN_POINT('Ctrl Pts',(-1.09255329056493,-1.,1.74010053962247));
#32381=CARTESIAN_POINT('Ctrl Pts',(-1.09255329056493,1.,1.74010053962247));
#32382=CARTESIAN_POINT('Ctrl Pts',(-1.08745056285427,-1.,1.73662628326091));
#32383=CARTESIAN_POINT('Ctrl Pts',(-1.08745056285427,1.,1.73662628326091));
#32384=CARTESIAN_POINT('Ctrl Pts',(-1.08238162784749,-1.,1.73311705663407));
#32385=CARTESIAN_POINT('Ctrl Pts',(-1.08238162784749,1.,1.73311705663407));
#32386=CARTESIAN_POINT('Ctrl Pts',(-1.0773470373727,-1.,1.72957248977424));
#32387=CARTESIAN_POINT('Ctrl Pts',(-1.0773470373727,1.,1.72957248977424));
#32388=CARTESIAN_POINT('Ctrl Pts',(-1.07234866990252,-1.,1.72599406198488));
#32389=CARTESIAN_POINT('Ctrl Pts',(-1.07234866990252,1.,1.72599406198488));
#32390=CARTESIAN_POINT('Ctrl Pts',(-1.06738966975462,-1.,1.72238500928453));
#32391=CARTESIAN_POINT('Ctrl Pts',(-1.06738966975462,1.,1.72238500928453));
#32392=CARTESIAN_POINT('Ctrl Pts',(-1.06247324680647,-1.,1.71874858456904));
#32393=CARTESIAN_POINT('Ctrl Pts',(-1.06247324680647,1.,1.71874858456904));
#32394=CARTESIAN_POINT('Ctrl Pts',(-1.05760163192479,-1.,1.7150865442702));
#32395=CARTESIAN_POINT('Ctrl Pts',(-1.05760163192479,1.,1.7150865442702));
#32396=CARTESIAN_POINT('Ctrl Pts',(-1.05277517202855,-1.,1.71139783543989));
#32397=CARTESIAN_POINT('Ctrl Pts',(-1.05277517202855,1.,1.71139783543989));
#32398=CARTESIAN_POINT('Ctrl Pts',(-1.04799085404995,-1.,1.70767646263649));
#32399=CARTESIAN_POINT('Ctrl Pts',(-1.04799085404995,1.,1.70767646263649));
#32400=CARTESIAN_POINT('Ctrl Pts',(-1.04324363334554,-1.,1.70391338707982));
#32401=CARTESIAN_POINT('Ctrl Pts',(-1.04324363334554,1.,1.70391338707982));
#32402=CARTESIAN_POINT('Ctrl Pts',(-1.03852922490789,-1.,1.70010052930962));
#32403=CARTESIAN_POINT('Ctrl Pts',(-1.03852922490789,1.,1.70010052930962));
#32404=CARTESIAN_POINT('Ctrl Pts',(-1.03384646003588,-1.,1.69623414782771));
#32405=CARTESIAN_POINT('Ctrl Pts',(-1.03384646003588,1.,1.69623414782771));
#32406=CARTESIAN_POINT('Ctrl Pts',(-1.02919977579147,-1.,1.69231840863458));
#32407=CARTESIAN_POINT('Ctrl Pts',(-1.02919977579147,1.,1.69231840863458));
#32408=CARTESIAN_POINT('Ctrl Pts',(-1.02460180535255,-1.,1.68836910178447));
#32409=CARTESIAN_POINT('Ctrl Pts',(-1.02460180535255,1.,1.68836910178447));
#32410=CARTESIAN_POINT('Ctrl Pts',(-1.02006795074201,-1.,1.68440578021706));
#32411=CARTESIAN_POINT('Ctrl Pts',(-1.02006795074201,1.,1.68440578021706));
#32412=CARTESIAN_POINT('Ctrl Pts',(-1.01561026162773,-1.,1.68044289894798));
#32413=CARTESIAN_POINT('Ctrl Pts',(-1.01561026162773,1.,1.68044289894798));
#32414=CARTESIAN_POINT('Ctrl Pts',(-1.01123236493511,-1.,1.67648246776464));
#32415=CARTESIAN_POINT('Ctrl Pts',(-1.01123236493511,1.,1.67648246776464));
#32416=CARTESIAN_POINT('Ctrl Pts',(-1.00692206696414,-1.,1.67250335383293));
#32417=CARTESIAN_POINT('Ctrl Pts',(-1.00692206696414,1.,1.67250335383293));
#32418=CARTESIAN_POINT('Ctrl Pts',(-1.00265091003727,-1.,1.66846059277303));
#32419=CARTESIAN_POINT('Ctrl Pts',(-1.00265091003727,1.,1.66846059277303));
#32420=CARTESIAN_POINT('Ctrl Pts',(-0.998389654952758,-1.,1.66430758030376));
#32421=CARTESIAN_POINT('Ctrl Pts',(-0.998389654952758,1.,1.66430758030376));
#32422=CARTESIAN_POINT('Ctrl Pts',(-0.994121836661306,-1.,1.66001553809947));
#32423=CARTESIAN_POINT('Ctrl Pts',(-0.994121836661306,1.,1.66001553809947));
#32424=CARTESIAN_POINT('Ctrl Pts',(-0.989855627854165,-1.,1.65559044289699));
#32425=CARTESIAN_POINT('Ctrl Pts',(-0.989855627854165,1.,1.65559044289699));
#32426=CARTESIAN_POINT('Ctrl Pts',(-0.985642622920821,-1.,1.65110016612638));
#32427=CARTESIAN_POINT('Ctrl Pts',(-0.985642622920821,1.,1.65110016612638));
#32428=CARTESIAN_POINT('Ctrl Pts',(-0.981562530939489,-1.,1.64665139190656));
#32429=CARTESIAN_POINT('Ctrl Pts',(-0.981562530939489,1.,1.64665139190656));
#32430=CARTESIAN_POINT('Ctrl Pts',(-0.977689794119416,-1.,1.64233990826687));
#32431=CARTESIAN_POINT('Ctrl Pts',(-0.977689794119416,1.,1.64233990826687));
#32432=CARTESIAN_POINT('Ctrl Pts',(-0.974066058287418,-1.,1.63820952658144));
#32433=CARTESIAN_POINT('Ctrl Pts',(-0.974066058287418,1.,1.63820952658144));
#32434=CARTESIAN_POINT('Ctrl Pts',(-0.970669715997509,-1.,1.63420665729798));
#32435=CARTESIAN_POINT('Ctrl Pts',(-0.970669715997509,1.,1.63420665729798));
#32436=CARTESIAN_POINT('Ctrl Pts',(-0.967387853230345,-1.,1.63013849959461));
#32437=CARTESIAN_POINT('Ctrl Pts',(-0.967387853230345,1.,1.63013849959461));
#32438=CARTESIAN_POINT('Ctrl Pts',(-0.964046107040536,-1.,1.62571930670187));
#32439=CARTESIAN_POINT('Ctrl Pts',(-0.964046107040536,1.,1.62571930670187));
#32440=CARTESIAN_POINT('Ctrl Pts',(-0.960438326101729,-1.,1.62061638140221));
#32441=CARTESIAN_POINT('Ctrl Pts',(-0.960438326101729,1.,1.62061638140221));
#32442=CARTESIAN_POINT('Ctrl Pts',(-0.956354422920671,-1.,1.61449324337085));
#32443=CARTESIAN_POINT('Ctrl Pts',(-0.956354422920671,1.,1.61449324337085));
#32444=CARTESIAN_POINT('Ctrl Pts',(-0.951613284356035,-1.,1.60706069896936));
#32445=CARTESIAN_POINT('Ctrl Pts',(-0.951613284356035,1.,1.60706069896936));
#32446=CARTESIAN_POINT('Ctrl Pts',(-0.946078063315257,-1.,1.59810042043673));
#32447=CARTESIAN_POINT('Ctrl Pts',(-0.946078063315257,1.,1.59810042043673));
#32448=CARTESIAN_POINT('Ctrl Pts',(-0.939646377893399,-1.,1.58744937487176));
#32449=CARTESIAN_POINT('Ctrl Pts',(-0.939646377893399,1.,1.58744937487176));
#32450=CARTESIAN_POINT('Ctrl Pts',(-0.932246680108685,-1.,1.57499388382243));
#32451=CARTESIAN_POINT('Ctrl Pts',(-0.932246680108685,1.,1.57499388382243));
#32452=CARTESIAN_POINT('Ctrl Pts',(-0.923832188944341,-1.,1.56065988578893));
#32453=CARTESIAN_POINT('Ctrl Pts',(-0.923832188944341,1.,1.56065988578893));
#32454=CARTESIAN_POINT('Ctrl Pts',(-0.914375919026456,-1.,1.54440491149498));
#32455=CARTESIAN_POINT('Ctrl Pts',(-0.914375919026456,1.,1.54440491149498));
#32456=CARTESIAN_POINT('Ctrl Pts',(-0.905967409625651,-1.,1.52984849887993));
#32457=CARTESIAN_POINT('Ctrl Pts',(-0.905967409625651,1.,1.52984849887993));
#32458=CARTESIAN_POINT('Ctrl Pts',(-0.899185047483511,-1.,1.51805569590094));
#32459=CARTESIAN_POINT('Ctrl Pts',(-0.899185047483511,1.,1.51805569590094));
#32460=CARTESIAN_POINT('Ctrl Pts',(-0.894452006964543,-1.,1.50980486806688));
#32461=CARTESIAN_POINT('Ctrl Pts',(-0.894452006964543,1.,1.50980486806688));
#32462=CARTESIAN_POINT('Ctrl Pts',(-0.892032620296855,-1.,1.5055822144029));
#32463=CARTESIAN_POINT('Ctrl Pts',(-0.892032620296855,1.,1.5055822144029));
#32464=CARTESIAN_POINT('',(-1.23627494547115,1.,1.81978687191668));
#32465=CARTESIAN_POINT('Ctrl Pts',(-1.23627494547115,1.,1.81978687191668));
#32466=CARTESIAN_POINT('Ctrl Pts',(-1.23509651170476,1.,1.81925017193666));
#32467=CARTESIAN_POINT('Ctrl Pts',(-1.2327422452705,1.,1.81817389921279));
#32468=CARTESIAN_POINT('Ctrl Pts',(-1.2292186489137,1.,1.8165508718364));
#32469=CARTESIAN_POINT('Ctrl Pts',(-1.2245361330495,1.,1.81436959210434));
#32470=CARTESIAN_POINT('Ctrl Pts',(-1.21870906103557,1.,1.81161420806656));
#32471=CARTESIAN_POINT('Ctrl Pts',(-1.21290815708314,1.,1.80882996917129));
#32472=CARTESIAN_POINT('Ctrl Pts',(-1.20713356605475,1.,1.80601678480707));
#32473=CARTESIAN_POINT('Ctrl Pts',(-1.20138548938974,1.,1.80317454838603));
#32474=CARTESIAN_POINT('Ctrl Pts',(-1.19566418930242,1.,1.80030314369879));
#32475=CARTESIAN_POINT('Ctrl Pts',(-1.18996997934445,1.,1.79740245923478));
#32476=CARTESIAN_POINT('Ctrl Pts',(-1.18430321697432,1.,1.79447240321515));
#32477=CARTESIAN_POINT('Ctrl Pts',(-1.17866429440809,1.,1.79151291552689));
#32478=CARTESIAN_POINT('Ctrl Pts',(-1.17305363177328,1.,1.78852398877616));
#32479=CARTESIAN_POINT('Ctrl Pts',(-1.16747166312303,1.,1.78550566040443));
#32480=CARTESIAN_POINT('Ctrl Pts',(-1.16191881298499,1.,1.78245795881009));
#32481=CARTESIAN_POINT('Ctrl Pts',(-1.15639547194698,1.,1.77938085564275));
#32482=CARTESIAN_POINT('Ctrl Pts',(-1.15090197841515,1.,1.7762742255701));
#32483=CARTESIAN_POINT('Ctrl Pts',(-1.1454385822692,1.,1.77313777896194));
#32484=CARTESIAN_POINT('Ctrl Pts',(-1.14000548336975,1.,1.76997111386769));
#32485=CARTESIAN_POINT('Ctrl Pts',(-1.1346029180462,1.,1.76677384551862));
#32486=CARTESIAN_POINT('Ctrl Pts',(-1.12923123555075,1.,1.7635457196617));
#32487=CARTESIAN_POINT('Ctrl Pts',(-1.12389096855086,1.,1.76028671825096));
#32488=CARTESIAN_POINT('Ctrl Pts',(-1.11858293216763,1.,1.75699720772105));
#32489=CARTESIAN_POINT('Ctrl Pts',(-1.11330807582551,1.,1.7536777209463));
#32490=CARTESIAN_POINT('Ctrl Pts',(-1.10806728183007,1.,1.7503286607592));
#32491=CARTESIAN_POINT('Ctrl Pts',(-1.10286118991143,1.,1.74695004214923));
#32492=CARTESIAN_POINT('Ctrl Pts',(-1.09768999241225,1.,1.74354119236208));
#32493=CARTESIAN_POINT('Ctrl Pts',(-1.09255329056493,1.,1.74010053962247));
#32494=CARTESIAN_POINT('Ctrl Pts',(-1.08745056285427,1.,1.73662628326091));
#32495=CARTESIAN_POINT('Ctrl Pts',(-1.08238162784749,1.,1.73311705663407));
#32496=CARTESIAN_POINT('Ctrl Pts',(-1.0773470373727,1.,1.72957248977424));
#32497=CARTESIAN_POINT('Ctrl Pts',(-1.07234866990252,1.,1.72599406198488));
#32498=CARTESIAN_POINT('Ctrl Pts',(-1.06738966975462,1.,1.72238500928453));
#32499=CARTESIAN_POINT('Ctrl Pts',(-1.06247324680647,1.,1.71874858456904));
#32500=CARTESIAN_POINT('Ctrl Pts',(-1.05760163192479,1.,1.7150865442702));
#32501=CARTESIAN_POINT('Ctrl Pts',(-1.05277517202855,1.,1.71139783543989));
#32502=CARTESIAN_POINT('Ctrl Pts',(-1.04799085404995,1.,1.70767646263649));
#32503=CARTESIAN_POINT('Ctrl Pts',(-1.04324363334554,1.,1.70391338707982));
#32504=CARTESIAN_POINT('Ctrl Pts',(-1.03852922490789,1.,1.70010052930962));
#32505=CARTESIAN_POINT('Ctrl Pts',(-1.03384646003588,1.,1.69623414782771));
#32506=CARTESIAN_POINT('Ctrl Pts',(-1.02919977579147,1.,1.69231840863458));
#32507=CARTESIAN_POINT('Ctrl Pts',(-1.02460180535255,1.,1.68836910178447));
#32508=CARTESIAN_POINT('Ctrl Pts',(-1.02006795074201,1.,1.68440578021706));
#32509=CARTESIAN_POINT('Ctrl Pts',(-1.01561026162773,1.,1.68044289894798));
#32510=CARTESIAN_POINT('Ctrl Pts',(-1.01123236493511,1.,1.67648246776464));
#32511=CARTESIAN_POINT('Ctrl Pts',(-1.00692206696414,1.,1.67250335383293));
#32512=CARTESIAN_POINT('Ctrl Pts',(-1.00265091003727,1.,1.66846059277303));
#32513=CARTESIAN_POINT('Ctrl Pts',(-0.998389654952758,1.,1.66430758030376));
#32514=CARTESIAN_POINT('Ctrl Pts',(-0.994121836661306,1.,1.66001553809947));
#32515=CARTESIAN_POINT('Ctrl Pts',(-0.989855627854165,1.,1.65559044289699));
#32516=CARTESIAN_POINT('Ctrl Pts',(-0.985642622920821,1.,1.65110016612638));
#32517=CARTESIAN_POINT('Ctrl Pts',(-0.981562530939489,1.,1.64665139190656));
#32518=CARTESIAN_POINT('Ctrl Pts',(-0.977689794119416,1.,1.64233990826687));
#32519=CARTESIAN_POINT('Ctrl Pts',(-0.974066058287418,1.,1.63820952658144));
#32520=CARTESIAN_POINT('Ctrl Pts',(-0.970669715997509,1.,1.63420665729798));
#32521=CARTESIAN_POINT('Ctrl Pts',(-0.967387853230345,1.,1.63013849959461));
#32522=CARTESIAN_POINT('Ctrl Pts',(-0.964046107040536,1.,1.62571930670187));
#32523=CARTESIAN_POINT('Ctrl Pts',(-0.960438326101729,1.,1.62061638140221));
#32524=CARTESIAN_POINT('Ctrl Pts',(-0.956354422920671,1.,1.61449324337085));
#32525=CARTESIAN_POINT('Ctrl Pts',(-0.951613284356035,1.,1.60706069896936));
#32526=CARTESIAN_POINT('Ctrl Pts',(-0.946078063315257,1.,1.59810042043673));
#32527=CARTESIAN_POINT('Ctrl Pts',(-0.939646377893399,1.,1.58744937487176));
#32528=CARTESIAN_POINT('Ctrl Pts',(-0.932246680108685,1.,1.57499388382243));
#32529=CARTESIAN_POINT('Ctrl Pts',(-0.923832188944341,1.,1.56065988578893));
#32530=CARTESIAN_POINT('Ctrl Pts',(-0.914375919026456,1.,1.54440491149498));
#32531=CARTESIAN_POINT('Ctrl Pts',(-0.905967409625651,1.,1.52984849887993));
#32532=CARTESIAN_POINT('Ctrl Pts',(-0.899185047483511,1.,1.51805569590094));
#32533=CARTESIAN_POINT('Ctrl Pts',(-0.894452006964543,1.,1.50980486806688));
#32534=CARTESIAN_POINT('Ctrl Pts',(-0.892032620296855,1.,1.5055822144029));
#32535=CARTESIAN_POINT('',(-1.23627494547115,0.,1.81978687191668));
#32536=CARTESIAN_POINT('Origin',(-1.34869019493419,0.,1.73811241238545));
#32537=CARTESIAN_POINT('',(-1.34869019493419,1.,1.73811241238545));
#32538=CARTESIAN_POINT('',(-1.23627494547115,1.,1.81978687191668));
#32539=CARTESIAN_POINT('',(-1.34869019493419,0.,1.73811241238545));
#32540=CARTESIAN_POINT('Ctrl Pts',(-1.15624053661742,-1.,1.31362392696032));
#32541=CARTESIAN_POINT('Ctrl Pts',(-1.15624053661742,1.,1.31362392696032));
#32542=CARTESIAN_POINT('Ctrl Pts',(-1.15950888730809,-1.,1.31722977216397));
#32543=CARTESIAN_POINT('Ctrl Pts',(-1.15950888730809,1.,1.31722977216397));
#32544=CARTESIAN_POINT('Ctrl Pts',(-1.16589330093588,-1.,1.32428080721772));
#32545=CARTESIAN_POINT('Ctrl Pts',(-1.16589330093588,1.,1.32428080721772));
#32546=CARTESIAN_POINT('Ctrl Pts',(-1.17501305789857,-1.,1.33437539347008));
#32547=CARTESIAN_POINT('Ctrl Pts',(-1.17501305789857,1.,1.33437539347008));
#32548=CARTESIAN_POINT('Ctrl Pts',(-1.18625865667441,-1.,1.34687054001093));
#32549=CARTESIAN_POINT('Ctrl Pts',(-1.18625865667441,1.,1.34687054001093));
#32550=CARTESIAN_POINT('Ctrl Pts',(-1.1987959077932,-1.,1.36088705043885));
#32551=CARTESIAN_POINT('Ctrl Pts',(-1.1987959077932,1.,1.36088705043885));
#32552=CARTESIAN_POINT('Ctrl Pts',(-1.20982812925645,-1.,1.37331915607905));
#32553=CARTESIAN_POINT('Ctrl Pts',(-1.20982812925645,1.,1.37331915607905));
#32554=CARTESIAN_POINT('Ctrl Pts',(-1.21938737280852,-1.,1.38420564527715));
#32555=CARTESIAN_POINT('Ctrl Pts',(-1.21938737280852,1.,1.38420564527715));
#32556=CARTESIAN_POINT('Ctrl Pts',(-1.22752961899387,-1.,1.39361389568796));
#32557=CARTESIAN_POINT('Ctrl Pts',(-1.22752961899387,1.,1.39361389568796));
#32558=CARTESIAN_POINT('Ctrl Pts',(-1.23434087290423,-1.,1.40164708206106));
#32559=CARTESIAN_POINT('Ctrl Pts',(-1.23434087290423,1.,1.40164708206106));
#32560=CARTESIAN_POINT('Ctrl Pts',(-1.23994455029534,-1.,1.40845295531283));
#32561=CARTESIAN_POINT('Ctrl Pts',(-1.23994455029534,1.,1.40845295531283));
#32562=CARTESIAN_POINT('Ctrl Pts',(-1.24450600513056,-1.,1.41422913175179));
#32563=CARTESIAN_POINT('Ctrl Pts',(-1.24450600513056,1.,1.41422913175179));
#32564=CARTESIAN_POINT('Ctrl Pts',(-1.24824430986571,-1.,1.41923722596025));
#32565=CARTESIAN_POINT('Ctrl Pts',(-1.24824430986571,1.,1.41923722596025));
#32566=CARTESIAN_POINT('Ctrl Pts',(-1.2514145557001,-1.,1.42378102115575));
#32567=CARTESIAN_POINT('Ctrl Pts',(-1.2514145557001,1.,1.42378102115575));
#32568=CARTESIAN_POINT('Ctrl Pts',(-1.25426945222639,-1.,1.42815938799387));
#32569=CARTESIAN_POINT('Ctrl Pts',(-1.25426945222639,1.,1.42815938799387));
#32570=CARTESIAN_POINT('Ctrl Pts',(-1.25702687965755,-1.,1.43262645609691));
#32571=CARTESIAN_POINT('Ctrl Pts',(-1.25702687965755,1.,1.43262645609691));
#32572=CARTESIAN_POINT('Ctrl Pts',(-1.25983531012005,-1.,1.43734919180848));
#32573=CARTESIAN_POINT('Ctrl Pts',(-1.25983531012005,1.,1.43734919180848));
#32574=CARTESIAN_POINT('Ctrl Pts',(-1.26273903323859,-1.,1.44236470511303));
#32575=CARTESIAN_POINT('Ctrl Pts',(-1.26273903323859,1.,1.44236470511303));
#32576=CARTESIAN_POINT('Ctrl Pts',(-1.26570925118868,-1.,1.44761985001662));
#32577=CARTESIAN_POINT('Ctrl Pts',(-1.26570925118868,1.,1.44761985001662));
#32578=CARTESIAN_POINT('Ctrl Pts',(-1.2686778680489,-1.,1.45301422764247));
#32579=CARTESIAN_POINT('Ctrl Pts',(-1.2686778680489,1.,1.45301422764247));
#32580=CARTESIAN_POINT('Ctrl Pts',(-1.27156805265289,-1.,1.45843906294697));
#32581=CARTESIAN_POINT('Ctrl Pts',(-1.27156805265289,1.,1.45843906294697));
#32582=CARTESIAN_POINT('Ctrl Pts',(-1.27433119897822,-1.,1.46382431332476));
#32583=CARTESIAN_POINT('Ctrl Pts',(-1.27433119897822,1.,1.46382431332476));
#32584=CARTESIAN_POINT('Ctrl Pts',(-1.27696414831089,-1.,1.46916035917133));
#32585=CARTESIAN_POINT('Ctrl Pts',(-1.27696414831089,1.,1.46916035917133));
#32586=CARTESIAN_POINT('Ctrl Pts',(-1.2794891824849,-1.,1.4744717526707));
#32587=CARTESIAN_POINT('Ctrl Pts',(-1.2794891824849,1.,1.4744717526707));
#32588=CARTESIAN_POINT('Ctrl Pts',(-1.28194158939517,-1.,1.47980070347095));
#32589=CARTESIAN_POINT('Ctrl Pts',(-1.28194158939517,1.,1.47980070347095));
#32590=CARTESIAN_POINT('Ctrl Pts',(-1.28435533880201,-1.,1.4851881711891));
#32591=CARTESIAN_POINT('Ctrl Pts',(-1.28435533880201,1.,1.4851881711891));
#32592=CARTESIAN_POINT('Ctrl Pts',(-1.2867467611644,-1.,1.4906522831278));
#32593=CARTESIAN_POINT('Ctrl Pts',(-1.2867467611644,1.,1.4906522831278));
#32594=CARTESIAN_POINT('Ctrl Pts',(-1.28911506584254,-1.,1.49618896881754));
#32595=CARTESIAN_POINT('Ctrl Pts',(-1.28911506584254,1.,1.49618896881754));
#32596=CARTESIAN_POINT('Ctrl Pts',(-1.29145022885181,-1.,1.50178230149776));
#32597=CARTESIAN_POINT('Ctrl Pts',(-1.29145022885181,1.,1.50178230149776));
#32598=CARTESIAN_POINT('Ctrl Pts',(-1.29373841372842,-1.,1.50741159078365));
#32599=CARTESIAN_POINT('Ctrl Pts',(-1.29373841372842,1.,1.50741159078365));
#32600=CARTESIAN_POINT('Ctrl Pts',(-1.29596850710509,-1.,1.51305994241402));
#32601=CARTESIAN_POINT('Ctrl Pts',(-1.29596850710509,1.,1.51305994241402));
#32602=CARTESIAN_POINT('Ctrl Pts',(-1.29813791800747,-1.,1.51872184912724));
#32603=CARTESIAN_POINT('Ctrl Pts',(-1.29813791800747,1.,1.51872184912724));
#32604=CARTESIAN_POINT('Ctrl Pts',(-1.30024984366328,-1.,1.52439957861062));
#32605=CARTESIAN_POINT('Ctrl Pts',(-1.30024984366328,1.,1.52439957861062));
#32606=CARTESIAN_POINT('Ctrl Pts',(-1.30231064395568,-1.,1.53009970283891));
#32607=CARTESIAN_POINT('Ctrl Pts',(-1.30231064395568,1.,1.53009970283891));
#32608=CARTESIAN_POINT('Ctrl Pts',(-1.30432735639489,-1.,1.53582981268977));
#32609=CARTESIAN_POINT('Ctrl Pts',(-1.30432735639489,1.,1.53582981268977));
#32610=CARTESIAN_POINT('Ctrl Pts',(-1.30630475189556,-1.,1.54159462645432));
#32611=CARTESIAN_POINT('Ctrl Pts',(-1.30630475189556,1.,1.54159462645432));
#32612=CARTESIAN_POINT('Ctrl Pts',(-1.30824393907473,-1.,1.54739413957185));
#32613=CARTESIAN_POINT('Ctrl Pts',(-1.30824393907473,1.,1.54739413957185));
#32614=CARTESIAN_POINT('Ctrl Pts',(-1.31014393684222,-1.,1.55322568759481));
#32615=CARTESIAN_POINT('Ctrl Pts',(-1.31014393684222,1.,1.55322568759481));
#32616=CARTESIAN_POINT('Ctrl Pts',(-1.31200264341696,-1.,1.55908521254821));
#32617=CARTESIAN_POINT('Ctrl Pts',(-1.31200264341696,1.,1.55908521254821));
#32618=CARTESIAN_POINT('Ctrl Pts',(-1.31381795281002,-1.,1.56496872402353));
#32619=CARTESIAN_POINT('Ctrl Pts',(-1.31381795281002,1.,1.56496872402353));
#32620=CARTESIAN_POINT('Ctrl Pts',(-1.31558903860016,-1.,1.57087397835723));
#32621=CARTESIAN_POINT('Ctrl Pts',(-1.31558903860016,1.,1.57087397835723));
#32622=CARTESIAN_POINT('Ctrl Pts',(-1.31731642317187,-1.,1.5768005650559));
#32623=CARTESIAN_POINT('Ctrl Pts',(-1.31731642317187,1.,1.5768005650559));
#32624=CARTESIAN_POINT('Ctrl Pts',(-1.31900135021432,-1.,1.58274907898834));
#32625=CARTESIAN_POINT('Ctrl Pts',(-1.31900135021432,1.,1.58274907898834));
#32626=CARTESIAN_POINT('Ctrl Pts',(-1.32064537110892,-1.,1.58872057258245));
#32627=CARTESIAN_POINT('Ctrl Pts',(-1.32064537110892,1.,1.58872057258245));
#32628=CARTESIAN_POINT('Ctrl Pts',(-1.32224985747682,-1.,1.59471591079403));
#32629=CARTESIAN_POINT('Ctrl Pts',(-1.32224985747682,1.,1.59471591079403));
#32630=CARTESIAN_POINT('Ctrl Pts',(-1.32381550858256,-1.,1.60073511858687));
#32631=CARTESIAN_POINT('Ctrl Pts',(-1.32381550858256,1.,1.60073511858687));
#32632=CARTESIAN_POINT('Ctrl Pts',(-1.32534250785782,-1.,1.60677758290954));
#32633=CARTESIAN_POINT('Ctrl Pts',(-1.32534250785782,1.,1.60677758290954));
#32634=CARTESIAN_POINT('Ctrl Pts',(-1.32683074483356,-1.,1.6128423401575));
#32635=CARTESIAN_POINT('Ctrl Pts',(-1.32683074483356,1.,1.6128423401575));
#32636=CARTESIAN_POINT('Ctrl Pts',(-1.32828000610449,-1.,1.61892832270724));
#32637=CARTESIAN_POINT('Ctrl Pts',(-1.32828000610449,1.,1.61892832270724));
#32638=CARTESIAN_POINT('Ctrl Pts',(-1.3296901950568,-1.,1.62503464209797));
#32639=CARTESIAN_POINT('Ctrl Pts',(-1.3296901950568,1.,1.62503464209797));
#32640=CARTESIAN_POINT('Ctrl Pts',(-1.33106149345645,-1.,1.63116079730923));
#32641=CARTESIAN_POINT('Ctrl Pts',(-1.33106149345645,1.,1.63116079730923));
#32642=CARTESIAN_POINT('Ctrl Pts',(-1.33239425103724,-1.,1.63730653475089));
#32643=CARTESIAN_POINT('Ctrl Pts',(-1.33239425103724,1.,1.63730653475089));
#32644=CARTESIAN_POINT('Ctrl Pts',(-1.33368890676572,-1.,1.6434717485603));
#32645=CARTESIAN_POINT('Ctrl Pts',(-1.33368890676572,1.,1.6434717485603));
#32646=CARTESIAN_POINT('Ctrl Pts',(-1.33494590467993,-1.,1.6496563728683));
#32647=CARTESIAN_POINT('Ctrl Pts',(-1.33494590467993,1.,1.6496563728683));
#32648=CARTESIAN_POINT('Ctrl Pts',(-1.33616559745172,-1.,1.65586025952593));
#32649=CARTESIAN_POINT('Ctrl Pts',(-1.33616559745172,1.,1.65586025952593));
#32650=CARTESIAN_POINT('Ctrl Pts',(-1.33734820885262,-1.,1.66208312541983));
#32651=CARTESIAN_POINT('Ctrl Pts',(-1.33734820885262,1.,1.66208312541983));
#32652=CARTESIAN_POINT('Ctrl Pts',(-1.33849388654388,-1.,1.66832460783989));
#32653=CARTESIAN_POINT('Ctrl Pts',(-1.33849388654388,1.,1.66832460783989));
#32654=CARTESIAN_POINT('Ctrl Pts',(-1.3396027347034,-1.,1.67458429426086));
#32655=CARTESIAN_POINT('Ctrl Pts',(-1.3396027347034,1.,1.67458429426086));
#32656=CARTESIAN_POINT('Ctrl Pts',(-1.34067485185203,-1.,1.68086176030362));
#32657=CARTESIAN_POINT('Ctrl Pts',(-1.34067485185203,1.,1.68086176030362));
#32658=CARTESIAN_POINT('Ctrl Pts',(-1.341710374848,-1.,1.68715660868764));
#32659=CARTESIAN_POINT('Ctrl Pts',(-1.341710374848,1.,1.68715660868764));
#32660=CARTESIAN_POINT('Ctrl Pts',(-1.34270948206319,-1.,1.6934684849687));
#32661=CARTESIAN_POINT('Ctrl Pts',(-1.34270948206319,1.,1.6934684849687));
#32662=CARTESIAN_POINT('Ctrl Pts',(-1.34367237124483,-1.,1.69979707754427));
#32663=CARTESIAN_POINT('Ctrl Pts',(-1.34367237124483,1.,1.69979707754427));
#32664=CARTESIAN_POINT('Ctrl Pts',(-1.34459924533831,-1.,1.70614212266738));
#32665=CARTESIAN_POINT('Ctrl Pts',(-1.34459924533831,1.,1.70614212266738));
#32666=CARTESIAN_POINT('Ctrl Pts',(-1.34549029589416,-1.,1.71250340686822));
#32667=CARTESIAN_POINT('Ctrl Pts',(-1.34549029589416,1.,1.71250340686822));
#32668=CARTESIAN_POINT('Ctrl Pts',(-1.34634568653227,-1.,1.7188807715049));
#32669=CARTESIAN_POINT('Ctrl Pts',(-1.34634568653227,1.,1.7188807715049));
#32670=CARTESIAN_POINT('Ctrl Pts',(-1.34716554819527,-1.,1.72527410680674));
#32671=CARTESIAN_POINT('Ctrl Pts',(-1.34716554819527,1.,1.72527410680674));
#32672=CARTESIAN_POINT('Ctrl Pts',(-1.34779309152035,-1.,1.7304014965394));
#32673=CARTESIAN_POINT('Ctrl Pts',(-1.34779309152035,1.,1.7304014965394));
#32674=CARTESIAN_POINT('Ctrl Pts',(-1.34824783112887,-1.,1.73425417885907));
#32675=CARTESIAN_POINT('Ctrl Pts',(-1.34824783112887,1.,1.73425417885907));
#32676=CARTESIAN_POINT('Ctrl Pts',(-1.34854391898045,-1.,1.73682580585691));
#32677=CARTESIAN_POINT('Ctrl Pts',(-1.34854391898045,1.,1.73682580585691));
#32678=CARTESIAN_POINT('Ctrl Pts',(-1.34869019493419,-1.,1.73811241238545));
#32679=CARTESIAN_POINT('Ctrl Pts',(-1.34869019493419,1.,1.73811241238545));
#32680=CARTESIAN_POINT('',(-1.15624053661742,1.,1.31362392696032));
#32681=CARTESIAN_POINT('Ctrl Pts',(-1.15624053661742,1.,1.31362392696032));
#32682=CARTESIAN_POINT('Ctrl Pts',(-1.15950888730809,1.,1.31722977216397));
#32683=CARTESIAN_POINT('Ctrl Pts',(-1.16589330093588,1.,1.32428080721772));
#32684=CARTESIAN_POINT('Ctrl Pts',(-1.17501305789857,1.,1.33437539347008));
#32685=CARTESIAN_POINT('Ctrl Pts',(-1.18625865667441,1.,1.34687054001093));
#32686=CARTESIAN_POINT('Ctrl Pts',(-1.1987959077932,1.,1.36088705043885));
#32687=CARTESIAN_POINT('Ctrl Pts',(-1.20982812925645,1.,1.37331915607905));
#32688=CARTESIAN_POINT('Ctrl Pts',(-1.21938737280852,1.,1.38420564527715));
#32689=CARTESIAN_POINT('Ctrl Pts',(-1.22752961899387,1.,1.39361389568796));
#32690=CARTESIAN_POINT('Ctrl Pts',(-1.23434087290423,1.,1.40164708206106));
#32691=CARTESIAN_POINT('Ctrl Pts',(-1.23994455029534,1.,1.40845295531283));
#32692=CARTESIAN_POINT('Ctrl Pts',(-1.24450600513056,1.,1.41422913175179));
#32693=CARTESIAN_POINT('Ctrl Pts',(-1.24824430986571,1.,1.41923722596025));
#32694=CARTESIAN_POINT('Ctrl Pts',(-1.2514145557001,1.,1.42378102115575));
#32695=CARTESIAN_POINT('Ctrl Pts',(-1.25426945222639,1.,1.42815938799387));
#32696=CARTESIAN_POINT('Ctrl Pts',(-1.25702687965755,1.,1.43262645609691));
#32697=CARTESIAN_POINT('Ctrl Pts',(-1.25983531012005,1.,1.43734919180848));
#32698=CARTESIAN_POINT('Ctrl Pts',(-1.26273903323859,1.,1.44236470511303));
#32699=CARTESIAN_POINT('Ctrl Pts',(-1.26570925118868,1.,1.44761985001662));
#32700=CARTESIAN_POINT('Ctrl Pts',(-1.2686778680489,1.,1.45301422764247));
#32701=CARTESIAN_POINT('Ctrl Pts',(-1.27156805265289,1.,1.45843906294697));
#32702=CARTESIAN_POINT('Ctrl Pts',(-1.27433119897822,1.,1.46382431332476));
#32703=CARTESIAN_POINT('Ctrl Pts',(-1.27696414831089,1.,1.46916035917133));
#32704=CARTESIAN_POINT('Ctrl Pts',(-1.2794891824849,1.,1.4744717526707));
#32705=CARTESIAN_POINT('Ctrl Pts',(-1.28194158939517,1.,1.47980070347095));
#32706=CARTESIAN_POINT('Ctrl Pts',(-1.28435533880201,1.,1.4851881711891));
#32707=CARTESIAN_POINT('Ctrl Pts',(-1.2867467611644,1.,1.4906522831278));
#32708=CARTESIAN_POINT('Ctrl Pts',(-1.28911506584254,1.,1.49618896881754));
#32709=CARTESIAN_POINT('Ctrl Pts',(-1.29145022885181,1.,1.50178230149776));
#32710=CARTESIAN_POINT('Ctrl Pts',(-1.29373841372842,1.,1.50741159078365));
#32711=CARTESIAN_POINT('Ctrl Pts',(-1.29596850710509,1.,1.51305994241402));
#32712=CARTESIAN_POINT('Ctrl Pts',(-1.29813791800747,1.,1.51872184912724));
#32713=CARTESIAN_POINT('Ctrl Pts',(-1.30024984366328,1.,1.52439957861062));
#32714=CARTESIAN_POINT('Ctrl Pts',(-1.30231064395568,1.,1.53009970283891));
#32715=CARTESIAN_POINT('Ctrl Pts',(-1.30432735639489,1.,1.53582981268977));
#32716=CARTESIAN_POINT('Ctrl Pts',(-1.30630475189556,1.,1.54159462645432));
#32717=CARTESIAN_POINT('Ctrl Pts',(-1.30824393907473,1.,1.54739413957185));
#32718=CARTESIAN_POINT('Ctrl Pts',(-1.31014393684222,1.,1.55322568759481));
#32719=CARTESIAN_POINT('Ctrl Pts',(-1.31200264341696,1.,1.55908521254821));
#32720=CARTESIAN_POINT('Ctrl Pts',(-1.31381795281002,1.,1.56496872402353));
#32721=CARTESIAN_POINT('Ctrl Pts',(-1.31558903860016,1.,1.57087397835723));
#32722=CARTESIAN_POINT('Ctrl Pts',(-1.31731642317187,1.,1.5768005650559));
#32723=CARTESIAN_POINT('Ctrl Pts',(-1.31900135021432,1.,1.58274907898834));
#32724=CARTESIAN_POINT('Ctrl Pts',(-1.32064537110892,1.,1.58872057258245));
#32725=CARTESIAN_POINT('Ctrl Pts',(-1.32224985747682,1.,1.59471591079403));
#32726=CARTESIAN_POINT('Ctrl Pts',(-1.32381550858256,1.,1.60073511858687));
#32727=CARTESIAN_POINT('Ctrl Pts',(-1.32534250785782,1.,1.60677758290954));
#32728=CARTESIAN_POINT('Ctrl Pts',(-1.32683074483356,1.,1.6128423401575));
#32729=CARTESIAN_POINT('Ctrl Pts',(-1.32828000610449,1.,1.61892832270724));
#32730=CARTESIAN_POINT('Ctrl Pts',(-1.3296901950568,1.,1.62503464209797));
#32731=CARTESIAN_POINT('Ctrl Pts',(-1.33106149345645,1.,1.63116079730923));
#32732=CARTESIAN_POINT('Ctrl Pts',(-1.33239425103724,1.,1.63730653475089));
#32733=CARTESIAN_POINT('Ctrl Pts',(-1.33368890676572,1.,1.6434717485603));
#32734=CARTESIAN_POINT('Ctrl Pts',(-1.33494590467993,1.,1.6496563728683));
#32735=CARTESIAN_POINT('Ctrl Pts',(-1.33616559745172,1.,1.65586025952593));
#32736=CARTESIAN_POINT('Ctrl Pts',(-1.33734820885262,1.,1.66208312541983));
#32737=CARTESIAN_POINT('Ctrl Pts',(-1.33849388654388,1.,1.66832460783989));
#32738=CARTESIAN_POINT('Ctrl Pts',(-1.3396027347034,1.,1.67458429426086));
#32739=CARTESIAN_POINT('Ctrl Pts',(-1.34067485185203,1.,1.68086176030362));
#32740=CARTESIAN_POINT('Ctrl Pts',(-1.341710374848,1.,1.68715660868764));
#32741=CARTESIAN_POINT('Ctrl Pts',(-1.34270948206319,1.,1.6934684849687));
#32742=CARTESIAN_POINT('Ctrl Pts',(-1.34367237124483,1.,1.69979707754427));
#32743=CARTESIAN_POINT('Ctrl Pts',(-1.34459924533831,1.,1.70614212266738));
#32744=CARTESIAN_POINT('Ctrl Pts',(-1.34549029589416,1.,1.71250340686822));
#32745=CARTESIAN_POINT('Ctrl Pts',(-1.34634568653227,1.,1.7188807715049));
#32746=CARTESIAN_POINT('Ctrl Pts',(-1.34716554819527,1.,1.72527410680674));
#32747=CARTESIAN_POINT('Ctrl Pts',(-1.34779309152035,1.,1.7304014965394));
#32748=CARTESIAN_POINT('Ctrl Pts',(-1.34824783112887,1.,1.73425417885907));
#32749=CARTESIAN_POINT('Ctrl Pts',(-1.34854391898045,1.,1.73682580585691));
#32750=CARTESIAN_POINT('Ctrl Pts',(-1.34869019493419,1.,1.73811241238545));
#32751=CARTESIAN_POINT('',(-1.15624053661742,0.,1.31362392696032));
#32752=CARTESIAN_POINT('Origin',(0.,0.,0.));
#32753=CARTESIAN_POINT('',(-1.31362392696033,1.,1.15624053661742));
#32754=CARTESIAN_POINT('Origin',(0.,1.,0.));
#32755=CARTESIAN_POINT('',(-1.31362392696033,0.,1.15624053661742));
#32756=CARTESIAN_POINT('Ctrl Pts',(-1.73811241238545,-1.,1.34869019493419));
#32757=CARTESIAN_POINT('Ctrl Pts',(-1.73811241238545,1.,1.34869019493419));
#32758=CARTESIAN_POINT('Ctrl Pts',(-1.73682580585819,-1.,1.34854391898145));
#32759=CARTESIAN_POINT('Ctrl Pts',(-1.73682580585819,1.,1.34854391898145));
#32760=CARTESIAN_POINT('Ctrl Pts',(-1.73425417886255,-1.,1.34824783113158));
#32761=CARTESIAN_POINT('Ctrl Pts',(-1.73425417886255,1.,1.34824783113158));
#32762=CARTESIAN_POINT('Ctrl Pts',(-1.73040149654497,-1.,1.3477930915247));
#32763=CARTESIAN_POINT('Ctrl Pts',(-1.73040149654497,1.,1.3477930915247));
#32764=CARTESIAN_POINT('Ctrl Pts',(-1.72527410681298,-1.,1.34716554820013));
#32765=CARTESIAN_POINT('Ctrl Pts',(-1.72527410681298,1.,1.34716554820013));
#32766=CARTESIAN_POINT('Ctrl Pts',(-1.7188807715095,-1.,1.34634568653586));
#32767=CARTESIAN_POINT('Ctrl Pts',(-1.7188807715095,1.,1.34634568653586));
#32768=CARTESIAN_POINT('Ctrl Pts',(-1.71250340687011,-1.,1.34549029589563));
#32769=CARTESIAN_POINT('Ctrl Pts',(-1.71250340687011,1.,1.34549029589563));
#32770=CARTESIAN_POINT('Ctrl Pts',(-1.70614212266676,-1.,1.34459924533783));
#32771=CARTESIAN_POINT('Ctrl Pts',(-1.70614212266676,1.,1.34459924533783));
#32772=CARTESIAN_POINT('Ctrl Pts',(-1.69979707754221,-1.,1.34367237124322));
#32773=CARTESIAN_POINT('Ctrl Pts',(-1.69979707754221,1.,1.34367237124322));
#32774=CARTESIAN_POINT('Ctrl Pts',(-1.6934684849664,-1.,1.34270948206139));
#32775=CARTESIAN_POINT('Ctrl Pts',(-1.6934684849664,1.,1.34270948206139));
#32776=CARTESIAN_POINT('Ctrl Pts',(-1.68715660868602,-1.,1.34171037484673));
#32777=CARTESIAN_POINT('Ctrl Pts',(-1.68715660868602,1.,1.34171037484673));
#32778=CARTESIAN_POINT('Ctrl Pts',(-1.68086176030308,-1.,1.3406748518516));
#32779=CARTESIAN_POINT('Ctrl Pts',(-1.68086176030308,1.,1.3406748518516));
#32780=CARTESIAN_POINT('Ctrl Pts',(-1.67458429426126,-1.,1.33960273470372));
#32781=CARTESIAN_POINT('Ctrl Pts',(-1.67458429426126,1.,1.33960273470372));
#32782=CARTESIAN_POINT('Ctrl Pts',(-1.66832460784078,-1.,1.33849388654458));
#32783=CARTESIAN_POINT('Ctrl Pts',(-1.66832460784078,1.,1.33849388654458));
#32784=CARTESIAN_POINT('Ctrl Pts',(-1.66208312542073,-1.,1.33734820885331));
#32785=CARTESIAN_POINT('Ctrl Pts',(-1.66208312542073,1.,1.33734820885331));
#32786=CARTESIAN_POINT('Ctrl Pts',(-1.65586025952651,-1.,1.33616559745217));
#32787=CARTESIAN_POINT('Ctrl Pts',(-1.65586025952651,1.,1.33616559745217));
#32788=CARTESIAN_POINT('Ctrl Pts',(-1.64965637286843,-1.,1.33494590468003));
#32789=CARTESIAN_POINT('Ctrl Pts',(-1.64965637286843,1.,1.33494590468003));
#32790=CARTESIAN_POINT('Ctrl Pts',(-1.64347174856007,-1.,1.33368890676554));
#32791=CARTESIAN_POINT('Ctrl Pts',(-1.64347174856007,1.,1.33368890676554));
#32792=CARTESIAN_POINT('Ctrl Pts',(-1.6373065347505,-1.,1.33239425103694));
#32793=CARTESIAN_POINT('Ctrl Pts',(-1.6373065347505,1.,1.33239425103694));
#32794=CARTESIAN_POINT('Ctrl Pts',(-1.63116079730887,-1.,1.33106149345618));
#32795=CARTESIAN_POINT('Ctrl Pts',(-1.63116079730887,1.,1.33106149345618));
#32796=CARTESIAN_POINT('Ctrl Pts',(-1.62503464209777,-1.,1.32969019505665));
#32797=CARTESIAN_POINT('Ctrl Pts',(-1.62503464209777,1.,1.32969019505665));
#32798=CARTESIAN_POINT('Ctrl Pts',(-1.61892832270723,-1.,1.32828000610448));
#32799=CARTESIAN_POINT('Ctrl Pts',(-1.61892832270723,1.,1.32828000610448));
#32800=CARTESIAN_POINT('Ctrl Pts',(-1.61284234015762,-1.,1.32683074483365));
#32801=CARTESIAN_POINT('Ctrl Pts',(-1.61284234015762,1.,1.32683074483365));
#32802=CARTESIAN_POINT('Ctrl Pts',(-1.6067775829097,-1.,1.32534250785794));
#32803=CARTESIAN_POINT('Ctrl Pts',(-1.6067775829097,1.,1.32534250785794));
#32804=CARTESIAN_POINT('Ctrl Pts',(-1.600735118587,-1.,1.32381550858266));
#32805=CARTESIAN_POINT('Ctrl Pts',(-1.600735118587,1.,1.32381550858266));
#32806=CARTESIAN_POINT('Ctrl Pts',(-1.59471591079408,-1.,1.32224985747686));
#32807=CARTESIAN_POINT('Ctrl Pts',(-1.59471591079408,1.,1.32224985747686));
#32808=CARTESIAN_POINT('Ctrl Pts',(-1.58872057258244,-1.,1.32064537110891));
#32809=CARTESIAN_POINT('Ctrl Pts',(-1.58872057258244,1.,1.32064537110891));
#32810=CARTESIAN_POINT('Ctrl Pts',(-1.58274907898829,-1.,1.31900135021428));
#32811=CARTESIAN_POINT('Ctrl Pts',(-1.58274907898829,1.,1.31900135021428));
#32812=CARTESIAN_POINT('Ctrl Pts',(-1.57680056505585,-1.,1.31731642317183));
#32813=CARTESIAN_POINT('Ctrl Pts',(-1.57680056505585,1.,1.31731642317183));
#32814=CARTESIAN_POINT('Ctrl Pts',(-1.57087397835721,-1.,1.31558903860015));
#32815=CARTESIAN_POINT('Ctrl Pts',(-1.57087397835721,1.,1.31558903860015));
#32816=CARTESIAN_POINT('Ctrl Pts',(-1.56496872402352,-1.,1.31381795281002));
#32817=CARTESIAN_POINT('Ctrl Pts',(-1.56496872402352,1.,1.31381795281002));
#32818=CARTESIAN_POINT('Ctrl Pts',(-1.55908521254822,-1.,1.31200264341696));
#32819=CARTESIAN_POINT('Ctrl Pts',(-1.55908521254822,1.,1.31200264341696));
#32820=CARTESIAN_POINT('Ctrl Pts',(-1.55322568759481,-1.,1.31014393684221));
#32821=CARTESIAN_POINT('Ctrl Pts',(-1.55322568759481,1.,1.31014393684221));
#32822=CARTESIAN_POINT('Ctrl Pts',(-1.54739413957183,-1.,1.30824393907471));
#32823=CARTESIAN_POINT('Ctrl Pts',(-1.54739413957183,1.,1.30824393907471));
#32824=CARTESIAN_POINT('Ctrl Pts',(-1.54159462645428,-1.,1.30630475189553));
#32825=CARTESIAN_POINT('Ctrl Pts',(-1.54159462645428,1.,1.30630475189553));
#32826=CARTESIAN_POINT('Ctrl Pts',(-1.53582981268976,-1.,1.30432735639487));
#32827=CARTESIAN_POINT('Ctrl Pts',(-1.53582981268976,1.,1.30432735639487));
#32828=CARTESIAN_POINT('Ctrl Pts',(-1.53009970283893,-1.,1.3023106439557));
#32829=CARTESIAN_POINT('Ctrl Pts',(-1.53009970283893,1.,1.3023106439557));
#32830=CARTESIAN_POINT('Ctrl Pts',(-1.5243995786107,-1.,1.30024984366334));
#32831=CARTESIAN_POINT('Ctrl Pts',(-1.5243995786107,1.,1.30024984366334));
#32832=CARTESIAN_POINT('Ctrl Pts',(-1.51872184912735,-1.,1.29813791800757));
#32833=CARTESIAN_POINT('Ctrl Pts',(-1.51872184912735,1.,1.29813791800757));
#32834=CARTESIAN_POINT('Ctrl Pts',(-1.51305994241412,-1.,1.29596850710518));
#32835=CARTESIAN_POINT('Ctrl Pts',(-1.51305994241412,1.,1.29596850710518));
#32836=CARTESIAN_POINT('Ctrl Pts',(-1.50741159078367,-1.,1.29373841372843));
#32837=CARTESIAN_POINT('Ctrl Pts',(-1.50741159078367,1.,1.29373841372843));
#32838=CARTESIAN_POINT('Ctrl Pts',(-1.50178230149764,-1.,1.29145022885171));
#32839=CARTESIAN_POINT('Ctrl Pts',(-1.50178230149764,1.,1.29145022885171));
#32840=CARTESIAN_POINT('Ctrl Pts',(-1.49618896881729,-1.,1.28911506584232));
#32841=CARTESIAN_POINT('Ctrl Pts',(-1.49618896881729,1.,1.28911506584232));
#32842=CARTESIAN_POINT('Ctrl Pts',(-1.4906522831275,-1.,1.28674676116415));
#32843=CARTESIAN_POINT('Ctrl Pts',(-1.4906522831275,1.,1.28674676116415));
#32844=CARTESIAN_POINT('Ctrl Pts',(-1.48518817118891,-1.,1.28435533880184));
#32845=CARTESIAN_POINT('Ctrl Pts',(-1.48518817118891,1.,1.28435533880184));
#32846=CARTESIAN_POINT('Ctrl Pts',(-1.47980070347102,-1.,1.28194158939522));
#32847=CARTESIAN_POINT('Ctrl Pts',(-1.47980070347102,1.,1.28194158939522));
#32848=CARTESIAN_POINT('Ctrl Pts',(-1.4744717526711,-1.,1.27948918248524));
#32849=CARTESIAN_POINT('Ctrl Pts',(-1.4744717526711,1.,1.27948918248524));
#32850=CARTESIAN_POINT('Ctrl Pts',(-1.46916035917197,-1.,1.27696414831144));
#32851=CARTESIAN_POINT('Ctrl Pts',(-1.46916035917197,1.,1.27696414831144));
#32852=CARTESIAN_POINT('Ctrl Pts',(-1.4638243133254,-1.,1.27433119897877));
#32853=CARTESIAN_POINT('Ctrl Pts',(-1.4638243133254,1.,1.27433119897877));
#32854=CARTESIAN_POINT('Ctrl Pts',(-1.45843906294725,-1.,1.27156805265312));
#32855=CARTESIAN_POINT('Ctrl Pts',(-1.45843906294725,1.,1.27156805265312));
#32856=CARTESIAN_POINT('Ctrl Pts',(-1.45301422764205,-1.,1.26867786804854));
#32857=CARTESIAN_POINT('Ctrl Pts',(-1.45301422764205,1.,1.26867786804854));
#32858=CARTESIAN_POINT('Ctrl Pts',(-1.44761985001544,-1.,1.26570925118767));
#32859=CARTESIAN_POINT('Ctrl Pts',(-1.44761985001544,1.,1.26570925118767));
#32860=CARTESIAN_POINT('Ctrl Pts',(-1.44236470511145,-1.,1.26273903323723));
#32861=CARTESIAN_POINT('Ctrl Pts',(-1.44236470511145,1.,1.26273903323723));
#32862=CARTESIAN_POINT('Ctrl Pts',(-1.43734919180719,-1.,1.25983531011894));
#32863=CARTESIAN_POINT('Ctrl Pts',(-1.43734919180719,1.,1.25983531011894));
#32864=CARTESIAN_POINT('Ctrl Pts',(-1.43262645609679,-1.,1.25702687965744));
#32865=CARTESIAN_POINT('Ctrl Pts',(-1.43262645609679,1.,1.25702687965744));
#32866=CARTESIAN_POINT('Ctrl Pts',(-1.42815938799555,-1.,1.25426945222783));
#32867=CARTESIAN_POINT('Ctrl Pts',(-1.42815938799555,1.,1.25426945222783));
#32868=CARTESIAN_POINT('Ctrl Pts',(-1.42378102115911,-1.,1.25141455570299));
#32869=CARTESIAN_POINT('Ctrl Pts',(-1.42378102115911,1.,1.25141455570299));
#32870=CARTESIAN_POINT('Ctrl Pts',(-1.41923722596421,-1.,1.24824430986911));
#32871=CARTESIAN_POINT('Ctrl Pts',(-1.41923722596421,1.,1.24824430986911));
#32872=CARTESIAN_POINT('Ctrl Pts',(-1.41422913175437,-1.,1.24450600513278));
#32873=CARTESIAN_POINT('Ctrl Pts',(-1.41422913175437,1.,1.24450600513278));
#32874=CARTESIAN_POINT('Ctrl Pts',(-1.40845295531151,-1.,1.23994455029421));
#32875=CARTESIAN_POINT('Ctrl Pts',(-1.40845295531151,1.,1.23994455029421));
#32876=CARTESIAN_POINT('Ctrl Pts',(-1.40164708205345,-1.,1.23434087289768));
#32877=CARTESIAN_POINT('Ctrl Pts',(-1.40164708205345,1.,1.23434087289768));
#32878=CARTESIAN_POINT('Ctrl Pts',(-1.39361389567257,-1.,1.22752961898063));
#32879=CARTESIAN_POINT('Ctrl Pts',(-1.39361389567257,1.,1.22752961898063));
#32880=CARTESIAN_POINT('Ctrl Pts',(-1.38420564525391,-1.,1.21938737278853));
#32881=CARTESIAN_POINT('Ctrl Pts',(-1.38420564525391,1.,1.21938737278853));
#32882=CARTESIAN_POINT('Ctrl Pts',(-1.37331915604962,-1.,1.20982812923113));
#32883=CARTESIAN_POINT('Ctrl Pts',(-1.37331915604962,1.,1.20982812923113));
#32884=CARTESIAN_POINT('Ctrl Pts',(-1.36088705040677,-1.,1.1987959077656));
#32885=CARTESIAN_POINT('Ctrl Pts',(-1.36088705040677,1.,1.1987959077656));
#32886=CARTESIAN_POINT('Ctrl Pts',(-1.34687053998157,-1.,1.18625865664915));
#32887=CARTESIAN_POINT('Ctrl Pts',(-1.34687053998157,1.,1.18625865664915));
#32888=CARTESIAN_POINT('Ctrl Pts',(-1.33437539344842,-1.,1.17501305787994));
#32889=CARTESIAN_POINT('Ctrl Pts',(-1.33437539344842,1.,1.17501305787994));
#32890=CARTESIAN_POINT('Ctrl Pts',(-1.32428080720544,-1.,1.16589330092532));
#32891=CARTESIAN_POINT('Ctrl Pts',(-1.32428080720544,1.,1.16589330092532));
#32892=CARTESIAN_POINT('Ctrl Pts',(-1.3172297721596,-1.,1.15950888730433));
#32893=CARTESIAN_POINT('Ctrl Pts',(-1.3172297721596,1.,1.15950888730433));
#32894=CARTESIAN_POINT('Ctrl Pts',(-1.31362392696033,-1.,1.15624053661742));
#32895=CARTESIAN_POINT('Ctrl Pts',(-1.31362392696033,1.,1.15624053661742));
#32896=CARTESIAN_POINT('',(-1.73811241238545,1.,1.34869019493419));
#32897=CARTESIAN_POINT('Ctrl Pts',(-1.73811241238545,1.,1.34869019493419));
#32898=CARTESIAN_POINT('Ctrl Pts',(-1.73682580585819,1.,1.34854391898145));
#32899=CARTESIAN_POINT('Ctrl Pts',(-1.73425417886255,1.,1.34824783113158));
#32900=CARTESIAN_POINT('Ctrl Pts',(-1.73040149654497,1.,1.3477930915247));
#32901=CARTESIAN_POINT('Ctrl Pts',(-1.72527410681298,1.,1.34716554820013));
#32902=CARTESIAN_POINT('Ctrl Pts',(-1.7188807715095,1.,1.34634568653586));
#32903=CARTESIAN_POINT('Ctrl Pts',(-1.71250340687011,1.,1.34549029589563));
#32904=CARTESIAN_POINT('Ctrl Pts',(-1.70614212266676,1.,1.34459924533783));
#32905=CARTESIAN_POINT('Ctrl Pts',(-1.69979707754221,1.,1.34367237124322));
#32906=CARTESIAN_POINT('Ctrl Pts',(-1.6934684849664,1.,1.34270948206139));
#32907=CARTESIAN_POINT('Ctrl Pts',(-1.68715660868602,1.,1.34171037484673));
#32908=CARTESIAN_POINT('Ctrl Pts',(-1.68086176030308,1.,1.3406748518516));
#32909=CARTESIAN_POINT('Ctrl Pts',(-1.67458429426126,1.,1.33960273470372));
#32910=CARTESIAN_POINT('Ctrl Pts',(-1.66832460784078,1.,1.33849388654458));
#32911=CARTESIAN_POINT('Ctrl Pts',(-1.66208312542073,1.,1.33734820885331));
#32912=CARTESIAN_POINT('Ctrl Pts',(-1.65586025952651,1.,1.33616559745217));
#32913=CARTESIAN_POINT('Ctrl Pts',(-1.64965637286843,1.,1.33494590468003));
#32914=CARTESIAN_POINT('Ctrl Pts',(-1.64347174856007,1.,1.33368890676554));
#32915=CARTESIAN_POINT('Ctrl Pts',(-1.6373065347505,1.,1.33239425103694));
#32916=CARTESIAN_POINT('Ctrl Pts',(-1.63116079730887,1.,1.33106149345618));
#32917=CARTESIAN_POINT('Ctrl Pts',(-1.62503464209777,1.,1.32969019505665));
#32918=CARTESIAN_POINT('Ctrl Pts',(-1.61892832270723,1.,1.32828000610448));
#32919=CARTESIAN_POINT('Ctrl Pts',(-1.61284234015762,1.,1.32683074483365));
#32920=CARTESIAN_POINT('Ctrl Pts',(-1.6067775829097,1.,1.32534250785794));
#32921=CARTESIAN_POINT('Ctrl Pts',(-1.600735118587,1.,1.32381550858266));
#32922=CARTESIAN_POINT('Ctrl Pts',(-1.59471591079408,1.,1.32224985747686));
#32923=CARTESIAN_POINT('Ctrl Pts',(-1.58872057258244,1.,1.32064537110891));
#32924=CARTESIAN_POINT('Ctrl Pts',(-1.58274907898829,1.,1.31900135021428));
#32925=CARTESIAN_POINT('Ctrl Pts',(-1.57680056505585,1.,1.31731642317183));
#32926=CARTESIAN_POINT('Ctrl Pts',(-1.57087397835721,1.,1.31558903860015));
#32927=CARTESIAN_POINT('Ctrl Pts',(-1.56496872402352,1.,1.31381795281002));
#32928=CARTESIAN_POINT('Ctrl Pts',(-1.55908521254822,1.,1.31200264341696));
#32929=CARTESIAN_POINT('Ctrl Pts',(-1.55322568759481,1.,1.31014393684221));
#32930=CARTESIAN_POINT('Ctrl Pts',(-1.54739413957183,1.,1.30824393907471));
#32931=CARTESIAN_POINT('Ctrl Pts',(-1.54159462645428,1.,1.30630475189553));
#32932=CARTESIAN_POINT('Ctrl Pts',(-1.53582981268976,1.,1.30432735639487));
#32933=CARTESIAN_POINT('Ctrl Pts',(-1.53009970283893,1.,1.3023106439557));
#32934=CARTESIAN_POINT('Ctrl Pts',(-1.5243995786107,1.,1.30024984366334));
#32935=CARTESIAN_POINT('Ctrl Pts',(-1.51872184912735,1.,1.29813791800757));
#32936=CARTESIAN_POINT('Ctrl Pts',(-1.51305994241412,1.,1.29596850710518));
#32937=CARTESIAN_POINT('Ctrl Pts',(-1.50741159078367,1.,1.29373841372843));
#32938=CARTESIAN_POINT('Ctrl Pts',(-1.50178230149764,1.,1.29145022885171));
#32939=CARTESIAN_POINT('Ctrl Pts',(-1.49618896881729,1.,1.28911506584232));
#32940=CARTESIAN_POINT('Ctrl Pts',(-1.4906522831275,1.,1.28674676116415));
#32941=CARTESIAN_POINT('Ctrl Pts',(-1.48518817118891,1.,1.28435533880184));
#32942=CARTESIAN_POINT('Ctrl Pts',(-1.47980070347102,1.,1.28194158939522));
#32943=CARTESIAN_POINT('Ctrl Pts',(-1.4744717526711,1.,1.27948918248524));
#32944=CARTESIAN_POINT('Ctrl Pts',(-1.46916035917197,1.,1.27696414831144));
#32945=CARTESIAN_POINT('Ctrl Pts',(-1.4638243133254,1.,1.27433119897877));
#32946=CARTESIAN_POINT('Ctrl Pts',(-1.45843906294725,1.,1.27156805265312));
#32947=CARTESIAN_POINT('Ctrl Pts',(-1.45301422764205,1.,1.26867786804854));
#32948=CARTESIAN_POINT('Ctrl Pts',(-1.44761985001544,1.,1.26570925118767));
#32949=CARTESIAN_POINT('Ctrl Pts',(-1.44236470511145,1.,1.26273903323723));
#32950=CARTESIAN_POINT('Ctrl Pts',(-1.43734919180719,1.,1.25983531011894));
#32951=CARTESIAN_POINT('Ctrl Pts',(-1.43262645609679,1.,1.25702687965744));
#32952=CARTESIAN_POINT('Ctrl Pts',(-1.42815938799555,1.,1.25426945222783));
#32953=CARTESIAN_POINT('Ctrl Pts',(-1.42378102115911,1.,1.25141455570299));
#32954=CARTESIAN_POINT('Ctrl Pts',(-1.41923722596421,1.,1.24824430986911));
#32955=CARTESIAN_POINT('Ctrl Pts',(-1.41422913175437,1.,1.24450600513278));
#32956=CARTESIAN_POINT('Ctrl Pts',(-1.40845295531151,1.,1.23994455029421));
#32957=CARTESIAN_POINT('Ctrl Pts',(-1.40164708205345,1.,1.23434087289768));
#32958=CARTESIAN_POINT('Ctrl Pts',(-1.39361389567257,1.,1.22752961898063));
#32959=CARTESIAN_POINT('Ctrl Pts',(-1.38420564525391,1.,1.21938737278853));
#32960=CARTESIAN_POINT('Ctrl Pts',(-1.37331915604962,1.,1.20982812923113));
#32961=CARTESIAN_POINT('Ctrl Pts',(-1.36088705040677,1.,1.1987959077656));
#32962=CARTESIAN_POINT('Ctrl Pts',(-1.34687053998157,1.,1.18625865664915));
#32963=CARTESIAN_POINT('Ctrl Pts',(-1.33437539344842,1.,1.17501305787994));
#32964=CARTESIAN_POINT('Ctrl Pts',(-1.32428080720544,1.,1.16589330092532));
#32965=CARTESIAN_POINT('Ctrl Pts',(-1.3172297721596,1.,1.15950888730433));
#32966=CARTESIAN_POINT('Ctrl Pts',(-1.31362392696033,1.,1.15624053661742));
#32967=CARTESIAN_POINT('',(-1.73811241238545,0.,1.34869019493419));
#32968=CARTESIAN_POINT('Origin',(-1.81978687191668,0.,1.23627494547115));
#32969=CARTESIAN_POINT('',(-1.81978687191668,1.,1.23627494547115));
#32970=CARTESIAN_POINT('',(-1.73811241238545,1.,1.34869019493419));
#32971=CARTESIAN_POINT('',(-1.81978687191668,0.,1.23627494547115));
#32972=CARTESIAN_POINT('Ctrl Pts',(-1.5055822144029,-1.,0.892032620296855));
#32973=CARTESIAN_POINT('Ctrl Pts',(-1.5055822144029,1.,0.892032620296855));
#32974=CARTESIAN_POINT('Ctrl Pts',(-1.50980486807181,-1.,0.894452006967538));
#32975=CARTESIAN_POINT('Ctrl Pts',(-1.50980486807181,1.,0.894452006967538));
#32976=CARTESIAN_POINT('Ctrl Pts',(-1.51805569591479,-1.,0.89918504749193));
#32977=CARTESIAN_POINT('Ctrl Pts',(-1.51805569591479,1.,0.89918504749193));
#32978=CARTESIAN_POINT('Ctrl Pts',(-1.52984849890434,-1.,0.905967409640499));
#32979=CARTESIAN_POINT('Ctrl Pts',(-1.52984849890434,1.,0.905967409640499));
#32980=CARTESIAN_POINT('Ctrl Pts',(-1.54440491152808,-1.,0.91437591904658));
#32981=CARTESIAN_POINT('Ctrl Pts',(-1.54440491152808,1.,0.91437591904658));
#32982=CARTESIAN_POINT('Ctrl Pts',(-1.56065988582509,-1.,0.923832188966322));
#32983=CARTESIAN_POINT('Ctrl Pts',(-1.56065988582509,1.,0.923832188966322));
#32984=CARTESIAN_POINT('Ctrl Pts',(-1.57499388385561,-1.,0.932246680128849));
#32985=CARTESIAN_POINT('Ctrl Pts',(-1.57499388385561,1.,0.932246680128849));
#32986=CARTESIAN_POINT('Ctrl Pts',(-1.58744937489796,-1.,0.939646377909319));
#32987=CARTESIAN_POINT('Ctrl Pts',(-1.58744937489796,1.,0.939646377909319));
#32988=CARTESIAN_POINT('Ctrl Pts',(-1.59810042045408,-1.,0.946078063325796));
#32989=CARTESIAN_POINT('Ctrl Pts',(-1.59810042045408,1.,0.946078063325796));
#32990=CARTESIAN_POINT('Ctrl Pts',(-1.60706069897794,-1.,0.951613284361248));
#32991=CARTESIAN_POINT('Ctrl Pts',(-1.60706069897794,1.,0.951613284361248));
#32992=CARTESIAN_POINT('Ctrl Pts',(-1.61449324337233,-1.,0.956354422921573));
#32993=CARTESIAN_POINT('Ctrl Pts',(-1.61449324337233,1.,0.956354422921573));
#32994=CARTESIAN_POINT('Ctrl Pts',(-1.62061638139929,-1.,0.960438326099958));
#32995=CARTESIAN_POINT('Ctrl Pts',(-1.62061638139929,1.,0.960438326099958));
#32996=CARTESIAN_POINT('Ctrl Pts',(-1.6257193066974,-1.,0.964046107037821));
#32997=CARTESIAN_POINT('Ctrl Pts',(-1.6257193066974,1.,0.964046107037821));
#32998=CARTESIAN_POINT('Ctrl Pts',(-1.63013849959083,-1.,0.967387853228041));
#32999=CARTESIAN_POINT('Ctrl Pts',(-1.63013849959083,1.,0.967387853228041));
#33000=CARTESIAN_POINT('Ctrl Pts',(-1.63420665729609,-1.,0.970669715996356));
#33001=CARTESIAN_POINT('Ctrl Pts',(-1.63420665729609,1.,0.970669715996356));
#33002=CARTESIAN_POINT('Ctrl Pts',(-1.63820952658157,-1.,0.974066058287501));
#33003=CARTESIAN_POINT('Ctrl Pts',(-1.63820952658157,1.,0.974066058287501));
#33004=CARTESIAN_POINT('Ctrl Pts',(-1.64233990826831,-1.,0.977689794120297));
#33005=CARTESIAN_POINT('Ctrl Pts',(-1.64233990826831,1.,0.977689794120297));
#33006=CARTESIAN_POINT('Ctrl Pts',(-1.64665139190834,-1.,0.981562530940574));
#33007=CARTESIAN_POINT('Ctrl Pts',(-1.64665139190834,1.,0.981562530940574));
#33008=CARTESIAN_POINT('Ctrl Pts',(-1.6511001661277,-1.,0.985642622921626));
#33009=CARTESIAN_POINT('Ctrl Pts',(-1.6511001661277,1.,0.985642622921626));
#33010=CARTESIAN_POINT('Ctrl Pts',(-1.65559044289746,-1.,0.98985562785445));
#33011=CARTESIAN_POINT('Ctrl Pts',(-1.65559044289746,1.,0.98985562785445));
#33012=CARTESIAN_POINT('Ctrl Pts',(-1.66001553809916,-1.,0.994121836661116));
#33013=CARTESIAN_POINT('Ctrl Pts',(-1.66001553809916,1.,0.994121836661116));
#33014=CARTESIAN_POINT('Ctrl Pts',(-1.66430758030304,-1.,0.998389654952317));
#33015=CARTESIAN_POINT('Ctrl Pts',(-1.66430758030304,1.,0.998389654952317));
#33016=CARTESIAN_POINT('Ctrl Pts',(-1.66846059277231,-1.,1.00265091003682));
#33017=CARTESIAN_POINT('Ctrl Pts',(-1.66846059277231,1.,1.00265091003682));
#33018=CARTESIAN_POINT('Ctrl Pts',(-1.67250335383248,-1.,1.00692206696387));
#33019=CARTESIAN_POINT('Ctrl Pts',(-1.67250335383248,1.,1.00692206696387));
#33020=CARTESIAN_POINT('Ctrl Pts',(-1.67648246776457,-1.,1.01123236493507));
#33021=CARTESIAN_POINT('Ctrl Pts',(-1.67648246776457,1.,1.01123236493507));
#33022=CARTESIAN_POINT('Ctrl Pts',(-1.6804428989482,-1.,1.01561026162787));
#33023=CARTESIAN_POINT('Ctrl Pts',(-1.6804428989482,1.,1.01561026162787));
#33024=CARTESIAN_POINT('Ctrl Pts',(-1.68440578021739,-1.,1.02006795074222));
#33025=CARTESIAN_POINT('Ctrl Pts',(-1.68440578021739,1.,1.02006795074222));
#33026=CARTESIAN_POINT('Ctrl Pts',(-1.68836910178475,-1.,1.02460180535272));
#33027=CARTESIAN_POINT('Ctrl Pts',(-1.68836910178475,1.,1.02460180535272));
#33028=CARTESIAN_POINT('Ctrl Pts',(-1.69231840863471,-1.,1.02919977579155));
#33029=CARTESIAN_POINT('Ctrl Pts',(-1.69231840863471,1.,1.02919977579155));
#33030=CARTESIAN_POINT('Ctrl Pts',(-1.69623414782769,-1.,1.03384646003587));
#33031=CARTESIAN_POINT('Ctrl Pts',(-1.69623414782769,1.,1.03384646003587));
#33032=CARTESIAN_POINT('Ctrl Pts',(-1.70010052930951,-1.,1.03852922490782));
#33033=CARTESIAN_POINT('Ctrl Pts',(-1.70010052930951,1.,1.03852922490782));
#33034=CARTESIAN_POINT('Ctrl Pts',(-1.70391338707969,-1.,1.04324363334546));
#33035=CARTESIAN_POINT('Ctrl Pts',(-1.70391338707969,1.,1.04324363334546));
#33036=CARTESIAN_POINT('Ctrl Pts',(-1.70767646263641,-1.,1.0479908540499));
#33037=CARTESIAN_POINT('Ctrl Pts',(-1.70767646263641,1.,1.0479908540499));
#33038=CARTESIAN_POINT('Ctrl Pts',(-1.71139783543986,-1.,1.05277517202854));
#33039=CARTESIAN_POINT('Ctrl Pts',(-1.71139783543986,1.,1.05277517202854));
#33040=CARTESIAN_POINT('Ctrl Pts',(-1.71508654427022,-1.,1.05760163192481));
#33041=CARTESIAN_POINT('Ctrl Pts',(-1.71508654427022,1.,1.05760163192481));
#33042=CARTESIAN_POINT('Ctrl Pts',(-1.71874858456908,-1.,1.0624732468065));
#33043=CARTESIAN_POINT('Ctrl Pts',(-1.71874858456908,1.,1.0624732468065));
#33044=CARTESIAN_POINT('Ctrl Pts',(-1.72238500928456,-1.,1.06738966975463));
#33045=CARTESIAN_POINT('Ctrl Pts',(-1.72238500928456,1.,1.06738966975463));
#33046=CARTESIAN_POINT('Ctrl Pts',(-1.72599406198489,-1.,1.07234866990252));
#33047=CARTESIAN_POINT('Ctrl Pts',(-1.72599406198489,1.,1.07234866990252));
#33048=CARTESIAN_POINT('Ctrl Pts',(-1.72957248977424,-1.,1.0773470373727));
#33049=CARTESIAN_POINT('Ctrl Pts',(-1.72957248977424,1.,1.0773470373727));
#33050=CARTESIAN_POINT('Ctrl Pts',(-1.73311705663407,-1.,1.08238162784749));
#33051=CARTESIAN_POINT('Ctrl Pts',(-1.73311705663407,1.,1.08238162784749));
#33052=CARTESIAN_POINT('Ctrl Pts',(-1.73662628326093,-1.,1.08745056285429));
#33053=CARTESIAN_POINT('Ctrl Pts',(-1.73662628326093,1.,1.08745056285429));
#33054=CARTESIAN_POINT('Ctrl Pts',(-1.74010053962252,-1.,1.09255329056496));
#33055=CARTESIAN_POINT('Ctrl Pts',(-1.74010053962252,1.,1.09255329056496));
#33056=CARTESIAN_POINT('Ctrl Pts',(-1.74354119236212,-1.,1.09768999241229));
#33057=CARTESIAN_POINT('Ctrl Pts',(-1.74354119236212,1.,1.09768999241229));
#33058=CARTESIAN_POINT('Ctrl Pts',(-1.74695004214924,-1.,1.10286118991144));
#33059=CARTESIAN_POINT('Ctrl Pts',(-1.74695004214924,1.,1.10286118991144));
#33060=CARTESIAN_POINT('Ctrl Pts',(-1.75032866075914,-1.,1.10806728183003));
#33061=CARTESIAN_POINT('Ctrl Pts',(-1.75032866075914,1.,1.10806728183003));
#33062=CARTESIAN_POINT('Ctrl Pts',(-1.75367772094617,-1.,1.11330807582542));
#33063=CARTESIAN_POINT('Ctrl Pts',(-1.75367772094617,1.,1.11330807582542));
#33064=CARTESIAN_POINT('Ctrl Pts',(-1.75699720772089,-1.,1.11858293216752));
#33065=CARTESIAN_POINT('Ctrl Pts',(-1.75699720772089,1.,1.11858293216752));
#33066=CARTESIAN_POINT('Ctrl Pts',(-1.76028671825084,-1.,1.12389096855078));
#33067=CARTESIAN_POINT('Ctrl Pts',(-1.76028671825084,1.,1.12389096855078));
#33068=CARTESIAN_POINT('Ctrl Pts',(-1.76354571966171,-1.,1.12923123555076));
#33069=CARTESIAN_POINT('Ctrl Pts',(-1.76354571966171,1.,1.12923123555076));
#33070=CARTESIAN_POINT('Ctrl Pts',(-1.76677384551883,-1.,1.13460291804635));
#33071=CARTESIAN_POINT('Ctrl Pts',(-1.76677384551883,1.,1.13460291804635));
#33072=CARTESIAN_POINT('Ctrl Pts',(-1.76997111386806,-1.,1.14000548337));
#33073=CARTESIAN_POINT('Ctrl Pts',(-1.76997111386806,1.,1.14000548337));
#33074=CARTESIAN_POINT('Ctrl Pts',(-1.77313777896234,-1.,1.14543858226948));
#33075=CARTESIAN_POINT('Ctrl Pts',(-1.77313777896234,1.,1.14543858226948));
#33076=CARTESIAN_POINT('Ctrl Pts',(-1.77627422557034,-1.,1.15090197841531));
#33077=CARTESIAN_POINT('Ctrl Pts',(-1.77627422557034,1.,1.15090197841531));
#33078=CARTESIAN_POINT('Ctrl Pts',(-1.77938085564261,-1.,1.15639547194689));
#33079=CARTESIAN_POINT('Ctrl Pts',(-1.77938085564261,1.,1.15639547194689));
#33080=CARTESIAN_POINT('Ctrl Pts',(-1.78245795880949,-1.,1.16191881298458));
#33081=CARTESIAN_POINT('Ctrl Pts',(-1.78245795880949,1.,1.16191881298458));
#33082=CARTESIAN_POINT('Ctrl Pts',(-1.78550566040349,-1.,1.16747166312239));
#33083=CARTESIAN_POINT('Ctrl Pts',(-1.78550566040349,1.,1.16747166312239));
#33084=CARTESIAN_POINT('Ctrl Pts',(-1.78852398877523,-1.,1.17305363177265));
#33085=CARTESIAN_POINT('Ctrl Pts',(-1.78852398877523,1.,1.17305363177265));
#33086=CARTESIAN_POINT('Ctrl Pts',(-1.79151291552646,-1.,1.17866429440781));
#33087=CARTESIAN_POINT('Ctrl Pts',(-1.79151291552646,1.,1.17866429440781));
#33088=CARTESIAN_POINT('Ctrl Pts',(-1.79447240321572,-1.,1.18430321697471));
#33089=CARTESIAN_POINT('Ctrl Pts',(-1.79447240321572,1.,1.18430321697471));
#33090=CARTESIAN_POINT('Ctrl Pts',(-1.79740245923649,-1.,1.1899699793456));
#33091=CARTESIAN_POINT('Ctrl Pts',(-1.79740245923649,1.,1.1899699793456));
#33092=CARTESIAN_POINT('Ctrl Pts',(-1.80030314370121,-1.,1.19566418930405));
#33093=CARTESIAN_POINT('Ctrl Pts',(-1.80030314370121,1.,1.19566418930405));
#33094=CARTESIAN_POINT('Ctrl Pts',(-1.8031745483882,-1.,1.2013854893912));
#33095=CARTESIAN_POINT('Ctrl Pts',(-1.8031745483882,1.,1.2013854893912));
#33096=CARTESIAN_POINT('Ctrl Pts',(-1.80601678480772,-1.,1.20713356605519));
#33097=CARTESIAN_POINT('Ctrl Pts',(-1.80601678480772,1.,1.20713356605519));
#33098=CARTESIAN_POINT('Ctrl Pts',(-1.80882996916931,-1.,1.2129081570818));
#33099=CARTESIAN_POINT('Ctrl Pts',(-1.80882996916931,1.,1.2129081570818));
#33100=CARTESIAN_POINT('Ctrl Pts',(-1.81161420806172,-1.,1.2187090610323));
#33101=CARTESIAN_POINT('Ctrl Pts',(-1.81161420806172,1.,1.2187090610323));
#33102=CARTESIAN_POINT('Ctrl Pts',(-1.81436959209778,-1.,1.22453613304507));
#33103=CARTESIAN_POINT('Ctrl Pts',(-1.81436959209778,1.,1.22453613304507));
#33104=CARTESIAN_POINT('Ctrl Pts',(-1.81655087183054,-1.,1.22921864890975));
#33105=CARTESIAN_POINT('Ctrl Pts',(-1.81655087183054,1.,1.22921864890975));
#33106=CARTESIAN_POINT('Ctrl Pts',(-1.81817389920914,-1.,1.23274224526804));
#33107=CARTESIAN_POINT('Ctrl Pts',(-1.81817389920914,1.,1.23274224526804));
#33108=CARTESIAN_POINT('Ctrl Pts',(-1.81925017193531,-1.,1.23509651170384));
#33109=CARTESIAN_POINT('Ctrl Pts',(-1.81925017193531,1.,1.23509651170384));
#33110=CARTESIAN_POINT('Ctrl Pts',(-1.81978687191668,-1.,1.23627494547115));
#33111=CARTESIAN_POINT('Ctrl Pts',(-1.81978687191668,1.,1.23627494547115));
#33112=CARTESIAN_POINT('',(-1.5055822144029,1.,0.892032620296855));
#33113=CARTESIAN_POINT('Ctrl Pts',(-1.5055822144029,1.,0.892032620296855));
#33114=CARTESIAN_POINT('Ctrl Pts',(-1.50980486807181,1.,0.894452006967538));
#33115=CARTESIAN_POINT('Ctrl Pts',(-1.51805569591479,1.,0.89918504749193));
#33116=CARTESIAN_POINT('Ctrl Pts',(-1.52984849890434,1.,0.905967409640499));
#33117=CARTESIAN_POINT('Ctrl Pts',(-1.54440491152808,1.,0.91437591904658));
#33118=CARTESIAN_POINT('Ctrl Pts',(-1.56065988582509,1.,0.923832188966322));
#33119=CARTESIAN_POINT('Ctrl Pts',(-1.57499388385561,1.,0.932246680128849));
#33120=CARTESIAN_POINT('Ctrl Pts',(-1.58744937489796,1.,0.939646377909319));
#33121=CARTESIAN_POINT('Ctrl Pts',(-1.59810042045408,1.,0.946078063325796));
#33122=CARTESIAN_POINT('Ctrl Pts',(-1.60706069897794,1.,0.951613284361248));
#33123=CARTESIAN_POINT('Ctrl Pts',(-1.61449324337233,1.,0.956354422921573));
#33124=CARTESIAN_POINT('Ctrl Pts',(-1.62061638139929,1.,0.960438326099958));
#33125=CARTESIAN_POINT('Ctrl Pts',(-1.6257193066974,1.,0.964046107037821));
#33126=CARTESIAN_POINT('Ctrl Pts',(-1.63013849959083,1.,0.967387853228041));
#33127=CARTESIAN_POINT('Ctrl Pts',(-1.63420665729609,1.,0.970669715996356));
#33128=CARTESIAN_POINT('Ctrl Pts',(-1.63820952658157,1.,0.974066058287501));
#33129=CARTESIAN_POINT('Ctrl Pts',(-1.64233990826831,1.,0.977689794120297));
#33130=CARTESIAN_POINT('Ctrl Pts',(-1.64665139190834,1.,0.981562530940574));
#33131=CARTESIAN_POINT('Ctrl Pts',(-1.6511001661277,1.,0.985642622921626));
#33132=CARTESIAN_POINT('Ctrl Pts',(-1.65559044289746,1.,0.98985562785445));
#33133=CARTESIAN_POINT('Ctrl Pts',(-1.66001553809916,1.,0.994121836661116));
#33134=CARTESIAN_POINT('Ctrl Pts',(-1.66430758030304,1.,0.998389654952317));
#33135=CARTESIAN_POINT('Ctrl Pts',(-1.66846059277231,1.,1.00265091003682));
#33136=CARTESIAN_POINT('Ctrl Pts',(-1.67250335383248,1.,1.00692206696387));
#33137=CARTESIAN_POINT('Ctrl Pts',(-1.67648246776457,1.,1.01123236493507));
#33138=CARTESIAN_POINT('Ctrl Pts',(-1.6804428989482,1.,1.01561026162787));
#33139=CARTESIAN_POINT('Ctrl Pts',(-1.68440578021739,1.,1.02006795074222));
#33140=CARTESIAN_POINT('Ctrl Pts',(-1.68836910178475,1.,1.02460180535272));
#33141=CARTESIAN_POINT('Ctrl Pts',(-1.69231840863471,1.,1.02919977579155));
#33142=CARTESIAN_POINT('Ctrl Pts',(-1.69623414782769,1.,1.03384646003587));
#33143=CARTESIAN_POINT('Ctrl Pts',(-1.70010052930951,1.,1.03852922490782));
#33144=CARTESIAN_POINT('Ctrl Pts',(-1.70391338707969,1.,1.04324363334546));
#33145=CARTESIAN_POINT('Ctrl Pts',(-1.70767646263641,1.,1.0479908540499));
#33146=CARTESIAN_POINT('Ctrl Pts',(-1.71139783543986,1.,1.05277517202854));
#33147=CARTESIAN_POINT('Ctrl Pts',(-1.71508654427022,1.,1.05760163192481));
#33148=CARTESIAN_POINT('Ctrl Pts',(-1.71874858456908,1.,1.0624732468065));
#33149=CARTESIAN_POINT('Ctrl Pts',(-1.72238500928456,1.,1.06738966975463));
#33150=CARTESIAN_POINT('Ctrl Pts',(-1.72599406198489,1.,1.07234866990252));
#33151=CARTESIAN_POINT('Ctrl Pts',(-1.72957248977424,1.,1.0773470373727));
#33152=CARTESIAN_POINT('Ctrl Pts',(-1.73311705663407,1.,1.08238162784749));
#33153=CARTESIAN_POINT('Ctrl Pts',(-1.73662628326093,1.,1.08745056285429));
#33154=CARTESIAN_POINT('Ctrl Pts',(-1.74010053962252,1.,1.09255329056496));
#33155=CARTESIAN_POINT('Ctrl Pts',(-1.74354119236212,1.,1.09768999241229));
#33156=CARTESIAN_POINT('Ctrl Pts',(-1.74695004214924,1.,1.10286118991144));
#33157=CARTESIAN_POINT('Ctrl Pts',(-1.75032866075914,1.,1.10806728183003));
#33158=CARTESIAN_POINT('Ctrl Pts',(-1.75367772094617,1.,1.11330807582542));
#33159=CARTESIAN_POINT('Ctrl Pts',(-1.75699720772089,1.,1.11858293216752));
#33160=CARTESIAN_POINT('Ctrl Pts',(-1.76028671825084,1.,1.12389096855078));
#33161=CARTESIAN_POINT('Ctrl Pts',(-1.76354571966171,1.,1.12923123555076));
#33162=CARTESIAN_POINT('Ctrl Pts',(-1.76677384551883,1.,1.13460291804635));
#33163=CARTESIAN_POINT('Ctrl Pts',(-1.76997111386806,1.,1.14000548337));
#33164=CARTESIAN_POINT('Ctrl Pts',(-1.77313777896234,1.,1.14543858226948));
#33165=CARTESIAN_POINT('Ctrl Pts',(-1.77627422557034,1.,1.15090197841531));
#33166=CARTESIAN_POINT('Ctrl Pts',(-1.77938085564261,1.,1.15639547194689));
#33167=CARTESIAN_POINT('Ctrl Pts',(-1.78245795880949,1.,1.16191881298458));
#33168=CARTESIAN_POINT('Ctrl Pts',(-1.78550566040349,1.,1.16747166312239));
#33169=CARTESIAN_POINT('Ctrl Pts',(-1.78852398877523,1.,1.17305363177265));
#33170=CARTESIAN_POINT('Ctrl Pts',(-1.79151291552646,1.,1.17866429440781));
#33171=CARTESIAN_POINT('Ctrl Pts',(-1.79447240321572,1.,1.18430321697471));
#33172=CARTESIAN_POINT('Ctrl Pts',(-1.79740245923649,1.,1.1899699793456));
#33173=CARTESIAN_POINT('Ctrl Pts',(-1.80030314370121,1.,1.19566418930405));
#33174=CARTESIAN_POINT('Ctrl Pts',(-1.8031745483882,1.,1.2013854893912));
#33175=CARTESIAN_POINT('Ctrl Pts',(-1.80601678480772,1.,1.20713356605519));
#33176=CARTESIAN_POINT('Ctrl Pts',(-1.80882996916931,1.,1.2129081570818));
#33177=CARTESIAN_POINT('Ctrl Pts',(-1.81161420806172,1.,1.2187090610323));
#33178=CARTESIAN_POINT('Ctrl Pts',(-1.81436959209778,1.,1.22453613304507));
#33179=CARTESIAN_POINT('Ctrl Pts',(-1.81655087183054,1.,1.22921864890975));
#33180=CARTESIAN_POINT('Ctrl Pts',(-1.81817389920914,1.,1.23274224526804));
#33181=CARTESIAN_POINT('Ctrl Pts',(-1.81925017193531,1.,1.23509651170384));
#33182=CARTESIAN_POINT('Ctrl Pts',(-1.81978687191668,1.,1.23627494547115));
#33183=CARTESIAN_POINT('',(-1.5055822144029,0.,0.892032620296856));
#33184=CARTESIAN_POINT('Origin',(0.,0.,0.));
#33185=CARTESIAN_POINT('',(-1.60662857109684,1.,0.693717979106305));
#33186=CARTESIAN_POINT('Origin',(0.,1.,0.));
#33187=CARTESIAN_POINT('',(-1.60662857109684,0.,0.693717979106306));
#33188=CARTESIAN_POINT('Ctrl Pts',(-2.0698113262342,-1.,0.7455743247944));
#33189=CARTESIAN_POINT('Ctrl Pts',(-2.0698113262342,1.,0.7455743247944));
#33190=CARTESIAN_POINT('Ctrl Pts',(-2.06854248895728,-1.,0.745832791378367));
#33191=CARTESIAN_POINT('Ctrl Pts',(-2.06854248895728,1.,0.745832791378367));
#33192=CARTESIAN_POINT('Ctrl Pts',(-2.06600523016815,-1.,0.7463458715442));
#33193=CARTESIAN_POINT('Ctrl Pts',(-2.06600523016815,1.,0.7463458715442));
#33194=CARTESIAN_POINT('Ctrl Pts',(-2.06220058927826,-1.,0.747103932787919));
#33195=CARTESIAN_POINT('Ctrl Pts',(-2.06220058927826,1.,0.747103932787919));
#33196=CARTESIAN_POINT('Ctrl Pts',(-2.05713023031006,-1.,0.748091554183802));
#33197=CARTESIAN_POINT('Ctrl Pts',(-2.05713023031006,1.,0.748091554183802));
#33198=CARTESIAN_POINT('Ctrl Pts',(-2.05079645592154,-1.,0.749287468665046));
#33199=CARTESIAN_POINT('Ctrl Pts',(-2.05079645592154,1.,0.749287468665046));
#33200=CARTESIAN_POINT('Ctrl Pts',(-2.04446689147979,-1.,0.750444657875576));
#33201=CARTESIAN_POINT('Ctrl Pts',(-2.04446689147979,1.,0.750444657875576));
#33202=CARTESIAN_POINT('Ctrl Pts',(-2.03814160092099,-1.,0.751562963361115));
#33203=CARTESIAN_POINT('Ctrl Pts',(-2.03814160092099,1.,0.751562963361115));
#33204=CARTESIAN_POINT('Ctrl Pts',(-2.03182068456221,-1.,0.752642180487211));
#33205=CARTESIAN_POINT('Ctrl Pts',(-2.03182068456221,1.,0.752642180487211));
#33206=CARTESIAN_POINT('Ctrl Pts',(-2.02550428623313,-1.,0.753682061112768));
#33207=CARTESIAN_POINT('Ctrl Pts',(-2.02550428623313,1.,0.753682061112768));
#33208=CARTESIAN_POINT('Ctrl Pts',(-2.01919259405809,-1.,0.754682330722816));
#33209=CARTESIAN_POINT('Ctrl Pts',(-2.01919259405809,1.,0.754682330722816));
#33210=CARTESIAN_POINT('Ctrl Pts',(-2.01288584328084,-1.,0.755642704957865));
#33211=CARTESIAN_POINT('Ctrl Pts',(-2.01288584328084,1.,0.755642704957865));
#33212=CARTESIAN_POINT('Ctrl Pts',(-2.0065843158773,-1.,0.75656290464667));
#33213=CARTESIAN_POINT('Ctrl Pts',(-2.0065843158773,1.,0.75656290464667));
#33214=CARTESIAN_POINT('Ctrl Pts',(-2.00028834739178,-1.,0.757442676862724));
#33215=CARTESIAN_POINT('Ctrl Pts',(-2.00028834739178,1.,0.757442676862724));
#33216=CARTESIAN_POINT('Ctrl Pts',(-1.99399831098817,-1.,0.758281796766761));
#33217=CARTESIAN_POINT('Ctrl Pts',(-1.99399831098817,1.,0.758281796766761));
#33218=CARTESIAN_POINT('Ctrl Pts',(-1.98771456680874,-1.,0.759080037802488));
#33219=CARTESIAN_POINT('Ctrl Pts',(-1.98771456680874,1.,0.759080037802488));
#33220=CARTESIAN_POINT('Ctrl Pts',(-1.98143741418172,-1.,0.75983714745219));
#33221=CARTESIAN_POINT('Ctrl Pts',(-1.98143741418172,1.,0.75983714745219));
#33222=CARTESIAN_POINT('Ctrl Pts',(-1.97516705321494,-1.,0.760552825409757));
#33223=CARTESIAN_POINT('Ctrl Pts',(-1.97516705321494,1.,0.760552825409757));
#33224=CARTESIAN_POINT('Ctrl Pts',(-1.96890351582499,-1.,0.76122669048382));
#33225=CARTESIAN_POINT('Ctrl Pts',(-1.96890351582499,1.,0.76122669048382));
#33226=CARTESIAN_POINT('Ctrl Pts',(-1.96264672744186,-1.,0.761858300014423));
#33227=CARTESIAN_POINT('Ctrl Pts',(-1.96264672744186,1.,0.761858300014423));
#33228=CARTESIAN_POINT('Ctrl Pts',(-1.95639665309869,-1.,0.762447203806179));
#33229=CARTESIAN_POINT('Ctrl Pts',(-1.95639665309869,1.,0.762447203806179));
#33230=CARTESIAN_POINT('Ctrl Pts',(-1.95015342590024,-1.,0.762992990878769));
#33231=CARTESIAN_POINT('Ctrl Pts',(-1.95015342590024,1.,0.762992990878769));
#33232=CARTESIAN_POINT('Ctrl Pts',(-1.9439174661764,-1.,0.763495333538629));
#33233=CARTESIAN_POINT('Ctrl Pts',(-1.9439174661764,1.,0.763495333538629));
#33234=CARTESIAN_POINT('Ctrl Pts',(-1.93768964875886,-1.,0.763954049121458));
#33235=CARTESIAN_POINT('Ctrl Pts',(-1.93768964875886,1.,0.763954049121458));
#33236=CARTESIAN_POINT('Ctrl Pts',(-1.93147105496382,-1.,0.76436901067394));
#33237=CARTESIAN_POINT('Ctrl Pts',(-1.93147105496382,1.,0.76436901067394));
#33238=CARTESIAN_POINT('Ctrl Pts',(-1.92526263537048,-1.,0.764740025488211));
#33239=CARTESIAN_POINT('Ctrl Pts',(-1.92526263537048,1.,0.764740025488211));
#33240=CARTESIAN_POINT('Ctrl Pts',(-1.91906491634196,-1.,0.765066729667088));
#33241=CARTESIAN_POINT('Ctrl Pts',(-1.91906491634196,1.,0.765066729667088));
#33242=CARTESIAN_POINT('Ctrl Pts',(-1.91287765805169,-1.,0.765348465884722));
#33243=CARTESIAN_POINT('Ctrl Pts',(-1.91287765805169,1.,0.765348465884722));
#33244=CARTESIAN_POINT('Ctrl Pts',(-1.90669961402356,-1.,0.765584196937919));
#33245=CARTESIAN_POINT('Ctrl Pts',(-1.90669961402356,1.,0.765584196937919));
#33246=CARTESIAN_POINT('Ctrl Pts',(-1.90052930393596,-1.,0.765772772593386));
#33247=CARTESIAN_POINT('Ctrl Pts',(-1.90052930393596,1.,0.765772772593386));
#33248=CARTESIAN_POINT('Ctrl Pts',(-1.89436577771388,-1.,0.765913193856978));
#33249=CARTESIAN_POINT('Ctrl Pts',(-1.89436577771388,1.,0.765913193856978));
#33250=CARTESIAN_POINT('Ctrl Pts',(-1.88820926433409,-1.,0.766004837062091));
#33251=CARTESIAN_POINT('Ctrl Pts',(-1.88820926433409,1.,0.766004837062091));
#33252=CARTESIAN_POINT('Ctrl Pts',(-1.88206215302561,-1.,0.766047794851864));
#33253=CARTESIAN_POINT('Ctrl Pts',(-1.88206215302561,1.,0.766047794851864));
#33254=CARTESIAN_POINT('Ctrl Pts',(-1.87592888967883,-1.,0.766042837036744));
#33255=CARTESIAN_POINT('Ctrl Pts',(-1.87592888967883,1.,0.766042837036744));
#33256=CARTESIAN_POINT('Ctrl Pts',(-1.86981398314341,-1.,0.765990708546091));
#33257=CARTESIAN_POINT('Ctrl Pts',(-1.86981398314341,1.,0.765990708546091));
#33258=CARTESIAN_POINT('Ctrl Pts',(-1.86372027063312,-1.,0.765891519092547));
#33259=CARTESIAN_POINT('Ctrl Pts',(-1.86372027063312,1.,0.765891519092547));
#33260=CARTESIAN_POINT('Ctrl Pts',(-1.85764741390394,-1.,0.765744212909318));
#33261=CARTESIAN_POINT('Ctrl Pts',(-1.85764741390394,1.,0.765744212909318));
#33262=CARTESIAN_POINT('Ctrl Pts',(-1.85158945130063,-1.,0.765545710619062));
#33263=CARTESIAN_POINT('Ctrl Pts',(-1.85158945130063,1.,0.765545710619062));
#33264=CARTESIAN_POINT('Ctrl Pts',(-1.84553698875924,-1.,0.765291664862029));
#33265=CARTESIAN_POINT('Ctrl Pts',(-1.84553698875924,1.,0.765291664862029));
#33266=CARTESIAN_POINT('Ctrl Pts',(-1.83948181064835,-1.,0.764978057881737));
#33267=CARTESIAN_POINT('Ctrl Pts',(-1.83948181064835,1.,0.764978057881737));
#33268=CARTESIAN_POINT('Ctrl Pts',(-1.83342077227142,-1.,0.764602549687853));
#33269=CARTESIAN_POINT('Ctrl Pts',(-1.83342077227142,1.,0.764602549687853));
#33270=CARTESIAN_POINT('Ctrl Pts',(-1.82735991200065,-1.,0.764165902605995));
#33271=CARTESIAN_POINT('Ctrl Pts',(-1.82735991200065,1.,0.764165902605995));
#33272=CARTESIAN_POINT('Ctrl Pts',(-1.82131873145266,-1.,0.763673465462726));
#33273=CARTESIAN_POINT('Ctrl Pts',(-1.82131873145266,1.,0.763673465462726));
#33274=CARTESIAN_POINT('Ctrl Pts',(-1.8153211840553,-1.,0.763132003836634));
#33275=CARTESIAN_POINT('Ctrl Pts',(-1.8153211840553,1.,0.763132003836634));
#33276=CARTESIAN_POINT('Ctrl Pts',(-1.80938551463965,-1.,0.762546129463938));
#33277=CARTESIAN_POINT('Ctrl Pts',(-1.80938551463965,1.,0.762546129463938));
#33278=CARTESIAN_POINT('Ctrl Pts',(-1.80351583877342,-1.,0.761915336443547));
#33279=CARTESIAN_POINT('Ctrl Pts',(-1.80351583877342,1.,0.761915336443547));
#33280=CARTESIAN_POINT('Ctrl Pts',(-1.79768986997783,-1.,0.761229695230558));
#33281=CARTESIAN_POINT('Ctrl Pts',(-1.79768986997783,1.,0.761229695230558));
#33282=CARTESIAN_POINT('Ctrl Pts',(-1.7918581561088,-1.,0.760469555880749));
#33283=CARTESIAN_POINT('Ctrl Pts',(-1.7918581561088,1.,0.760469555880749));
#33284=CARTESIAN_POINT('Ctrl Pts',(-1.78596964884604,-1.,0.759614401110189));
#33285=CARTESIAN_POINT('Ctrl Pts',(-1.78596964884604,1.,0.759614401110189));
#33286=CARTESIAN_POINT('Ctrl Pts',(-1.77999411220945,-1.,0.758650626677518));
#33287=CARTESIAN_POINT('Ctrl Pts',(-1.77999411220945,1.,0.758650626677518));
#33288=CARTESIAN_POINT('Ctrl Pts',(-1.77394167108292,-1.,0.757578264077029));
#33289=CARTESIAN_POINT('Ctrl Pts',(-1.77394167108292,1.,0.757578264077029));
#33290=CARTESIAN_POINT('Ctrl Pts',(-1.76789396002998,-1.,0.75642189602781));
#33291=CARTESIAN_POINT('Ctrl Pts',(-1.76789396002998,1.,0.75642189602781));
#33292=CARTESIAN_POINT('Ctrl Pts',(-1.76197817240128,-1.,0.755220979974461));
#33293=CARTESIAN_POINT('Ctrl Pts',(-1.76197817240128,1.,0.755220979974461));
#33294=CARTESIAN_POINT('Ctrl Pts',(-1.75631083600019,-1.,0.754009254027829));
#33295=CARTESIAN_POINT('Ctrl Pts',(-1.75631083600019,1.,0.754009254027829));
#33296=CARTESIAN_POINT('Ctrl Pts',(-1.75095139468794,-1.,0.752797683531314));
#33297=CARTESIAN_POINT('Ctrl Pts',(-1.75095139468794,1.,0.752797683531314));
#33298=CARTESIAN_POINT('Ctrl Pts',(-1.74585086852502,-1.,0.751555614164482));
#33299=CARTESIAN_POINT('Ctrl Pts',(-1.74585086852502,1.,0.751555614164482));
#33300=CARTESIAN_POINT('Ctrl Pts',(-1.74080458267114,-1.,0.750193435981249));
#33301=CARTESIAN_POINT('Ctrl Pts',(-1.74080458267114,1.,0.750193435981249));
#33302=CARTESIAN_POINT('Ctrl Pts',(-1.7355035168033,-1.,0.74858246295687));
#33303=CARTESIAN_POINT('Ctrl Pts',(-1.7355035168033,1.,0.74858246295687));
#33304=CARTESIAN_POINT('Ctrl Pts',(-1.72958533647714,-1.,0.746574710097752));
#33305=CARTESIAN_POINT('Ctrl Pts',(-1.72958533647714,1.,0.746574710097752));
#33306=CARTESIAN_POINT('Ctrl Pts',(-1.72268229916769,-1.,0.744021445433093));
#33307=CARTESIAN_POINT('Ctrl Pts',(-1.72268229916769,1.,0.744021445433093));
#33308=CARTESIAN_POINT('Ctrl Pts',(-1.71447789751001,-1.,0.74079516202821));
#33309=CARTESIAN_POINT('Ctrl Pts',(-1.71447789751001,1.,0.74079516202821));
#33310=CARTESIAN_POINT('Ctrl Pts',(-1.70473309004249,-1.,0.736799665716932));
#33311=CARTESIAN_POINT('Ctrl Pts',(-1.70473309004249,1.,0.736799665716932));
#33312=CARTESIAN_POINT('Ctrl Pts',(-1.69326921972915,-1.,0.731963238685357));
#33313=CARTESIAN_POINT('Ctrl Pts',(-1.69326921972915,1.,0.731963238685357));
#33314=CARTESIAN_POINT('Ctrl Pts',(-1.67996158451922,-1.,0.726235967982445));
#33315=CARTESIAN_POINT('Ctrl Pts',(-1.67996158451922,1.,0.726235967982445));
#33316=CARTESIAN_POINT('Ctrl Pts',(-1.66472880551777,-1.,0.71958543378795));
#33317=CARTESIAN_POINT('Ctrl Pts',(-1.66472880551777,1.,0.71958543378795));
#33318=CARTESIAN_POINT('Ctrl Pts',(-1.64752408828442,-1.,0.711993139340447));
#33319=CARTESIAN_POINT('Ctrl Pts',(-1.64752408828442,1.,0.711993139340447));
#33320=CARTESIAN_POINT('Ctrl Pts',(-1.6321654166204,-1.,0.705159151977294));
#33321=CARTESIAN_POINT('Ctrl Pts',(-1.6321654166204,1.,0.705159151977294));
#33322=CARTESIAN_POINT('Ctrl Pts',(-1.61974673471117,-1.,0.699605146398837));
#33323=CARTESIAN_POINT('Ctrl Pts',(-1.61974673471117,1.,0.699605146398837));
#33324=CARTESIAN_POINT('Ctrl Pts',(-1.61106790957619,-1.,0.69571209787897));
#33325=CARTESIAN_POINT('Ctrl Pts',(-1.61106790957619,1.,0.69571209787897));
#33326=CARTESIAN_POINT('Ctrl Pts',(-1.60662857109684,-1.,0.693717979106305));
#33327=CARTESIAN_POINT('Ctrl Pts',(-1.60662857109684,1.,0.693717979106305));
#33328=CARTESIAN_POINT('',(-2.0698113262342,1.,0.7455743247944));
#33329=CARTESIAN_POINT('Ctrl Pts',(-2.0698113262342,1.,0.7455743247944));
#33330=CARTESIAN_POINT('Ctrl Pts',(-2.06854248895728,1.,0.745832791378367));
#33331=CARTESIAN_POINT('Ctrl Pts',(-2.06600523016815,1.,0.7463458715442));
#33332=CARTESIAN_POINT('Ctrl Pts',(-2.06220058927826,1.,0.747103932787919));
#33333=CARTESIAN_POINT('Ctrl Pts',(-2.05713023031006,1.,0.748091554183802));
#33334=CARTESIAN_POINT('Ctrl Pts',(-2.05079645592154,1.,0.749287468665046));
#33335=CARTESIAN_POINT('Ctrl Pts',(-2.04446689147979,1.,0.750444657875576));
#33336=CARTESIAN_POINT('Ctrl Pts',(-2.03814160092099,1.,0.751562963361115));
#33337=CARTESIAN_POINT('Ctrl Pts',(-2.03182068456221,1.,0.752642180487211));
#33338=CARTESIAN_POINT('Ctrl Pts',(-2.02550428623313,1.,0.753682061112768));
#33339=CARTESIAN_POINT('Ctrl Pts',(-2.01919259405809,1.,0.754682330722816));
#33340=CARTESIAN_POINT('Ctrl Pts',(-2.01288584328084,1.,0.755642704957865));
#33341=CARTESIAN_POINT('Ctrl Pts',(-2.0065843158773,1.,0.75656290464667));
#33342=CARTESIAN_POINT('Ctrl Pts',(-2.00028834739178,1.,0.757442676862724));
#33343=CARTESIAN_POINT('Ctrl Pts',(-1.99399831098817,1.,0.758281796766761));
#33344=CARTESIAN_POINT('Ctrl Pts',(-1.98771456680874,1.,0.759080037802488));
#33345=CARTESIAN_POINT('Ctrl Pts',(-1.98143741418172,1.,0.75983714745219));
#33346=CARTESIAN_POINT('Ctrl Pts',(-1.97516705321494,1.,0.760552825409757));
#33347=CARTESIAN_POINT('Ctrl Pts',(-1.96890351582499,1.,0.76122669048382));
#33348=CARTESIAN_POINT('Ctrl Pts',(-1.96264672744186,1.,0.761858300014423));
#33349=CARTESIAN_POINT('Ctrl Pts',(-1.95639665309869,1.,0.762447203806179));
#33350=CARTESIAN_POINT('Ctrl Pts',(-1.95015342590024,1.,0.762992990878769));
#33351=CARTESIAN_POINT('Ctrl Pts',(-1.9439174661764,1.,0.763495333538629));
#33352=CARTESIAN_POINT('Ctrl Pts',(-1.93768964875886,1.,0.763954049121458));
#33353=CARTESIAN_POINT('Ctrl Pts',(-1.93147105496382,1.,0.76436901067394));
#33354=CARTESIAN_POINT('Ctrl Pts',(-1.92526263537048,1.,0.764740025488211));
#33355=CARTESIAN_POINT('Ctrl Pts',(-1.91906491634196,1.,0.765066729667088));
#33356=CARTESIAN_POINT('Ctrl Pts',(-1.91287765805169,1.,0.765348465884722));
#33357=CARTESIAN_POINT('Ctrl Pts',(-1.90669961402356,1.,0.765584196937919));
#33358=CARTESIAN_POINT('Ctrl Pts',(-1.90052930393596,1.,0.765772772593386));
#33359=CARTESIAN_POINT('Ctrl Pts',(-1.89436577771388,1.,0.765913193856978));
#33360=CARTESIAN_POINT('Ctrl Pts',(-1.88820926433409,1.,0.766004837062091));
#33361=CARTESIAN_POINT('Ctrl Pts',(-1.88206215302561,1.,0.766047794851864));
#33362=CARTESIAN_POINT('Ctrl Pts',(-1.87592888967883,1.,0.766042837036744));
#33363=CARTESIAN_POINT('Ctrl Pts',(-1.86981398314341,1.,0.765990708546091));
#33364=CARTESIAN_POINT('Ctrl Pts',(-1.86372027063312,1.,0.765891519092547));
#33365=CARTESIAN_POINT('Ctrl Pts',(-1.85764741390394,1.,0.765744212909318));
#33366=CARTESIAN_POINT('Ctrl Pts',(-1.85158945130063,1.,0.765545710619062));
#33367=CARTESIAN_POINT('Ctrl Pts',(-1.84553698875924,1.,0.765291664862029));
#33368=CARTESIAN_POINT('Ctrl Pts',(-1.83948181064835,1.,0.764978057881737));
#33369=CARTESIAN_POINT('Ctrl Pts',(-1.83342077227142,1.,0.764602549687853));
#33370=CARTESIAN_POINT('Ctrl Pts',(-1.82735991200065,1.,0.764165902605995));
#33371=CARTESIAN_POINT('Ctrl Pts',(-1.82131873145266,1.,0.763673465462726));
#33372=CARTESIAN_POINT('Ctrl Pts',(-1.8153211840553,1.,0.763132003836634));
#33373=CARTESIAN_POINT('Ctrl Pts',(-1.80938551463965,1.,0.762546129463938));
#33374=CARTESIAN_POINT('Ctrl Pts',(-1.80351583877342,1.,0.761915336443547));
#33375=CARTESIAN_POINT('Ctrl Pts',(-1.79768986997783,1.,0.761229695230558));
#33376=CARTESIAN_POINT('Ctrl Pts',(-1.7918581561088,1.,0.760469555880749));
#33377=CARTESIAN_POINT('Ctrl Pts',(-1.78596964884604,1.,0.759614401110189));
#33378=CARTESIAN_POINT('Ctrl Pts',(-1.77999411220945,1.,0.758650626677518));
#33379=CARTESIAN_POINT('Ctrl Pts',(-1.77394167108292,1.,0.757578264077029));
#33380=CARTESIAN_POINT('Ctrl Pts',(-1.76789396002998,1.,0.75642189602781));
#33381=CARTESIAN_POINT('Ctrl Pts',(-1.76197817240128,1.,0.755220979974461));
#33382=CARTESIAN_POINT('Ctrl Pts',(-1.75631083600019,1.,0.754009254027829));
#33383=CARTESIAN_POINT('Ctrl Pts',(-1.75095139468794,1.,0.752797683531314));
#33384=CARTESIAN_POINT('Ctrl Pts',(-1.74585086852502,1.,0.751555614164482));
#33385=CARTESIAN_POINT('Ctrl Pts',(-1.74080458267114,1.,0.750193435981249));
#33386=CARTESIAN_POINT('Ctrl Pts',(-1.7355035168033,1.,0.74858246295687));
#33387=CARTESIAN_POINT('Ctrl Pts',(-1.72958533647714,1.,0.746574710097752));
#33388=CARTESIAN_POINT('Ctrl Pts',(-1.72268229916769,1.,0.744021445433093));
#33389=CARTESIAN_POINT('Ctrl Pts',(-1.71447789751001,1.,0.74079516202821));
#33390=CARTESIAN_POINT('Ctrl Pts',(-1.70473309004249,1.,0.736799665716932));
#33391=CARTESIAN_POINT('Ctrl Pts',(-1.69326921972915,1.,0.731963238685357));
#33392=CARTESIAN_POINT('Ctrl Pts',(-1.67996158451922,1.,0.726235967982445));
#33393=CARTESIAN_POINT('Ctrl Pts',(-1.66472880551777,1.,0.71958543378795));
#33394=CARTESIAN_POINT('Ctrl Pts',(-1.64752408828442,1.,0.711993139340447));
#33395=CARTESIAN_POINT('Ctrl Pts',(-1.6321654166204,1.,0.705159151977294));
#33396=CARTESIAN_POINT('Ctrl Pts',(-1.61974673471117,1.,0.699605146398837));
#33397=CARTESIAN_POINT('Ctrl Pts',(-1.61106790957619,1.,0.69571209787897));
#33398=CARTESIAN_POINT('Ctrl Pts',(-1.60662857109684,1.,0.693717979106305));
#33399=CARTESIAN_POINT('',(-2.0698113262342,0.,0.7455743247944));
#33400=CARTESIAN_POINT('Origin',(-2.11275013067528,0.,0.61342227326009));
#33401=CARTESIAN_POINT('',(-2.11275013067528,1.,0.61342227326009));
#33402=CARTESIAN_POINT('',(-2.0698113262342,1.,0.7455743247944));
#33403=CARTESIAN_POINT('',(-2.11275013067528,0.,0.61342227326009));
#33404=CARTESIAN_POINT('Ctrl Pts',(-1.7075470150345,-1.,0.383122945602004));
#33405=CARTESIAN_POINT('Ctrl Pts',(-1.7075470150345,1.,0.383122945602004));
#33406=CARTESIAN_POINT('Ctrl Pts',(-1.71231062891958,-1.,0.384119047315542));
#33407=CARTESIAN_POINT('Ctrl Pts',(-1.71231062891958,1.,0.384119047315542));
#33408=CARTESIAN_POINT('Ctrl Pts',(-1.72162022246158,-1.,0.38607079032701));
#33409=CARTESIAN_POINT('Ctrl Pts',(-1.72162022246158,1.,0.38607079032701));
#33410=CARTESIAN_POINT('Ctrl Pts',(-1.7349317097561,-1.,0.388877023509191));
#33411=CARTESIAN_POINT('Ctrl Pts',(-1.7349317097561,1.,0.388877023509191));
#33412=CARTESIAN_POINT('Ctrl Pts',(-1.75137405313962,-1.,0.392375812294307));
#33413=CARTESIAN_POINT('Ctrl Pts',(-1.75137405313962,1.,0.392375812294307));
#33414=CARTESIAN_POINT('Ctrl Pts',(-1.7697556004756,-1.,0.39634619612042));
#33415=CARTESIAN_POINT('Ctrl Pts',(-1.7697556004756,1.,0.39634619612042));
#33416=CARTESIAN_POINT('Ctrl Pts',(-1.78598826347533,-1.,0.39991940378308));
#33417=CARTESIAN_POINT('Ctrl Pts',(-1.78598826347533,1.,0.39991940378308));
#33418=CARTESIAN_POINT('Ctrl Pts',(-1.80012077176221,-1.,0.403107976170441));
#33419=CARTESIAN_POINT('Ctrl Pts',(-1.80012077176221,1.,0.403107976170441));
#33420=CARTESIAN_POINT('Ctrl Pts',(-1.81223801813988,-1.,0.405933518411838));
#33421=CARTESIAN_POINT('Ctrl Pts',(-1.81223801813988,1.,0.405933518411838));
#33422=CARTESIAN_POINT('Ctrl Pts',(-1.8224702267854,-1.,0.408428948108533));
#33423=CARTESIAN_POINT('Ctrl Pts',(-1.8224702267854,1.,0.408428948108533));
#33424=CARTESIAN_POINT('Ctrl Pts',(-1.83100408895216,-1.,0.410641256301675));
#33425=CARTESIAN_POINT('Ctrl Pts',(-1.83100408895216,1.,0.410641256301675));
#33426=CARTESIAN_POINT('Ctrl Pts',(-1.83808953475839,-1.,0.412633125322161));
#33427=CARTESIAN_POINT('Ctrl Pts',(-1.83808953475839,1.,0.412633125322161));
#33428=CARTESIAN_POINT('Ctrl Pts',(-1.8440575707371,-1.,0.41448743825434));
#33429=CARTESIAN_POINT('Ctrl Pts',(-1.8440575707371,1.,0.41448743825434));
#33430=CARTESIAN_POINT('Ctrl Pts',(-1.84929312929882,-1.,0.416300022038864));
#33431=CARTESIAN_POINT('Ctrl Pts',(-1.84929312929882,1.,0.416300022038864));
#33432=CARTESIAN_POINT('Ctrl Pts',(-1.85417632856234,-1.,0.418164129143534));
#33433=CARTESIAN_POINT('Ctrl Pts',(-1.85417632856234,1.,0.418164129143534));
#33434=CARTESIAN_POINT('Ctrl Pts',(-1.85903281096686,-1.,0.420157287975619));
#33435=CARTESIAN_POINT('Ctrl Pts',(-1.85903281096686,1.,0.420157287975619));
#33436=CARTESIAN_POINT('Ctrl Pts',(-1.86408083334028,-1.,0.422327307418275));
#33437=CARTESIAN_POINT('Ctrl Pts',(-1.86408083334028,1.,0.422327307418275));
#33438=CARTESIAN_POINT('Ctrl Pts',(-1.86937803944323,-1.,0.424678177291359));
#33439=CARTESIAN_POINT('Ctrl Pts',(-1.86937803944323,1.,0.424678177291359));
#33440=CARTESIAN_POINT('Ctrl Pts',(-1.87486989291484,-1.,0.427183828519102));
#33441=CARTESIAN_POINT('Ctrl Pts',(-1.87486989291484,1.,0.427183828519102));
#33442=CARTESIAN_POINT('Ctrl Pts',(-1.88044229001832,-1.,0.429803062482344));
#33443=CARTESIAN_POINT('Ctrl Pts',(-1.88044229001832,1.,0.429803062482344));
#33444=CARTESIAN_POINT('Ctrl Pts',(-1.88596913666793,-1.,0.432493038548748));
#33445=CARTESIAN_POINT('Ctrl Pts',(-1.88596913666793,1.,0.432493038548748));
#33446=CARTESIAN_POINT('Ctrl Pts',(-1.89136993975504,-1.,0.435225660963383));
#33447=CARTESIAN_POINT('Ctrl Pts',(-1.89136993975504,1.,0.435225660963383));
#33448=CARTESIAN_POINT('Ctrl Pts',(-1.89663648956466,-1.,0.437995003948244));
#33449=CARTESIAN_POINT('Ctrl Pts',(-1.89663648956466,1.,0.437995003948244));
#33450=CARTESIAN_POINT('Ctrl Pts',(-1.90180124389086,-1.,0.440807833704038));
#33451=CARTESIAN_POINT('Ctrl Pts',(-1.90180124389086,1.,0.440807833704038));
#33452=CARTESIAN_POINT('Ctrl Pts',(-1.90691756144898,-1.,0.44367755684915));
#33453=CARTESIAN_POINT('Ctrl Pts',(-1.90691756144898,1.,0.44367755684915));
#33454=CARTESIAN_POINT('Ctrl Pts',(-1.9120369998112,-1.,0.446617343485711));
#33455=CARTESIAN_POINT('Ctrl Pts',(-1.9120369998112,1.,0.446617343485711));
#33456=CARTESIAN_POINT('Ctrl Pts',(-1.91718342555755,-1.,0.449632260106662));
#33457=CARTESIAN_POINT('Ctrl Pts',(-1.91718342555755,1.,0.449632260106662));
#33458=CARTESIAN_POINT('Ctrl Pts',(-1.92235380648502,-1.,0.452719478359432));
#33459=CARTESIAN_POINT('Ctrl Pts',(-1.92235380648502,1.,0.452719478359432));
#33460=CARTESIAN_POINT('Ctrl Pts',(-1.92753067150476,-1.,0.455872005174371));
#33461=CARTESIAN_POINT('Ctrl Pts',(-1.92753067150476,1.,0.455872005174371));
#33462=CARTESIAN_POINT('Ctrl Pts',(-1.93269066517934,-1.,0.459081234547926));
#33463=CARTESIAN_POINT('Ctrl Pts',(-1.93269066517934,1.,0.459081234547926));
#33464=CARTESIAN_POINT('Ctrl Pts',(-1.93781486640821,-1.,0.462340031009056));
#33465=CARTESIAN_POINT('Ctrl Pts',(-1.93781486640821,1.,0.462340031009056));
#33466=CARTESIAN_POINT('Ctrl Pts',(-1.9428979419619,-1.,0.46564546202603));
#33467=CARTESIAN_POINT('Ctrl Pts',(-1.9428979419619,1.,0.46564546202603));
#33468=CARTESIAN_POINT('Ctrl Pts',(-1.94794381136514,-1.,0.468997482913135));
#33469=CARTESIAN_POINT('Ctrl Pts',(-1.94794381136514,1.,0.468997482913135));
#33470=CARTESIAN_POINT('Ctrl Pts',(-1.95296148278133,-1.,0.472397672264072));
#33471=CARTESIAN_POINT('Ctrl Pts',(-1.95296148278133,1.,0.472397672264072));
#33472=CARTESIAN_POINT('Ctrl Pts',(-1.95796111148177,-1.,0.475848034683176));
#33473=CARTESIAN_POINT('Ctrl Pts',(-1.95796111148177,1.,0.475848034683176));
#33474=CARTESIAN_POINT('Ctrl Pts',(-1.96294933055943,-1.,0.479349583074855));
#33475=CARTESIAN_POINT('Ctrl Pts',(-1.96294933055943,1.,0.479349583074855));
#33476=CARTESIAN_POINT('Ctrl Pts',(-1.96792703422362,-1.,0.48290166212069));
#33477=CARTESIAN_POINT('Ctrl Pts',(-1.96792703422362,1.,0.48290166212069));
#33478=CARTESIAN_POINT('Ctrl Pts',(-1.97289186263272,-1.,0.486502692907659));
#33479=CARTESIAN_POINT('Ctrl Pts',(-1.97289186263272,1.,0.486502692907659));
#33480=CARTESIAN_POINT('Ctrl Pts',(-1.97783973019229,-1.,0.490150627860952));
#33481=CARTESIAN_POINT('Ctrl Pts',(-1.97783973019229,1.,0.490150627860952));
#33482=CARTESIAN_POINT('Ctrl Pts',(-1.98276658761821,-1.,0.493843476541494));
#33483=CARTESIAN_POINT('Ctrl Pts',(-1.98276658761821,1.,0.493843476541494));
#33484=CARTESIAN_POINT('Ctrl Pts',(-1.98767044752932,-1.,0.497579909545574));
#33485=CARTESIAN_POINT('Ctrl Pts',(-1.98767044752932,1.,0.497579909545574));
#33486=CARTESIAN_POINT('Ctrl Pts',(-1.99255149126155,-1.,0.501359287727146));
#33487=CARTESIAN_POINT('Ctrl Pts',(-1.99255149126155,1.,0.501359287727146));
#33488=CARTESIAN_POINT('Ctrl Pts',(-1.99741107463572,-1.,0.505181361323026));
#33489=CARTESIAN_POINT('Ctrl Pts',(-1.99741107463572,1.,0.505181361323026));
#33490=CARTESIAN_POINT('Ctrl Pts',(-2.00225107134734,-1.,0.509046069886157));
#33491=CARTESIAN_POINT('Ctrl Pts',(-2.00225107134734,1.,0.509046069886157));
#33492=CARTESIAN_POINT('Ctrl Pts',(-2.00707309946949,-1.,0.512953306961792));
#33493=CARTESIAN_POINT('Ctrl Pts',(-2.00707309946949,1.,0.512953306961792));
#33494=CARTESIAN_POINT('Ctrl Pts',(-2.01187773939242,-1.,0.516902681728687));
#33495=CARTESIAN_POINT('Ctrl Pts',(-2.01187773939242,1.,0.516902681728687));
#33496=CARTESIAN_POINT('Ctrl Pts',(-2.01666477917286,-1.,0.52089359039937));
#33497=CARTESIAN_POINT('Ctrl Pts',(-2.01666477917286,1.,0.52089359039937));
#33498=CARTESIAN_POINT('Ctrl Pts',(-2.02143356304698,-1.,0.524925318333476));
#33499=CARTESIAN_POINT('Ctrl Pts',(-2.02143356304698,1.,0.524925318333476));
#33500=CARTESIAN_POINT('Ctrl Pts',(-2.0261832908329,-1.,0.528997127241914));
#33501=CARTESIAN_POINT('Ctrl Pts',(-2.0261832908329,1.,0.528997127241914));
#33502=CARTESIAN_POINT('Ctrl Pts',(-2.03091336214426,-1.,0.533108355132976));
#33503=CARTESIAN_POINT('Ctrl Pts',(-2.03091336214426,1.,0.533108355132976));
#33504=CARTESIAN_POINT('Ctrl Pts',(-2.03562362954037,-1.,0.537258489833262));
#33505=CARTESIAN_POINT('Ctrl Pts',(-2.03562362954037,1.,0.537258489833262));
#33506=CARTESIAN_POINT('Ctrl Pts',(-2.04031422690527,-1.,0.541447120615659));
#33507=CARTESIAN_POINT('Ctrl Pts',(-2.04031422690527,1.,0.541447120615659));
#33508=CARTESIAN_POINT('Ctrl Pts',(-2.04498544714588,-1.,0.54567390381743));
#33509=CARTESIAN_POINT('Ctrl Pts',(-2.04498544714588,1.,0.54567390381743));
#33510=CARTESIAN_POINT('Ctrl Pts',(-2.04963761077958,-1.,0.549938525150295));
#33511=CARTESIAN_POINT('Ctrl Pts',(-2.04963761077958,1.,0.549938525150295));
#33512=CARTESIAN_POINT('Ctrl Pts',(-2.05427091604413,-1.,0.554240657463906));
#33513=CARTESIAN_POINT('Ctrl Pts',(-2.05427091604413,1.,0.554240657463906));
#33514=CARTESIAN_POINT('Ctrl Pts',(-2.05888537756462,-1.,0.558579940185151));
#33515=CARTESIAN_POINT('Ctrl Pts',(-2.05888537756462,1.,0.558579940185151));
#33516=CARTESIAN_POINT('Ctrl Pts',(-2.06348090160589,-1.,0.562955993082261));
#33517=CARTESIAN_POINT('Ctrl Pts',(-2.06348090160589,1.,0.562955993082261));
#33518=CARTESIAN_POINT('Ctrl Pts',(-2.06805732997334,-1.,0.567368421181087));
#33519=CARTESIAN_POINT('Ctrl Pts',(-2.06805732997334,1.,0.567368421181087));
#33520=CARTESIAN_POINT('Ctrl Pts',(-2.07261449292824,-1.,0.571816823242603));
#33521=CARTESIAN_POINT('Ctrl Pts',(-2.07261449292824,1.,0.571816823242603));
#33522=CARTESIAN_POINT('Ctrl Pts',(-2.07715226767559,-1.,0.576300797416844));
#33523=CARTESIAN_POINT('Ctrl Pts',(-2.07715226767559,1.,0.576300797416844));
#33524=CARTESIAN_POINT('Ctrl Pts',(-2.08167059018418,-1.,0.580819952108063));
#33525=CARTESIAN_POINT('Ctrl Pts',(-2.08167059018418,1.,0.580819952108063));
#33526=CARTESIAN_POINT('Ctrl Pts',(-2.08616943727951,-1.,0.585373918991617));
#33527=CARTESIAN_POINT('Ctrl Pts',(-2.08616943727951,1.,0.585373918991617));
#33528=CARTESIAN_POINT('Ctrl Pts',(-2.09064881812129,-1.,0.589962365403406));
#33529=CARTESIAN_POINT('Ctrl Pts',(-2.09064881812129,1.,0.589962365403406));
#33530=CARTESIAN_POINT('Ctrl Pts',(-2.0951087622027,-1.,0.594585006052162));
#33531=CARTESIAN_POINT('Ctrl Pts',(-2.0951087622027,1.,0.594585006052162));
#33532=CARTESIAN_POINT('Ctrl Pts',(-2.0995493086477,-1.,0.599241616420533));
#33533=CARTESIAN_POINT('Ctrl Pts',(-2.0995493086477,1.,0.599241616420533));
#33534=CARTESIAN_POINT('Ctrl Pts',(-2.10397049886949,-1.,0.60393203073603));
#33535=CARTESIAN_POINT('Ctrl Pts',(-2.10397049886949,1.,0.60393203073603));
#33536=CARTESIAN_POINT('Ctrl Pts',(-2.1074919961518,-1.,0.607711315454876));
#33537=CARTESIAN_POINT('Ctrl Pts',(-2.1074919961518,1.,0.607711315454876));
#33538=CARTESIAN_POINT('Ctrl Pts',(-2.11012443807238,-1.,0.610560911689899));
#33539=CARTESIAN_POINT('Ctrl Pts',(-2.11012443807238,1.,0.610560911689899));
#33540=CARTESIAN_POINT('Ctrl Pts',(-2.11187554259986,-1.,0.6124673655618));
#33541=CARTESIAN_POINT('Ctrl Pts',(-2.11187554259986,1.,0.6124673655618));
#33542=CARTESIAN_POINT('Ctrl Pts',(-2.11275013067528,-1.,0.61342227326009));
#33543=CARTESIAN_POINT('Ctrl Pts',(-2.11275013067528,1.,0.61342227326009));
#33544=CARTESIAN_POINT('',(-1.7075470150345,1.,0.383122945602004));
#33545=CARTESIAN_POINT('Ctrl Pts',(-1.7075470150345,1.,0.383122945602004));
#33546=CARTESIAN_POINT('Ctrl Pts',(-1.71231062891958,1.,0.384119047315542));
#33547=CARTESIAN_POINT('Ctrl Pts',(-1.72162022246158,1.,0.38607079032701));
#33548=CARTESIAN_POINT('Ctrl Pts',(-1.7349317097561,1.,0.388877023509191));
#33549=CARTESIAN_POINT('Ctrl Pts',(-1.75137405313962,1.,0.392375812294307));
#33550=CARTESIAN_POINT('Ctrl Pts',(-1.7697556004756,1.,0.39634619612042));
#33551=CARTESIAN_POINT('Ctrl Pts',(-1.78598826347533,1.,0.39991940378308));
#33552=CARTESIAN_POINT('Ctrl Pts',(-1.80012077176221,1.,0.403107976170441));
#33553=CARTESIAN_POINT('Ctrl Pts',(-1.81223801813988,1.,0.405933518411838));
#33554=CARTESIAN_POINT('Ctrl Pts',(-1.8224702267854,1.,0.408428948108533));
#33555=CARTESIAN_POINT('Ctrl Pts',(-1.83100408895216,1.,0.410641256301675));
#33556=CARTESIAN_POINT('Ctrl Pts',(-1.83808953475839,1.,0.412633125322161));
#33557=CARTESIAN_POINT('Ctrl Pts',(-1.8440575707371,1.,0.41448743825434));
#33558=CARTESIAN_POINT('Ctrl Pts',(-1.84929312929882,1.,0.416300022038864));
#33559=CARTESIAN_POINT('Ctrl Pts',(-1.85417632856234,1.,0.418164129143534));
#33560=CARTESIAN_POINT('Ctrl Pts',(-1.85903281096686,1.,0.420157287975619));
#33561=CARTESIAN_POINT('Ctrl Pts',(-1.86408083334028,1.,0.422327307418275));
#33562=CARTESIAN_POINT('Ctrl Pts',(-1.86937803944323,1.,0.424678177291359));
#33563=CARTESIAN_POINT('Ctrl Pts',(-1.87486989291484,1.,0.427183828519102));
#33564=CARTESIAN_POINT('Ctrl Pts',(-1.88044229001832,1.,0.429803062482344));
#33565=CARTESIAN_POINT('Ctrl Pts',(-1.88596913666793,1.,0.432493038548748));
#33566=CARTESIAN_POINT('Ctrl Pts',(-1.89136993975504,1.,0.435225660963383));
#33567=CARTESIAN_POINT('Ctrl Pts',(-1.89663648956466,1.,0.437995003948244));
#33568=CARTESIAN_POINT('Ctrl Pts',(-1.90180124389086,1.,0.440807833704038));
#33569=CARTESIAN_POINT('Ctrl Pts',(-1.90691756144898,1.,0.44367755684915));
#33570=CARTESIAN_POINT('Ctrl Pts',(-1.9120369998112,1.,0.446617343485711));
#33571=CARTESIAN_POINT('Ctrl Pts',(-1.91718342555755,1.,0.449632260106662));
#33572=CARTESIAN_POINT('Ctrl Pts',(-1.92235380648502,1.,0.452719478359432));
#33573=CARTESIAN_POINT('Ctrl Pts',(-1.92753067150476,1.,0.455872005174371));
#33574=CARTESIAN_POINT('Ctrl Pts',(-1.93269066517934,1.,0.459081234547926));
#33575=CARTESIAN_POINT('Ctrl Pts',(-1.93781486640821,1.,0.462340031009056));
#33576=CARTESIAN_POINT('Ctrl Pts',(-1.9428979419619,1.,0.46564546202603));
#33577=CARTESIAN_POINT('Ctrl Pts',(-1.94794381136514,1.,0.468997482913135));
#33578=CARTESIAN_POINT('Ctrl Pts',(-1.95296148278133,1.,0.472397672264072));
#33579=CARTESIAN_POINT('Ctrl Pts',(-1.95796111148177,1.,0.475848034683176));
#33580=CARTESIAN_POINT('Ctrl Pts',(-1.96294933055943,1.,0.479349583074855));
#33581=CARTESIAN_POINT('Ctrl Pts',(-1.96792703422362,1.,0.48290166212069));
#33582=CARTESIAN_POINT('Ctrl Pts',(-1.97289186263272,1.,0.486502692907659));
#33583=CARTESIAN_POINT('Ctrl Pts',(-1.97783973019229,1.,0.490150627860952));
#33584=CARTESIAN_POINT('Ctrl Pts',(-1.98276658761821,1.,0.493843476541494));
#33585=CARTESIAN_POINT('Ctrl Pts',(-1.98767044752932,1.,0.497579909545574));
#33586=CARTESIAN_POINT('Ctrl Pts',(-1.99255149126155,1.,0.501359287727146));
#33587=CARTESIAN_POINT('Ctrl Pts',(-1.99741107463572,1.,0.505181361323026));
#33588=CARTESIAN_POINT('Ctrl Pts',(-2.00225107134734,1.,0.509046069886157));
#33589=CARTESIAN_POINT('Ctrl Pts',(-2.00707309946949,1.,0.512953306961792));
#33590=CARTESIAN_POINT('Ctrl Pts',(-2.01187773939242,1.,0.516902681728687));
#33591=CARTESIAN_POINT('Ctrl Pts',(-2.01666477917286,1.,0.52089359039937));
#33592=CARTESIAN_POINT('Ctrl Pts',(-2.02143356304698,1.,0.524925318333476));
#33593=CARTESIAN_POINT('Ctrl Pts',(-2.0261832908329,1.,0.528997127241914));
#33594=CARTESIAN_POINT('Ctrl Pts',(-2.03091336214426,1.,0.533108355132976));
#33595=CARTESIAN_POINT('Ctrl Pts',(-2.03562362954037,1.,0.537258489833262));
#33596=CARTESIAN_POINT('Ctrl Pts',(-2.04031422690527,1.,0.541447120615659));
#33597=CARTESIAN_POINT('Ctrl Pts',(-2.04498544714588,1.,0.54567390381743));
#33598=CARTESIAN_POINT('Ctrl Pts',(-2.04963761077958,1.,0.549938525150295));
#33599=CARTESIAN_POINT('Ctrl Pts',(-2.05427091604413,1.,0.554240657463906));
#33600=CARTESIAN_POINT('Ctrl Pts',(-2.05888537756462,1.,0.558579940185151));
#33601=CARTESIAN_POINT('Ctrl Pts',(-2.06348090160589,1.,0.562955993082261));
#33602=CARTESIAN_POINT('Ctrl Pts',(-2.06805732997334,1.,0.567368421181087));
#33603=CARTESIAN_POINT('Ctrl Pts',(-2.07261449292824,1.,0.571816823242603));
#33604=CARTESIAN_POINT('Ctrl Pts',(-2.07715226767559,1.,0.576300797416844));
#33605=CARTESIAN_POINT('Ctrl Pts',(-2.08167059018418,1.,0.580819952108063));
#33606=CARTESIAN_POINT('Ctrl Pts',(-2.08616943727951,1.,0.585373918991617));
#33607=CARTESIAN_POINT('Ctrl Pts',(-2.09064881812129,1.,0.589962365403406));
#33608=CARTESIAN_POINT('Ctrl Pts',(-2.0951087622027,1.,0.594585006052162));
#33609=CARTESIAN_POINT('Ctrl Pts',(-2.0995493086477,1.,0.599241616420533));
#33610=CARTESIAN_POINT('Ctrl Pts',(-2.10397049886949,1.,0.60393203073603));
#33611=CARTESIAN_POINT('Ctrl Pts',(-2.1074919961518,1.,0.607711315454876));
#33612=CARTESIAN_POINT('Ctrl Pts',(-2.11012443807238,1.,0.610560911689899));
#33613=CARTESIAN_POINT('Ctrl Pts',(-2.11187554259986,1.,0.6124673655618));
#33614=CARTESIAN_POINT('Ctrl Pts',(-2.11275013067528,1.,0.61342227326009));
#33615=CARTESIAN_POINT('',(-1.7075470150345,0.,0.383122945602003));
#33616=CARTESIAN_POINT('Origin',(0.,0.,0.));
#33617=CARTESIAN_POINT('',(-1.74236521665491,1.,0.163289472382896));
#33618=CARTESIAN_POINT('Origin',(0.,1.,0.));
#33619=CARTESIAN_POINT('',(-1.74236521665491,0.,0.163289472382896));
#33620=CARTESIAN_POINT('Ctrl Pts',(-2.19890268624765,-1.,0.069476445021958));
#33621=CARTESIAN_POINT('Ctrl Pts',(-2.19890268624765,1.,0.069476445021958));
#33622=CARTESIAN_POINT('Ctrl Pts',(-2.19777582085423,-1.,0.0701143536325489));
#33623=CARTESIAN_POINT('Ctrl Pts',(-2.19777582085423,1.,0.0701143536325489));
#33624=CARTESIAN_POINT('Ctrl Pts',(-2.19552129484002,-1.,0.0713863779526153));
#33625=CARTESIAN_POINT('Ctrl Pts',(-2.19552129484002,1.,0.0713863779526153));
#33626=CARTESIAN_POINT('Ctrl Pts',(-2.19213712013662,-1.,0.0732830357306724));
#33627=CARTESIAN_POINT('Ctrl Pts',(-2.19213712013662,1.,0.0732830357306724));
#33628=CARTESIAN_POINT('Ctrl Pts',(-2.1876201139953,-1.,0.0757891465836146));
#33629=CARTESIAN_POINT('Ctrl Pts',(-2.1876201139953,1.,0.0757891465836146));
#33630=CARTESIAN_POINT('Ctrl Pts',(-2.18196589448887,-1.,0.0788837727685241));
#33631=CARTESIAN_POINT('Ctrl Pts',(-2.18196589448887,1.,0.0788837727685241));
#33632=CARTESIAN_POINT('Ctrl Pts',(-2.176303712113,-1.,0.0819402680872764));
#33633=CARTESIAN_POINT('Ctrl Pts',(-2.176303712113,1.,0.0819402680872764));
#33634=CARTESIAN_POINT('Ctrl Pts',(-2.17063357870952,-1.,0.0849584620835371));
#33635=CARTESIAN_POINT('Ctrl Pts',(-2.17063357870952,1.,0.0849584620835371));
#33636=CARTESIAN_POINT('Ctrl Pts',(-2.16495552645014,-1.,0.0879381291386921));
#33637=CARTESIAN_POINT('Ctrl Pts',(-2.16495552645014,1.,0.0879381291386921));
#33638=CARTESIAN_POINT('Ctrl Pts',(-2.15926961544516,-1.,0.0908789888107264));
#33639=CARTESIAN_POINT('Ctrl Pts',(-2.15926961544516,1.,0.0908789888107264));
#33640=CARTESIAN_POINT('Ctrl Pts',(-2.1535759397817,-1.,0.0937807218867642));
#33641=CARTESIAN_POINT('Ctrl Pts',(-2.1535759397817,1.,0.0937807218867642));
#33642=CARTESIAN_POINT('Ctrl Pts',(-2.14787463531795,-1.,0.0966429852305457));
#33643=CARTESIAN_POINT('Ctrl Pts',(-2.14787463531795,1.,0.0966429852305457));
#33644=CARTESIAN_POINT('Ctrl Pts',(-2.14216588396025,-1.,0.0994654261990914));
#33645=CARTESIAN_POINT('Ctrl Pts',(-2.14216588396025,1.,0.0994654261990914));
#33646=CARTESIAN_POINT('Ctrl Pts',(-2.13644992667165,-1.,0.1022477005561));
#33647=CARTESIAN_POINT('Ctrl Pts',(-2.13644992667165,1.,0.1022477005561));
#33648=CARTESIAN_POINT('Ctrl Pts',(-2.13072704887293,-1.,0.104989479152739));
#33649=CARTESIAN_POINT('Ctrl Pts',(-2.13072704887293,1.,0.104989479152739));
#33650=CARTESIAN_POINT('Ctrl Pts',(-2.12499752307,-1.,0.10769043523109));
#33651=CARTESIAN_POINT('Ctrl Pts',(-2.12499752307,1.,0.10769043523109));
#33652=CARTESIAN_POINT('Ctrl Pts',(-2.11926155590865,-1.,0.110350236135025));
#33653=CARTESIAN_POINT('Ctrl Pts',(-2.11926155590865,1.,0.110350236135025));
#33654=CARTESIAN_POINT('Ctrl Pts',(-2.11351924490306,-1.,0.112968534419737));
#33655=CARTESIAN_POINT('Ctrl Pts',(-2.11351924490306,1.,0.112968534419737));
#33656=CARTESIAN_POINT('Ctrl Pts',(-2.10777050261309,-1.,0.115544957687926));
#33657=CARTESIAN_POINT('Ctrl Pts',(-2.10777050261309,1.,0.115544957687926));
#33658=CARTESIAN_POINT('Ctrl Pts',(-2.102015121329,-1.,0.118079107988355));
#33659=CARTESIAN_POINT('Ctrl Pts',(-2.102015121329,1.,0.118079107988355));
#33660=CARTESIAN_POINT('Ctrl Pts',(-2.0962529286773,-1.,0.120570567965122));
#33661=CARTESIAN_POINT('Ctrl Pts',(-2.0962529286773,1.,0.120570567965122));
#33662=CARTESIAN_POINT('Ctrl Pts',(-2.09048392424825,-1.,0.123018905621083));
#33663=CARTESIAN_POINT('Ctrl Pts',(-2.09048392424825,1.,0.123018905621083));
#33664=CARTESIAN_POINT('Ctrl Pts',(-2.08470840653643,-1.,0.125423679412061));
#33665=CARTESIAN_POINT('Ctrl Pts',(-2.08470840653643,1.,0.125423679412061));
#33666=CARTESIAN_POINT('Ctrl Pts',(-2.07892715110987,-1.,0.12778444527612));
#33667=CARTESIAN_POINT('Ctrl Pts',(-2.07892715110987,1.,0.12778444527612));
#33668=CARTESIAN_POINT('Ctrl Pts',(-2.07314114713063,-1.,0.130100748328403));
#33669=CARTESIAN_POINT('Ctrl Pts',(-2.07314114713063,1.,0.130100748328403));
#33670=CARTESIAN_POINT('Ctrl Pts',(-2.06735123910326,-1.,0.13237211154771));
#33671=CARTESIAN_POINT('Ctrl Pts',(-2.06735123910326,1.,0.13237211154771));
#33672=CARTESIAN_POINT('Ctrl Pts',(-2.06155781517842,-1.,0.134598026192106));
#33673=CARTESIAN_POINT('Ctrl Pts',(-2.06155781517842,1.,0.134598026192106));
#33674=CARTESIAN_POINT('Ctrl Pts',(-2.05576044414264,-1.,0.136777941218043));
#33675=CARTESIAN_POINT('Ctrl Pts',(-2.05576044414264,1.,0.136777941218043));
#33676=CARTESIAN_POINT('Ctrl Pts',(-2.04995762001328,-1.,0.138911255368966));
#33677=CARTESIAN_POINT('Ctrl Pts',(-2.04995762001328,1.,0.138911255368966));
#33678=CARTESIAN_POINT('Ctrl Pts',(-2.04414757947916,-1.,0.140997332152546));
#33679=CARTESIAN_POINT('Ctrl Pts',(-2.04414757947916,1.,0.140997332152546));
#33680=CARTESIAN_POINT('Ctrl Pts',(-2.03832911025912,-1.,0.143035515058209));
#33681=CARTESIAN_POINT('Ctrl Pts',(-2.03832911025912,1.,0.143035515058209));
#33682=CARTESIAN_POINT('Ctrl Pts',(-2.03250223739942,-1.,0.145025140186057));
#33683=CARTESIAN_POINT('Ctrl Pts',(-2.03250223739942,1.,0.145025140186057));
#33684=CARTESIAN_POINT('Ctrl Pts',(-2.02666926182017,-1.,0.146965557332583));
#33685=CARTESIAN_POINT('Ctrl Pts',(-2.02666926182017,1.,0.146965557332583));
#33686=CARTESIAN_POINT('Ctrl Pts',(-2.02083464969894,-1.,0.148856124775337));
#33687=CARTESIAN_POINT('Ctrl Pts',(-2.02083464969894,1.,0.148856124775337));
#33688=CARTESIAN_POINT('Ctrl Pts',(-2.01500291940238,-1.,0.150696157673078));
#33689=CARTESIAN_POINT('Ctrl Pts',(-2.01500291940238,1.,0.150696157673078));
#33690=CARTESIAN_POINT('Ctrl Pts',(-2.00917680318424,-1.,0.15248488362145));
#33691=CARTESIAN_POINT('Ctrl Pts',(-2.00917680318424,1.,0.15248488362145));
#33692=CARTESIAN_POINT('Ctrl Pts',(-2.00335565310543,-1.,0.154221403049722));
#33693=CARTESIAN_POINT('Ctrl Pts',(-2.00335565310543,1.,0.154221403049722));
#33694=CARTESIAN_POINT('Ctrl Pts',(-1.99753284771497,-1.,0.155904629548783));
#33695=CARTESIAN_POINT('Ctrl Pts',(-1.99753284771497,1.,0.155904629548783));
#33696=CARTESIAN_POINT('Ctrl Pts',(-1.99169810931908,-1.,0.157533331459227));
#33697=CARTESIAN_POINT('Ctrl Pts',(-1.99169810931908,1.,0.157533331459227));
#33698=CARTESIAN_POINT('Ctrl Pts',(-1.98584238283292,-1.,0.159106226437299));
#33699=CARTESIAN_POINT('Ctrl Pts',(-1.98584238283292,1.,0.159106226437299));
#33700=CARTESIAN_POINT('Ctrl Pts',(-1.97996195437559,-1.,0.160622060784611));
#33701=CARTESIAN_POINT('Ctrl Pts',(-1.97996195437559,1.,0.160622060784611));
#33702=CARTESIAN_POINT('Ctrl Pts',(-1.97406280235188,-1.,0.162079693556288));
#33703=CARTESIAN_POINT('Ctrl Pts',(-1.97406280235188,1.,0.162079693556288));
#33704=CARTESIAN_POINT('Ctrl Pts',(-1.96816512677967,-1.,0.163478185457734));
#33705=CARTESIAN_POINT('Ctrl Pts',(-1.96816512677967,1.,0.163478185457734));
#33706=CARTESIAN_POINT('Ctrl Pts',(-1.96229379940136,-1.,0.164816568920269));
#33707=CARTESIAN_POINT('Ctrl Pts',(-1.96229379940136,1.,0.164816568920269));
#33708=CARTESIAN_POINT('Ctrl Pts',(-1.9564675971873,-1.,0.166093592002812));
#33709=CARTESIAN_POINT('Ctrl Pts',(-1.9564675971873,1.,0.166093592002812));
#33710=CARTESIAN_POINT('Ctrl Pts',(-1.95069027794294,-1.,0.167307501784475));
#33711=CARTESIAN_POINT('Ctrl Pts',(-1.95069027794294,1.,0.167307501784475));
#33712=CARTESIAN_POINT('Ctrl Pts',(-1.94493757756931,-1.,0.168455741607556));
#33713=CARTESIAN_POINT('Ctrl Pts',(-1.94493757756931,1.,0.168455741607556));
#33714=CARTESIAN_POINT('Ctrl Pts',(-1.93915639211581,-1.,0.169534904817491));
#33715=CARTESIAN_POINT('Ctrl Pts',(-1.93915639211581,1.,0.169534904817491));
#33716=CARTESIAN_POINT('Ctrl Pts',(-1.93329183155539,-1.,0.170541253116201));
#33717=CARTESIAN_POINT('Ctrl Pts',(-1.93329183155539,1.,0.170541253116201));
#33718=CARTESIAN_POINT('Ctrl Pts',(-1.92731093582036,-1.,0.171471191532988));
#33719=CARTESIAN_POINT('Ctrl Pts',(-1.92731093582036,1.,0.171471191532988));
#33720=CARTESIAN_POINT('Ctrl Pts',(-1.9212233439798,-1.,0.172321621259514));
#33721=CARTESIAN_POINT('Ctrl Pts',(-1.9212233439798,1.,0.172321621259514));
#33722=CARTESIAN_POINT('Ctrl Pts',(-1.91511429159527,-1.,0.173090695383496));
#33723=CARTESIAN_POINT('Ctrl Pts',(-1.91511429159527,1.,0.173090695383496));
#33724=CARTESIAN_POINT('Ctrl Pts',(-1.90911693975267,-1.,0.173776635257817));
#33725=CARTESIAN_POINT('Ctrl Pts',(-1.90911693975267,1.,0.173776635257817));
#33726=CARTESIAN_POINT('Ctrl Pts',(-1.90335253862834,-1.,0.174375518661085));
#33727=CARTESIAN_POINT('Ctrl Pts',(-1.90335253862834,1.,0.174375518661085));
#33728=CARTESIAN_POINT('Ctrl Pts',(-1.89788101117132,-1.,0.174879405091263));
#33729=CARTESIAN_POINT('Ctrl Pts',(-1.89788101117132,1.,0.174879405091263));
#33730=CARTESIAN_POINT('Ctrl Pts',(-1.892646301985,-1.,0.175274276190844));
#33731=CARTESIAN_POINT('Ctrl Pts',(-1.892646301985,1.,0.175274276190844));
#33732=CARTESIAN_POINT('Ctrl Pts',(-1.88742606273259,-1.,0.175538155840648));
#33733=CARTESIAN_POINT('Ctrl Pts',(-1.88742606273259,1.,0.175538155840648));
#33734=CARTESIAN_POINT('Ctrl Pts',(-1.88188663145367,-1.,0.175644148889698));
#33735=CARTESIAN_POINT('Ctrl Pts',(-1.88188663145367,1.,0.175644148889698));
#33736=CARTESIAN_POINT('Ctrl Pts',(-1.87563767773588,-1.,0.175563480746485));
#33737=CARTESIAN_POINT('Ctrl Pts',(-1.87563767773588,1.,0.175563480746485));
#33738=CARTESIAN_POINT('Ctrl Pts',(-1.86828349694799,-1.,0.175268337590758));
#33739=CARTESIAN_POINT('Ctrl Pts',(-1.86828349694799,1.,0.175268337590758));
#33740=CARTESIAN_POINT('Ctrl Pts',(-1.85948367088837,-1.,0.17473525927603));
#33741=CARTESIAN_POINT('Ctrl Pts',(-1.85948367088837,1.,0.17473525927603));
#33742=CARTESIAN_POINT('Ctrl Pts',(-1.8489811319852,-1.,0.173946627587731));
#33743=CARTESIAN_POINT('Ctrl Pts',(-1.8489811319852,1.,0.173946627587731));
#33744=CARTESIAN_POINT('Ctrl Pts',(-1.83658380527692,-1.,0.1728894428919));
#33745=CARTESIAN_POINT('Ctrl Pts',(-1.83658380527692,1.,0.1728894428919));
#33746=CARTESIAN_POINT('Ctrl Pts',(-1.82215766811545,-1.,0.171554770204119));
#33747=CARTESIAN_POINT('Ctrl Pts',(-1.82215766811545,1.,0.171554770204119));
#33748=CARTESIAN_POINT('Ctrl Pts',(-1.80561530629706,-1.,0.169936923904608));
#33749=CARTESIAN_POINT('Ctrl Pts',(-1.80561530629706,1.,0.169936923904608));
#33750=CARTESIAN_POINT('Ctrl Pts',(-1.7869064998507,-1.,0.168032772805197));
#33751=CARTESIAN_POINT('Ctrl Pts',(-1.7869064998507,1.,0.168032772805197));
#33752=CARTESIAN_POINT('Ctrl Pts',(-1.77018771684844,-1.,0.1662793551464));
#33753=CARTESIAN_POINT('Ctrl Pts',(-1.77018771684844,1.,0.1662793551464));
#33754=CARTESIAN_POINT('Ctrl Pts',(-1.75666056638427,-1.,0.164834765707158));
#33755=CARTESIAN_POINT('Ctrl Pts',(-1.75666056638427,1.,0.164834765707158));
#33756=CARTESIAN_POINT('Ctrl Pts',(-1.7472034950333,-1.,0.163814161002002));
#33757=CARTESIAN_POINT('Ctrl Pts',(-1.7472034950333,1.,0.163814161002002));
#33758=CARTESIAN_POINT('Ctrl Pts',(-1.74236521665491,-1.,0.163289472382896));
#33759=CARTESIAN_POINT('Ctrl Pts',(-1.74236521665491,1.,0.163289472382896));
#33760=CARTESIAN_POINT('',(-2.19890268624765,1.,0.069476445021958));
#33761=CARTESIAN_POINT('Ctrl Pts',(-2.19890268624765,1.,0.069476445021958));
#33762=CARTESIAN_POINT('Ctrl Pts',(-2.19777582085423,1.,0.0701143536325489));
#33763=CARTESIAN_POINT('Ctrl Pts',(-2.19552129484002,1.,0.0713863779526153));
#33764=CARTESIAN_POINT('Ctrl Pts',(-2.19213712013662,1.,0.0732830357306724));
#33765=CARTESIAN_POINT('Ctrl Pts',(-2.1876201139953,1.,0.0757891465836146));
#33766=CARTESIAN_POINT('Ctrl Pts',(-2.18196589448887,1.,0.0788837727685241));
#33767=CARTESIAN_POINT('Ctrl Pts',(-2.176303712113,1.,0.0819402680872764));
#33768=CARTESIAN_POINT('Ctrl Pts',(-2.17063357870952,1.,0.0849584620835371));
#33769=CARTESIAN_POINT('Ctrl Pts',(-2.16495552645014,1.,0.0879381291386921));
#33770=CARTESIAN_POINT('Ctrl Pts',(-2.15926961544516,1.,0.0908789888107264));
#33771=CARTESIAN_POINT('Ctrl Pts',(-2.1535759397817,1.,0.0937807218867642));
#33772=CARTESIAN_POINT('Ctrl Pts',(-2.14787463531795,1.,0.0966429852305457));
#33773=CARTESIAN_POINT('Ctrl Pts',(-2.14216588396025,1.,0.0994654261990914));
#33774=CARTESIAN_POINT('Ctrl Pts',(-2.13644992667165,1.,0.1022477005561));
#33775=CARTESIAN_POINT('Ctrl Pts',(-2.13072704887293,1.,0.104989479152739));
#33776=CARTESIAN_POINT('Ctrl Pts',(-2.12499752307,1.,0.10769043523109));
#33777=CARTESIAN_POINT('Ctrl Pts',(-2.11926155590865,1.,0.110350236135025));
#33778=CARTESIAN_POINT('Ctrl Pts',(-2.11351924490306,1.,0.112968534419737));
#33779=CARTESIAN_POINT('Ctrl Pts',(-2.10777050261309,1.,0.115544957687926));
#33780=CARTESIAN_POINT('Ctrl Pts',(-2.102015121329,1.,0.118079107988355));
#33781=CARTESIAN_POINT('Ctrl Pts',(-2.0962529286773,1.,0.120570567965122));
#33782=CARTESIAN_POINT('Ctrl Pts',(-2.09048392424825,1.,0.123018905621083));
#33783=CARTESIAN_POINT('Ctrl Pts',(-2.08470840653643,1.,0.125423679412061));
#33784=CARTESIAN_POINT('Ctrl Pts',(-2.07892715110987,1.,0.12778444527612));
#33785=CARTESIAN_POINT('Ctrl Pts',(-2.07314114713063,1.,0.130100748328403));
#33786=CARTESIAN_POINT('Ctrl Pts',(-2.06735123910326,1.,0.13237211154771));
#33787=CARTESIAN_POINT('Ctrl Pts',(-2.06155781517842,1.,0.134598026192106));
#33788=CARTESIAN_POINT('Ctrl Pts',(-2.05576044414264,1.,0.136777941218043));
#33789=CARTESIAN_POINT('Ctrl Pts',(-2.04995762001328,1.,0.138911255368966));
#33790=CARTESIAN_POINT('Ctrl Pts',(-2.04414757947916,1.,0.140997332152546));
#33791=CARTESIAN_POINT('Ctrl Pts',(-2.03832911025912,1.,0.143035515058209));
#33792=CARTESIAN_POINT('Ctrl Pts',(-2.03250223739942,1.,0.145025140186057));
#33793=CARTESIAN_POINT('Ctrl Pts',(-2.02666926182017,1.,0.146965557332583));
#33794=CARTESIAN_POINT('Ctrl Pts',(-2.02083464969894,1.,0.148856124775337));
#33795=CARTESIAN_POINT('Ctrl Pts',(-2.01500291940238,1.,0.150696157673078));
#33796=CARTESIAN_POINT('Ctrl Pts',(-2.00917680318424,1.,0.15248488362145));
#33797=CARTESIAN_POINT('Ctrl Pts',(-2.00335565310543,1.,0.154221403049722));
#33798=CARTESIAN_POINT('Ctrl Pts',(-1.99753284771497,1.,0.155904629548783));
#33799=CARTESIAN_POINT('Ctrl Pts',(-1.99169810931908,1.,0.157533331459227));
#33800=CARTESIAN_POINT('Ctrl Pts',(-1.98584238283292,1.,0.159106226437299));
#33801=CARTESIAN_POINT('Ctrl Pts',(-1.97996195437559,1.,0.160622060784611));
#33802=CARTESIAN_POINT('Ctrl Pts',(-1.97406280235188,1.,0.162079693556288));
#33803=CARTESIAN_POINT('Ctrl Pts',(-1.96816512677967,1.,0.163478185457734));
#33804=CARTESIAN_POINT('Ctrl Pts',(-1.96229379940136,1.,0.164816568920269));
#33805=CARTESIAN_POINT('Ctrl Pts',(-1.9564675971873,1.,0.166093592002812));
#33806=CARTESIAN_POINT('Ctrl Pts',(-1.95069027794294,1.,0.167307501784475));
#33807=CARTESIAN_POINT('Ctrl Pts',(-1.94493757756931,1.,0.168455741607556));
#33808=CARTESIAN_POINT('Ctrl Pts',(-1.93915639211581,1.,0.169534904817491));
#33809=CARTESIAN_POINT('Ctrl Pts',(-1.93329183155539,1.,0.170541253116201));
#33810=CARTESIAN_POINT('Ctrl Pts',(-1.92731093582036,1.,0.171471191532988));
#33811=CARTESIAN_POINT('Ctrl Pts',(-1.9212233439798,1.,0.172321621259514));
#33812=CARTESIAN_POINT('Ctrl Pts',(-1.91511429159527,1.,0.173090695383496));
#33813=CARTESIAN_POINT('Ctrl Pts',(-1.90911693975267,1.,0.173776635257817));
#33814=CARTESIAN_POINT('Ctrl Pts',(-1.90335253862834,1.,0.174375518661085));
#33815=CARTESIAN_POINT('Ctrl Pts',(-1.89788101117132,1.,0.174879405091263));
#33816=CARTESIAN_POINT('Ctrl Pts',(-1.892646301985,1.,0.175274276190844));
#33817=CARTESIAN_POINT('Ctrl Pts',(-1.88742606273259,1.,0.175538155840648));
#33818=CARTESIAN_POINT('Ctrl Pts',(-1.88188663145367,1.,0.175644148889698));
#33819=CARTESIAN_POINT('Ctrl Pts',(-1.87563767773588,1.,0.175563480746485));
#33820=CARTESIAN_POINT('Ctrl Pts',(-1.86828349694799,1.,0.175268337590758));
#33821=CARTESIAN_POINT('Ctrl Pts',(-1.85948367088837,1.,0.17473525927603));
#33822=CARTESIAN_POINT('Ctrl Pts',(-1.8489811319852,1.,0.173946627587731));
#33823=CARTESIAN_POINT('Ctrl Pts',(-1.83658380527692,1.,0.1728894428919));
#33824=CARTESIAN_POINT('Ctrl Pts',(-1.82215766811545,1.,0.171554770204119));
#33825=CARTESIAN_POINT('Ctrl Pts',(-1.80561530629706,1.,0.169936923904608));
#33826=CARTESIAN_POINT('Ctrl Pts',(-1.7869064998507,1.,0.168032772805197));
#33827=CARTESIAN_POINT('Ctrl Pts',(-1.77018771684844,1.,0.1662793551464));
#33828=CARTESIAN_POINT('Ctrl Pts',(-1.75666056638427,1.,0.164834765707158));
#33829=CARTESIAN_POINT('Ctrl Pts',(-1.7472034950333,1.,0.163814161002002));
#33830=CARTESIAN_POINT('Ctrl Pts',(-1.74236521665491,1.,0.163289472382896));
#33831=CARTESIAN_POINT('',(-2.19890268624765,0.,0.069476445021958));
#33832=CARTESIAN_POINT('Origin',(-2.19890268624765,0.,-0.0694764450219585));
#33833=CARTESIAN_POINT('',(-2.19890268624765,1.,-0.0694764450219585));
#33834=CARTESIAN_POINT('',(-2.19890268624765,1.,0.069476445021958));
#33835=CARTESIAN_POINT('',(-2.19890268624765,0.,-0.0694764450219585));
#33836=CARTESIAN_POINT('Ctrl Pts',(-1.74236521665491,-1.,-0.163289472382896));
#33837=CARTESIAN_POINT('Ctrl Pts',(-1.74236521665491,1.,-0.163289472382896));
#33838=CARTESIAN_POINT('Ctrl Pts',(-1.74720349503904,-1.,-0.163814161002474));
#33839=CARTESIAN_POINT('Ctrl Pts',(-1.74720349503904,1.,-0.163814161002474));
#33840=CARTESIAN_POINT('Ctrl Pts',(-1.75666056640041,-1.,-0.164834765708484));
#33841=CARTESIAN_POINT('Ctrl Pts',(-1.75666056640041,1.,-0.164834765708484));
#33842=CARTESIAN_POINT('Ctrl Pts',(-1.77018771687692,-1.,-0.166279355148738));
#33843=CARTESIAN_POINT('Ctrl Pts',(-1.77018771687692,1.,-0.166279355148738));
#33844=CARTESIAN_POINT('Ctrl Pts',(-1.78690649988931,-1.,-0.16803277280837));
#33845=CARTESIAN_POINT('Ctrl Pts',(-1.78690649988931,1.,-0.16803277280837));
#33846=CARTESIAN_POINT('Ctrl Pts',(-1.80561530633924,-1.,-0.169936923908078));
#33847=CARTESIAN_POINT('Ctrl Pts',(-1.80561530633924,1.,-0.169936923908078));
#33848=CARTESIAN_POINT('Ctrl Pts',(-1.82215766815414,-1.,-0.171554770207306));
#33849=CARTESIAN_POINT('Ctrl Pts',(-1.82215766815414,1.,-0.171554770207306));
#33850=CARTESIAN_POINT('Ctrl Pts',(-1.83658380530747,-1.,-0.17288944289442));
#33851=CARTESIAN_POINT('Ctrl Pts',(-1.83658380530747,1.,-0.17288944289442));
#33852=CARTESIAN_POINT('Ctrl Pts',(-1.84898113200543,-1.,-0.173946627589401));
#33853=CARTESIAN_POINT('Ctrl Pts',(-1.84898113200543,1.,-0.173946627589401));
#33854=CARTESIAN_POINT('Ctrl Pts',(-1.85948367089838,-1.,-0.174735259276856));
#33855=CARTESIAN_POINT('Ctrl Pts',(-1.85948367089838,1.,-0.174735259276856));
#33856=CARTESIAN_POINT('Ctrl Pts',(-1.86828349694972,-1.,-0.175268337590901));
#33857=CARTESIAN_POINT('Ctrl Pts',(-1.86828349694972,1.,-0.175268337590901));
#33858=CARTESIAN_POINT('Ctrl Pts',(-1.87563767773249,-1.,-0.175563480746205));
#33859=CARTESIAN_POINT('Ctrl Pts',(-1.87563767773249,1.,-0.175563480746205));
#33860=CARTESIAN_POINT('Ctrl Pts',(-1.88188663144846,-1.,-0.175644148889271));
#33861=CARTESIAN_POINT('Ctrl Pts',(-1.88188663144846,1.,-0.175644148889271));
#33862=CARTESIAN_POINT('Ctrl Pts',(-1.88742606272818,-1.,-0.175538155840286));
#33863=CARTESIAN_POINT('Ctrl Pts',(-1.88742606272818,1.,-0.175538155840286));
#33864=CARTESIAN_POINT('Ctrl Pts',(-1.89264630198279,-1.,-0.175274276190664));
#33865=CARTESIAN_POINT('Ctrl Pts',(-1.89264630198279,1.,-0.175274276190664));
#33866=CARTESIAN_POINT('Ctrl Pts',(-1.89788101117148,-1.,-0.174879405091277));
#33867=CARTESIAN_POINT('Ctrl Pts',(-1.89788101117148,1.,-0.174879405091277));
#33868=CARTESIAN_POINT('Ctrl Pts',(-1.90335253863003,-1.,-0.174375518661222));
#33869=CARTESIAN_POINT('Ctrl Pts',(-1.90335253863003,1.,-0.174375518661222));
#33870=CARTESIAN_POINT('Ctrl Pts',(-1.90911693975475,-1.,-0.173776635257984));
#33871=CARTESIAN_POINT('Ctrl Pts',(-1.90911693975475,1.,-0.173776635257984));
#33872=CARTESIAN_POINT('Ctrl Pts',(-1.91511429159681,-1.,-0.173090695383619));
#33873=CARTESIAN_POINT('Ctrl Pts',(-1.91511429159681,1.,-0.173090695383619));
#33874=CARTESIAN_POINT('Ctrl Pts',(-1.92122334398034,-1.,-0.172321621259557));
#33875=CARTESIAN_POINT('Ctrl Pts',(-1.92122334398034,1.,-0.172321621259557));
#33876=CARTESIAN_POINT('Ctrl Pts',(-1.92731093582,-1.,-0.17147119153296));
#33877=CARTESIAN_POINT('Ctrl Pts',(-1.92731093582,1.,-0.17147119153296));
#33878=CARTESIAN_POINT('Ctrl Pts',(-1.93329183155455,-1.,-0.170541253116136));
#33879=CARTESIAN_POINT('Ctrl Pts',(-1.93329183155455,1.,-0.170541253116136));
#33880=CARTESIAN_POINT('Ctrl Pts',(-1.93915639211497,-1.,-0.169534904817425));
#33881=CARTESIAN_POINT('Ctrl Pts',(-1.93915639211497,1.,-0.169534904817425));
#33882=CARTESIAN_POINT('Ctrl Pts',(-1.94493757756879,-1.,-0.168455741607516));
#33883=CARTESIAN_POINT('Ctrl Pts',(-1.94493757756879,1.,-0.168455741607516));
#33884=CARTESIAN_POINT('Ctrl Pts',(-1.95069027794286,-1.,-0.167307501784469));
#33885=CARTESIAN_POINT('Ctrl Pts',(-1.95069027794286,1.,-0.167307501784469));
#33886=CARTESIAN_POINT('Ctrl Pts',(-1.95646759718755,-1.,-0.166093592002833));
#33887=CARTESIAN_POINT('Ctrl Pts',(-1.95646759718755,1.,-0.166093592002833));
#33888=CARTESIAN_POINT('Ctrl Pts',(-1.96229379940174,-1.,-0.1648165689203));
#33889=CARTESIAN_POINT('Ctrl Pts',(-1.96229379940174,1.,-0.1648165689203));
#33890=CARTESIAN_POINT('Ctrl Pts',(-1.96816512678,-1.,-0.16347818545776));
#33891=CARTESIAN_POINT('Ctrl Pts',(-1.96816512678,1.,-0.16347818545776));
#33892=CARTESIAN_POINT('Ctrl Pts',(-1.97406280235204,-1.,-0.162079693556302));
#33893=CARTESIAN_POINT('Ctrl Pts',(-1.97406280235204,1.,-0.162079693556302));
#33894=CARTESIAN_POINT('Ctrl Pts',(-1.97996195437557,-1.,-0.16062206078461));
#33895=CARTESIAN_POINT('Ctrl Pts',(-1.97996195437557,1.,-0.16062206078461));
#33896=CARTESIAN_POINT('Ctrl Pts',(-1.98584238283279,-1.,-0.159106226437289));
#33897=CARTESIAN_POINT('Ctrl Pts',(-1.98584238283279,1.,-0.159106226437289));
#33898=CARTESIAN_POINT('Ctrl Pts',(-1.99169810931893,-1.,-0.157533331459215));
#33899=CARTESIAN_POINT('Ctrl Pts',(-1.99169810931893,1.,-0.157533331459215));
#33900=CARTESIAN_POINT('Ctrl Pts',(-1.99753284771487,-1.,-0.155904629548775));
#33901=CARTESIAN_POINT('Ctrl Pts',(-1.99753284771487,1.,-0.155904629548775));
#33902=CARTESIAN_POINT('Ctrl Pts',(-2.00335565310539,-1.,-0.154221403049719));
#33903=CARTESIAN_POINT('Ctrl Pts',(-2.00335565310539,1.,-0.154221403049719));
#33904=CARTESIAN_POINT('Ctrl Pts',(-2.00917680318426,-1.,-0.152484883621452));
#33905=CARTESIAN_POINT('Ctrl Pts',(-2.00917680318426,1.,-0.152484883621452));
#33906=CARTESIAN_POINT('Ctrl Pts',(-2.01500291940243,-1.,-0.150696157673084));
#33907=CARTESIAN_POINT('Ctrl Pts',(-2.01500291940243,1.,-0.150696157673084));
#33908=CARTESIAN_POINT('Ctrl Pts',(-2.02083464969897,-1.,-0.148856124775343));
#33909=CARTESIAN_POINT('Ctrl Pts',(-2.02083464969897,1.,-0.148856124775343));
#33910=CARTESIAN_POINT('Ctrl Pts',(-2.02666926182017,-1.,-0.146965557332586));
#33911=CARTESIAN_POINT('Ctrl Pts',(-2.02666926182017,1.,-0.146965557332586));
#33912=CARTESIAN_POINT('Ctrl Pts',(-2.03250223739941,-1.,-0.145025140186058));
#33913=CARTESIAN_POINT('Ctrl Pts',(-2.03250223739941,1.,-0.145025140186058));
#33914=CARTESIAN_POINT('Ctrl Pts',(-2.03832911025913,-1.,-0.143035515058208));
#33915=CARTESIAN_POINT('Ctrl Pts',(-2.03832911025913,1.,-0.143035515058208));
#33916=CARTESIAN_POINT('Ctrl Pts',(-2.04414757947919,-1.,-0.140997332152545));
#33917=CARTESIAN_POINT('Ctrl Pts',(-2.04414757947919,1.,-0.140997332152545));
#33918=CARTESIAN_POINT('Ctrl Pts',(-2.04995762001333,-1.,-0.138911255368966));
#33919=CARTESIAN_POINT('Ctrl Pts',(-2.04995762001333,1.,-0.138911255368966));
#33920=CARTESIAN_POINT('Ctrl Pts',(-2.0557604441427,-1.,-0.136777941218044));
#33921=CARTESIAN_POINT('Ctrl Pts',(-2.0557604441427,1.,-0.136777941218044));
#33922=CARTESIAN_POINT('Ctrl Pts',(-2.06155781517844,-1.,-0.134598026192107));
#33923=CARTESIAN_POINT('Ctrl Pts',(-2.06155781517844,1.,-0.134598026192107));
#33924=CARTESIAN_POINT('Ctrl Pts',(-2.06735123910319,-1.,-0.13237211154771));
#33925=CARTESIAN_POINT('Ctrl Pts',(-2.06735123910319,1.,-0.13237211154771));
#33926=CARTESIAN_POINT('Ctrl Pts',(-2.07314114713047,-1.,-0.130100748328401));
#33927=CARTESIAN_POINT('Ctrl Pts',(-2.07314114713047,1.,-0.130100748328401));
#33928=CARTESIAN_POINT('Ctrl Pts',(-2.07892715110967,-1.,-0.127784445276116));
#33929=CARTESIAN_POINT('Ctrl Pts',(-2.07892715110967,1.,-0.127784445276116));
#33930=CARTESIAN_POINT('Ctrl Pts',(-2.08470840653628,-1.,-0.125423679412058));
#33931=CARTESIAN_POINT('Ctrl Pts',(-2.08470840653628,1.,-0.125423679412058));
#33932=CARTESIAN_POINT('Ctrl Pts',(-2.09048392424826,-1.,-0.123018905621083));
#33933=CARTESIAN_POINT('Ctrl Pts',(-2.09048392424826,1.,-0.123018905621083));
#33934=CARTESIAN_POINT('Ctrl Pts',(-2.09625292867756,-1.,-0.120570567965129));
#33935=CARTESIAN_POINT('Ctrl Pts',(-2.09625292867756,1.,-0.120570567965129));
#33936=CARTESIAN_POINT('Ctrl Pts',(-2.10201512132945,-1.,-0.118079107988368));
#33937=CARTESIAN_POINT('Ctrl Pts',(-2.10201512132945,1.,-0.118079107988368));
#33938=CARTESIAN_POINT('Ctrl Pts',(-2.10777050261359,-1.,-0.11554495768794));
#33939=CARTESIAN_POINT('Ctrl Pts',(-2.10777050261359,1.,-0.11554495768794));
#33940=CARTESIAN_POINT('Ctrl Pts',(-2.11351924490335,-1.,-0.112968534419746));
#33941=CARTESIAN_POINT('Ctrl Pts',(-2.11351924490335,1.,-0.112968534419746));
#33942=CARTESIAN_POINT('Ctrl Pts',(-2.11926155590849,-1.,-0.11035023613502));
#33943=CARTESIAN_POINT('Ctrl Pts',(-2.11926155590849,1.,-0.11035023613502));
#33944=CARTESIAN_POINT('Ctrl Pts',(-2.12499752306927,-1.,-0.107690435231068));
#33945=CARTESIAN_POINT('Ctrl Pts',(-2.12499752306927,1.,-0.107690435231068));
#33946=CARTESIAN_POINT('Ctrl Pts',(-2.1307270488718,-1.,-0.104989479152703));
#33947=CARTESIAN_POINT('Ctrl Pts',(-2.1307270488718,1.,-0.104989479152703));
#33948=CARTESIAN_POINT('Ctrl Pts',(-2.13644992667052,-1.,-0.102247700556064));
#33949=CARTESIAN_POINT('Ctrl Pts',(-2.13644992667052,1.,-0.102247700556064));
#33950=CARTESIAN_POINT('Ctrl Pts',(-2.14216588395974,-1.,-0.0994654261990744));
#33951=CARTESIAN_POINT('Ctrl Pts',(-2.14216588395974,1.,-0.0994654261990744));
#33952=CARTESIAN_POINT('Ctrl Pts',(-2.14787463531864,-1.,-0.096642985230569));
#33953=CARTESIAN_POINT('Ctrl Pts',(-2.14787463531864,1.,-0.096642985230569));
#33954=CARTESIAN_POINT('Ctrl Pts',(-2.15357593978377,-1.,-0.0937807218868346));
#33955=CARTESIAN_POINT('Ctrl Pts',(-2.15357593978377,1.,-0.0937807218868346));
#33956=CARTESIAN_POINT('Ctrl Pts',(-2.15926961544808,-1.,-0.0908789888108267));
#33957=CARTESIAN_POINT('Ctrl Pts',(-2.15926961544808,1.,-0.0908789888108267));
#33958=CARTESIAN_POINT('Ctrl Pts',(-2.16495552645275,-1.,-0.0879381291387824));
#33959=CARTESIAN_POINT('Ctrl Pts',(-2.16495552645275,1.,-0.0879381291387824));
#33960=CARTESIAN_POINT('Ctrl Pts',(-2.17063357871031,-1.,-0.0849584620835644));
#33961=CARTESIAN_POINT('Ctrl Pts',(-2.17063357871031,1.,-0.0849584620835644));
#33962=CARTESIAN_POINT('Ctrl Pts',(-2.1763037121106,-1.,-0.0819402680871941));
#33963=CARTESIAN_POINT('Ctrl Pts',(-2.1763037121106,1.,-0.0819402680871941));
#33964=CARTESIAN_POINT('Ctrl Pts',(-2.18196589448304,-1.,-0.0788837727683229));
#33965=CARTESIAN_POINT('Ctrl Pts',(-2.18196589448304,1.,-0.0788837727683229));
#33966=CARTESIAN_POINT('Ctrl Pts',(-2.1876201139874,-1.,-0.0757891465833413));
#33967=CARTESIAN_POINT('Ctrl Pts',(-2.1876201139874,1.,-0.0757891465833413));
#33968=CARTESIAN_POINT('Ctrl Pts',(-2.19213712012956,-1.,-0.0732830357304277));
#33969=CARTESIAN_POINT('Ctrl Pts',(-2.19213712012956,1.,-0.0732830357304277));
#33970=CARTESIAN_POINT('Ctrl Pts',(-2.19552129483562,-1.,-0.0713863779524629));
#33971=CARTESIAN_POINT('Ctrl Pts',(-2.19552129483562,1.,-0.0713863779524629));
#33972=CARTESIAN_POINT('Ctrl Pts',(-2.19777582085261,-1.,-0.0701143536324927));
#33973=CARTESIAN_POINT('Ctrl Pts',(-2.19777582085261,1.,-0.0701143536324927));
#33974=CARTESIAN_POINT('Ctrl Pts',(-2.19890268624765,-1.,-0.0694764450219585));
#33975=CARTESIAN_POINT('Ctrl Pts',(-2.19890268624765,1.,-0.0694764450219585));
#33976=CARTESIAN_POINT('',(-1.74236521665491,1.,-0.163289472382896));
#33977=CARTESIAN_POINT('Ctrl Pts',(-1.74236521665491,1.,-0.163289472382896));
#33978=CARTESIAN_POINT('Ctrl Pts',(-1.74720349503904,1.,-0.163814161002474));
#33979=CARTESIAN_POINT('Ctrl Pts',(-1.75666056640041,1.,-0.164834765708484));
#33980=CARTESIAN_POINT('Ctrl Pts',(-1.77018771687692,1.,-0.166279355148738));
#33981=CARTESIAN_POINT('Ctrl Pts',(-1.78690649988931,1.,-0.16803277280837));
#33982=CARTESIAN_POINT('Ctrl Pts',(-1.80561530633924,1.,-0.169936923908078));
#33983=CARTESIAN_POINT('Ctrl Pts',(-1.82215766815414,1.,-0.171554770207306));
#33984=CARTESIAN_POINT('Ctrl Pts',(-1.83658380530747,1.,-0.17288944289442));
#33985=CARTESIAN_POINT('Ctrl Pts',(-1.84898113200543,1.,-0.173946627589401));
#33986=CARTESIAN_POINT('Ctrl Pts',(-1.85948367089838,1.,-0.174735259276856));
#33987=CARTESIAN_POINT('Ctrl Pts',(-1.86828349694972,1.,-0.175268337590901));
#33988=CARTESIAN_POINT('Ctrl Pts',(-1.87563767773249,1.,-0.175563480746205));
#33989=CARTESIAN_POINT('Ctrl Pts',(-1.88188663144846,1.,-0.175644148889271));
#33990=CARTESIAN_POINT('Ctrl Pts',(-1.88742606272818,1.,-0.175538155840286));
#33991=CARTESIAN_POINT('Ctrl Pts',(-1.89264630198279,1.,-0.175274276190664));
#33992=CARTESIAN_POINT('Ctrl Pts',(-1.89788101117148,1.,-0.174879405091277));
#33993=CARTESIAN_POINT('Ctrl Pts',(-1.90335253863003,1.,-0.174375518661222));
#33994=CARTESIAN_POINT('Ctrl Pts',(-1.90911693975475,1.,-0.173776635257984));
#33995=CARTESIAN_POINT('Ctrl Pts',(-1.91511429159681,1.,-0.173090695383619));
#33996=CARTESIAN_POINT('Ctrl Pts',(-1.92122334398034,1.,-0.172321621259557));
#33997=CARTESIAN_POINT('Ctrl Pts',(-1.92731093582,1.,-0.17147119153296));
#33998=CARTESIAN_POINT('Ctrl Pts',(-1.93329183155455,1.,-0.170541253116136));
#33999=CARTESIAN_POINT('Ctrl Pts',(-1.93915639211497,1.,-0.169534904817425));
#34000=CARTESIAN_POINT('Ctrl Pts',(-1.94493757756879,1.,-0.168455741607516));
#34001=CARTESIAN_POINT('Ctrl Pts',(-1.95069027794286,1.,-0.167307501784469));
#34002=CARTESIAN_POINT('Ctrl Pts',(-1.95646759718755,1.,-0.166093592002833));
#34003=CARTESIAN_POINT('Ctrl Pts',(-1.96229379940174,1.,-0.1648165689203));
#34004=CARTESIAN_POINT('Ctrl Pts',(-1.96816512678,1.,-0.16347818545776));
#34005=CARTESIAN_POINT('Ctrl Pts',(-1.97406280235204,1.,-0.162079693556302));
#34006=CARTESIAN_POINT('Ctrl Pts',(-1.97996195437557,1.,-0.16062206078461));
#34007=CARTESIAN_POINT('Ctrl Pts',(-1.98584238283279,1.,-0.159106226437289));
#34008=CARTESIAN_POINT('Ctrl Pts',(-1.99169810931893,1.,-0.157533331459215));
#34009=CARTESIAN_POINT('Ctrl Pts',(-1.99753284771487,1.,-0.155904629548775));
#34010=CARTESIAN_POINT('Ctrl Pts',(-2.00335565310539,1.,-0.154221403049719));
#34011=CARTESIAN_POINT('Ctrl Pts',(-2.00917680318426,1.,-0.152484883621452));
#34012=CARTESIAN_POINT('Ctrl Pts',(-2.01500291940243,1.,-0.150696157673084));
#34013=CARTESIAN_POINT('Ctrl Pts',(-2.02083464969897,1.,-0.148856124775343));
#34014=CARTESIAN_POINT('Ctrl Pts',(-2.02666926182017,1.,-0.146965557332586));
#34015=CARTESIAN_POINT('Ctrl Pts',(-2.03250223739941,1.,-0.145025140186058));
#34016=CARTESIAN_POINT('Ctrl Pts',(-2.03832911025913,1.,-0.143035515058208));
#34017=CARTESIAN_POINT('Ctrl Pts',(-2.04414757947919,1.,-0.140997332152545));
#34018=CARTESIAN_POINT('Ctrl Pts',(-2.04995762001333,1.,-0.138911255368966));
#34019=CARTESIAN_POINT('Ctrl Pts',(-2.0557604441427,1.,-0.136777941218044));
#34020=CARTESIAN_POINT('Ctrl Pts',(-2.06155781517844,1.,-0.134598026192107));
#34021=CARTESIAN_POINT('Ctrl Pts',(-2.06735123910319,1.,-0.13237211154771));
#34022=CARTESIAN_POINT('Ctrl Pts',(-2.07314114713047,1.,-0.130100748328401));
#34023=CARTESIAN_POINT('Ctrl Pts',(-2.07892715110967,1.,-0.127784445276116));
#34024=CARTESIAN_POINT('Ctrl Pts',(-2.08470840653628,1.,-0.125423679412058));
#34025=CARTESIAN_POINT('Ctrl Pts',(-2.09048392424826,1.,-0.123018905621083));
#34026=CARTESIAN_POINT('Ctrl Pts',(-2.09625292867756,1.,-0.120570567965129));
#34027=CARTESIAN_POINT('Ctrl Pts',(-2.10201512132945,1.,-0.118079107988368));
#34028=CARTESIAN_POINT('Ctrl Pts',(-2.10777050261359,1.,-0.11554495768794));
#34029=CARTESIAN_POINT('Ctrl Pts',(-2.11351924490335,1.,-0.112968534419746));
#34030=CARTESIAN_POINT('Ctrl Pts',(-2.11926155590849,1.,-0.11035023613502));
#34031=CARTESIAN_POINT('Ctrl Pts',(-2.12499752306927,1.,-0.107690435231068));
#34032=CARTESIAN_POINT('Ctrl Pts',(-2.1307270488718,1.,-0.104989479152703));
#34033=CARTESIAN_POINT('Ctrl Pts',(-2.13644992667052,1.,-0.102247700556064));
#34034=CARTESIAN_POINT('Ctrl Pts',(-2.14216588395974,1.,-0.0994654261990744));
#34035=CARTESIAN_POINT('Ctrl Pts',(-2.14787463531864,1.,-0.096642985230569));
#34036=CARTESIAN_POINT('Ctrl Pts',(-2.15357593978377,1.,-0.0937807218868346));
#34037=CARTESIAN_POINT('Ctrl Pts',(-2.15926961544808,1.,-0.0908789888108267));
#34038=CARTESIAN_POINT('Ctrl Pts',(-2.16495552645275,1.,-0.0879381291387824));
#34039=CARTESIAN_POINT('Ctrl Pts',(-2.17063357871031,1.,-0.0849584620835644));
#34040=CARTESIAN_POINT('Ctrl Pts',(-2.1763037121106,1.,-0.0819402680871941));
#34041=CARTESIAN_POINT('Ctrl Pts',(-2.18196589448304,1.,-0.0788837727683229));
#34042=CARTESIAN_POINT('Ctrl Pts',(-2.1876201139874,1.,-0.0757891465833413));
#34043=CARTESIAN_POINT('Ctrl Pts',(-2.19213712012956,1.,-0.0732830357304277));
#34044=CARTESIAN_POINT('Ctrl Pts',(-2.19552129483562,1.,-0.0713863779524629));
#34045=CARTESIAN_POINT('Ctrl Pts',(-2.19777582085261,1.,-0.0701143536324927));
#34046=CARTESIAN_POINT('Ctrl Pts',(-2.19890268624765,1.,-0.0694764450219585));
#34047=CARTESIAN_POINT('',(-1.74236521665491,0.,-0.163289472382896));
#34048=CARTESIAN_POINT('Origin',(0.,0.,0.));
#34049=CARTESIAN_POINT('',(-1.7075470150345,1.,-0.383122945602004));
#34050=CARTESIAN_POINT('Origin',(0.,1.,0.));
#34051=CARTESIAN_POINT('',(-1.7075470150345,0.,-0.383122945602004));
#34052=CARTESIAN_POINT('Ctrl Pts',(-2.11275013067528,-1.,-0.61342227326009));
#34053=CARTESIAN_POINT('Ctrl Pts',(-2.11275013067528,1.,-0.61342227326009));
#34054=CARTESIAN_POINT('Ctrl Pts',(-2.11187554260142,-1.,-0.61246736556225));
#34055=CARTESIAN_POINT('Ctrl Pts',(-2.11187554260142,1.,-0.61246736556225));
#34056=CARTESIAN_POINT('Ctrl Pts',(-2.11012443807661,-1.,-0.610560911691113));
#34057=CARTESIAN_POINT('Ctrl Pts',(-2.11012443807661,1.,-0.610560911691113));
#34058=CARTESIAN_POINT('Ctrl Pts',(-2.10749199615859,-1.,-0.607711315456826));
#34059=CARTESIAN_POINT('Ctrl Pts',(-2.10749199615859,1.,-0.607711315456826));
#34060=CARTESIAN_POINT('Ctrl Pts',(-2.10397049887709,-1.,-0.603932030738212));
#34061=CARTESIAN_POINT('Ctrl Pts',(-2.10397049887709,1.,-0.603932030738212));
#34062=CARTESIAN_POINT('Ctrl Pts',(-2.09954930865331,-1.,-0.599241616422144));
#34063=CARTESIAN_POINT('Ctrl Pts',(-2.09954930865331,1.,-0.599241616422144));
#34064=CARTESIAN_POINT('Ctrl Pts',(-2.09510876220501,-1.,-0.594585006052823));
#34065=CARTESIAN_POINT('Ctrl Pts',(-2.09510876220501,1.,-0.594585006052823));
#34066=CARTESIAN_POINT('Ctrl Pts',(-2.09064881812053,-1.,-0.589962365403189));
#34067=CARTESIAN_POINT('Ctrl Pts',(-2.09064881812053,1.,-0.589962365403189));
#34068=CARTESIAN_POINT('Ctrl Pts',(-2.086169437277,-1.,-0.585373918990895));
#34069=CARTESIAN_POINT('Ctrl Pts',(-2.086169437277,1.,-0.585373918990895));
#34070=CARTESIAN_POINT('Ctrl Pts',(-2.08167059018138,-1.,-0.580819952107257));
#34071=CARTESIAN_POINT('Ctrl Pts',(-2.08167059018138,1.,-0.580819952107257));
#34072=CARTESIAN_POINT('Ctrl Pts',(-2.07715226767361,-1.,-0.576300797416274));
#34073=CARTESIAN_POINT('Ctrl Pts',(-2.07715226767361,1.,-0.576300797416274));
#34074=CARTESIAN_POINT('Ctrl Pts',(-2.07261449292757,-1.,-0.571816823242411));
#34075=CARTESIAN_POINT('Ctrl Pts',(-2.07261449292757,1.,-0.571816823242411));
#34076=CARTESIAN_POINT('Ctrl Pts',(-2.06805732997383,-1.,-0.567368421181229));
#34077=CARTESIAN_POINT('Ctrl Pts',(-2.06805732997383,1.,-0.567368421181229));
#34078=CARTESIAN_POINT('Ctrl Pts',(-2.06348090160697,-1.,-0.562955993082574));
#34079=CARTESIAN_POINT('Ctrl Pts',(-2.06348090160697,1.,-0.562955993082574));
#34080=CARTESIAN_POINT('Ctrl Pts',(-2.05888537756571,-1.,-0.558579940185467));
#34081=CARTESIAN_POINT('Ctrl Pts',(-2.05888537756571,1.,-0.558579940185467));
#34082=CARTESIAN_POINT('Ctrl Pts',(-2.05427091604482,-1.,-0.554240657464109));
#34083=CARTESIAN_POINT('Ctrl Pts',(-2.05427091604482,1.,-0.554240657464109));
#34084=CARTESIAN_POINT('Ctrl Pts',(-2.04963761077974,-1.,-0.549938525150342));
#34085=CARTESIAN_POINT('Ctrl Pts',(-2.04963761077974,1.,-0.549938525150342));
#34086=CARTESIAN_POINT('Ctrl Pts',(-2.0449854471456,-1.,-0.545673903817348));
#34087=CARTESIAN_POINT('Ctrl Pts',(-2.0449854471456,1.,-0.545673903817348));
#34088=CARTESIAN_POINT('Ctrl Pts',(-2.0403142269048,-1.,-0.54144712061552));
#34089=CARTESIAN_POINT('Ctrl Pts',(-2.0403142269048,1.,-0.54144712061552));
#34090=CARTESIAN_POINT('Ctrl Pts',(-2.03562362953993,-1.,-0.537258489833134));
#34091=CARTESIAN_POINT('Ctrl Pts',(-2.03562362953993,1.,-0.537258489833134));
#34092=CARTESIAN_POINT('Ctrl Pts',(-2.03091336214401,-1.,-0.533108355132905));
#34093=CARTESIAN_POINT('Ctrl Pts',(-2.03091336214401,1.,-0.533108355132905));
#34094=CARTESIAN_POINT('Ctrl Pts',(-2.02618329083289,-1.,-0.52899712724191));
#34095=CARTESIAN_POINT('Ctrl Pts',(-2.02618329083289,1.,-0.52899712724191));
#34096=CARTESIAN_POINT('Ctrl Pts',(-2.02143356304712,-1.,-0.524925318333518));
#34097=CARTESIAN_POINT('Ctrl Pts',(-2.02143356304712,1.,-0.524925318333518));
#34098=CARTESIAN_POINT('Ctrl Pts',(-2.01666477917305,-1.,-0.520893590399428));
#34099=CARTESIAN_POINT('Ctrl Pts',(-2.01666477917305,1.,-0.520893590399428));
#34100=CARTESIAN_POINT('Ctrl Pts',(-2.01187773939257,-1.,-0.516902681728733));
#34101=CARTESIAN_POINT('Ctrl Pts',(-2.01187773939257,1.,-0.516902681728733));
#34102=CARTESIAN_POINT('Ctrl Pts',(-2.00707309946955,-1.,-0.512953306961813));
#34103=CARTESIAN_POINT('Ctrl Pts',(-2.00707309946955,1.,-0.512953306961813));
#34104=CARTESIAN_POINT('Ctrl Pts',(-2.00225107134733,-1.,-0.509046069886152));
#34105=CARTESIAN_POINT('Ctrl Pts',(-2.00225107134733,1.,-0.509046069886152));
#34106=CARTESIAN_POINT('Ctrl Pts',(-1.99741107463567,-1.,-0.505181361323011));
#34107=CARTESIAN_POINT('Ctrl Pts',(-1.99741107463567,1.,-0.505181361323011));
#34108=CARTESIAN_POINT('Ctrl Pts',(-1.9925514912615,-1.,-0.501359287727129));
#34109=CARTESIAN_POINT('Ctrl Pts',(-1.9925514912615,1.,-0.501359287727129));
#34110=CARTESIAN_POINT('Ctrl Pts',(-1.98767044752929,-1.,-0.497579909545564));
#34111=CARTESIAN_POINT('Ctrl Pts',(-1.98767044752929,1.,-0.497579909545564));
#34112=CARTESIAN_POINT('Ctrl Pts',(-1.9827665876182,-1.,-0.493843476541492));
#34113=CARTESIAN_POINT('Ctrl Pts',(-1.9827665876182,1.,-0.493843476541492));
#34114=CARTESIAN_POINT('Ctrl Pts',(-1.97783973019229,-1.,-0.490150627860955));
#34115=CARTESIAN_POINT('Ctrl Pts',(-1.97783973019229,1.,-0.490150627860955));
#34116=CARTESIAN_POINT('Ctrl Pts',(-1.97289186263272,-1.,-0.486502692907661));
#34117=CARTESIAN_POINT('Ctrl Pts',(-1.97289186263272,1.,-0.486502692907661));
#34118=CARTESIAN_POINT('Ctrl Pts',(-1.96792703422358,-1.,-0.482901662120686));
#34119=CARTESIAN_POINT('Ctrl Pts',(-1.96792703422358,1.,-0.482901662120686));
#34120=CARTESIAN_POINT('Ctrl Pts',(-1.96294933055938,-1.,-0.479349583074846));
#34121=CARTESIAN_POINT('Ctrl Pts',(-1.96294933055938,1.,-0.479349583074846));
#34122=CARTESIAN_POINT('Ctrl Pts',(-1.95796111148175,-1.,-0.475848034683171));
#34123=CARTESIAN_POINT('Ctrl Pts',(-1.95796111148175,1.,-0.475848034683171));
#34124=CARTESIAN_POINT('Ctrl Pts',(-1.95296148278136,-1.,-0.472397672264079));
#34125=CARTESIAN_POINT('Ctrl Pts',(-1.95296148278136,1.,-0.472397672264079));
#34126=CARTESIAN_POINT('Ctrl Pts',(-1.94794381136524,-1.,-0.468997482913158));
#34127=CARTESIAN_POINT('Ctrl Pts',(-1.94794381136524,1.,-0.468997482913158));
#34128=CARTESIAN_POINT('Ctrl Pts',(-1.94289794196205,-1.,-0.465645462026064));
#34129=CARTESIAN_POINT('Ctrl Pts',(-1.94289794196205,1.,-0.465645462026064));
#34130=CARTESIAN_POINT('Ctrl Pts',(-1.93781486640834,-1.,-0.462340031009087));
#34131=CARTESIAN_POINT('Ctrl Pts',(-1.93781486640834,1.,-0.462340031009087));
#34132=CARTESIAN_POINT('Ctrl Pts',(-1.93269066517936,-1.,-0.459081234547931));
#34133=CARTESIAN_POINT('Ctrl Pts',(-1.93269066517936,1.,-0.459081234547931));
#34134=CARTESIAN_POINT('Ctrl Pts',(-1.92753067150461,-1.,-0.455872005174335));
#34135=CARTESIAN_POINT('Ctrl Pts',(-1.92753067150461,1.,-0.455872005174335));
#34136=CARTESIAN_POINT('Ctrl Pts',(-1.9223538064847,-1.,-0.452719478359356));
#34137=CARTESIAN_POINT('Ctrl Pts',(-1.9223538064847,1.,-0.452719478359356));
#34138=CARTESIAN_POINT('Ctrl Pts',(-1.91718342555717,-1.,-0.449632260106572));
#34139=CARTESIAN_POINT('Ctrl Pts',(-1.91718342555717,1.,-0.449632260106572));
#34140=CARTESIAN_POINT('Ctrl Pts',(-1.91203699981095,-1.,-0.446617343485651));
#34141=CARTESIAN_POINT('Ctrl Pts',(-1.91203699981095,1.,-0.446617343485651));
#34142=CARTESIAN_POINT('Ctrl Pts',(-1.90691756144906,-1.,-0.44367755684917));
#34143=CARTESIAN_POINT('Ctrl Pts',(-1.90691756144906,1.,-0.44367755684917));
#34144=CARTESIAN_POINT('Ctrl Pts',(-1.90180124389137,-1.,-0.44080783370416));
#34145=CARTESIAN_POINT('Ctrl Pts',(-1.90180124389137,1.,-0.44080783370416));
#34146=CARTESIAN_POINT('Ctrl Pts',(-1.89663648956549,-1.,-0.437995003948443));
#34147=CARTESIAN_POINT('Ctrl Pts',(-1.89663648956549,1.,-0.437995003948443));
#34148=CARTESIAN_POINT('Ctrl Pts',(-1.89136993975585,-1.,-0.43522566096358));
#34149=CARTESIAN_POINT('Ctrl Pts',(-1.89136993975585,1.,-0.43522566096358));
#34150=CARTESIAN_POINT('Ctrl Pts',(-1.88596913666828,-1.,-0.432493038548833));
#34151=CARTESIAN_POINT('Ctrl Pts',(-1.88596913666828,1.,-0.432493038548833));
#34152=CARTESIAN_POINT('Ctrl Pts',(-1.88044229001778,-1.,-0.429803062482217));
#34153=CARTESIAN_POINT('Ctrl Pts',(-1.88044229001778,1.,-0.429803062482217));
#34154=CARTESIAN_POINT('Ctrl Pts',(-1.87486989291333,-1.,-0.427183828518743));
#34155=CARTESIAN_POINT('Ctrl Pts',(-1.87486989291333,1.,-0.427183828518743));
#34156=CARTESIAN_POINT('Ctrl Pts',(-1.8693780394412,-1.,-0.424678177290876));
#34157=CARTESIAN_POINT('Ctrl Pts',(-1.8693780394412,1.,-0.424678177290876));
#34158=CARTESIAN_POINT('Ctrl Pts',(-1.86408083333863,-1.,-0.422327307417884));
#34159=CARTESIAN_POINT('Ctrl Pts',(-1.86408083333863,1.,-0.422327307417884));
#34160=CARTESIAN_POINT('Ctrl Pts',(-1.8590328109667,-1.,-0.420157287975583));
#34161=CARTESIAN_POINT('Ctrl Pts',(-1.8590328109667,1.,-0.420157287975583));
#34162=CARTESIAN_POINT('Ctrl Pts',(-1.8541763285645,-1.,-0.418164129144045));
#34163=CARTESIAN_POINT('Ctrl Pts',(-1.8541763285645,1.,-0.418164129144045));
#34164=CARTESIAN_POINT('Ctrl Pts',(-1.84929312930314,-1.,-0.416300022039885));
#34165=CARTESIAN_POINT('Ctrl Pts',(-1.84929312930314,1.,-0.416300022039885));
#34166=CARTESIAN_POINT('Ctrl Pts',(-1.84405757074218,-1.,-0.414487438255542));
#34167=CARTESIAN_POINT('Ctrl Pts',(-1.84405757074218,1.,-0.414487438255542));
#34168=CARTESIAN_POINT('Ctrl Pts',(-1.8380895347617,-1.,-0.412633125322945));
#34169=CARTESIAN_POINT('Ctrl Pts',(-1.8380895347617,1.,-0.412633125322945));
#34170=CARTESIAN_POINT('Ctrl Pts',(-1.83100408895047,-1.,-0.410641256301276));
#34171=CARTESIAN_POINT('Ctrl Pts',(-1.83100408895047,1.,-0.410641256301276));
#34172=CARTESIAN_POINT('Ctrl Pts',(-1.82247022677562,-1.,-0.408428948106227));
#34173=CARTESIAN_POINT('Ctrl Pts',(-1.82247022677562,1.,-0.408428948106227));
#34174=CARTESIAN_POINT('Ctrl Pts',(-1.81223801812013,-1.,-0.405933518407175));
#34175=CARTESIAN_POINT('Ctrl Pts',(-1.81223801812013,1.,-0.405933518407175));
#34176=CARTESIAN_POINT('Ctrl Pts',(-1.80012077173238,-1.,-0.403107976163396));
#34177=CARTESIAN_POINT('Ctrl Pts',(-1.80012077173238,1.,-0.403107976163396));
#34178=CARTESIAN_POINT('Ctrl Pts',(-1.78598826343754,-1.,-0.399919403774155));
#34179=CARTESIAN_POINT('Ctrl Pts',(-1.78598826343754,1.,-0.399919403774155));
#34180=CARTESIAN_POINT('Ctrl Pts',(-1.76975560043442,-1.,-0.396346196110688));
#34181=CARTESIAN_POINT('Ctrl Pts',(-1.76975560043442,1.,-0.396346196110688));
#34182=CARTESIAN_POINT('Ctrl Pts',(-1.75137405310193,-1.,-0.392375812285395));
#34183=CARTESIAN_POINT('Ctrl Pts',(-1.75137405310193,1.,-0.392375812285395));
#34184=CARTESIAN_POINT('Ctrl Pts',(-1.73493170972829,-1.,-0.388877023502615));
#34185=CARTESIAN_POINT('Ctrl Pts',(-1.73493170972829,1.,-0.388877023502615));
#34186=CARTESIAN_POINT('Ctrl Pts',(-1.72162022244582,-1.,-0.386070790323281));
#34187=CARTESIAN_POINT('Ctrl Pts',(-1.72162022244582,1.,-0.386070790323281));
#34188=CARTESIAN_POINT('Ctrl Pts',(-1.71231062891398,-1.,-0.384119047314215));
#34189=CARTESIAN_POINT('Ctrl Pts',(-1.71231062891398,1.,-0.384119047314215));
#34190=CARTESIAN_POINT('Ctrl Pts',(-1.7075470150345,-1.,-0.383122945602004));
#34191=CARTESIAN_POINT('Ctrl Pts',(-1.7075470150345,1.,-0.383122945602004));
#34192=CARTESIAN_POINT('',(-2.11275013067528,1.,-0.61342227326009));
#34193=CARTESIAN_POINT('Ctrl Pts',(-2.11275013067528,1.,-0.61342227326009));
#34194=CARTESIAN_POINT('Ctrl Pts',(-2.11187554260142,1.,-0.61246736556225));
#34195=CARTESIAN_POINT('Ctrl Pts',(-2.11012443807661,1.,-0.610560911691113));
#34196=CARTESIAN_POINT('Ctrl Pts',(-2.10749199615859,1.,-0.607711315456826));
#34197=CARTESIAN_POINT('Ctrl Pts',(-2.10397049887709,1.,-0.603932030738212));
#34198=CARTESIAN_POINT('Ctrl Pts',(-2.09954930865331,1.,-0.599241616422144));
#34199=CARTESIAN_POINT('Ctrl Pts',(-2.09510876220501,1.,-0.594585006052823));
#34200=CARTESIAN_POINT('Ctrl Pts',(-2.09064881812053,1.,-0.589962365403189));
#34201=CARTESIAN_POINT('Ctrl Pts',(-2.086169437277,1.,-0.585373918990895));
#34202=CARTESIAN_POINT('Ctrl Pts',(-2.08167059018138,1.,-0.580819952107257));
#34203=CARTESIAN_POINT('Ctrl Pts',(-2.07715226767361,1.,-0.576300797416274));
#34204=CARTESIAN_POINT('Ctrl Pts',(-2.07261449292757,1.,-0.571816823242411));
#34205=CARTESIAN_POINT('Ctrl Pts',(-2.06805732997383,1.,-0.567368421181229));
#34206=CARTESIAN_POINT('Ctrl Pts',(-2.06348090160697,1.,-0.562955993082574));
#34207=CARTESIAN_POINT('Ctrl Pts',(-2.05888537756571,1.,-0.558579940185467));
#34208=CARTESIAN_POINT('Ctrl Pts',(-2.05427091604482,1.,-0.554240657464109));
#34209=CARTESIAN_POINT('Ctrl Pts',(-2.04963761077974,1.,-0.549938525150342));
#34210=CARTESIAN_POINT('Ctrl Pts',(-2.0449854471456,1.,-0.545673903817348));
#34211=CARTESIAN_POINT('Ctrl Pts',(-2.0403142269048,1.,-0.54144712061552));
#34212=CARTESIAN_POINT('Ctrl Pts',(-2.03562362953993,1.,-0.537258489833134));
#34213=CARTESIAN_POINT('Ctrl Pts',(-2.03091336214401,1.,-0.533108355132905));
#34214=CARTESIAN_POINT('Ctrl Pts',(-2.02618329083289,1.,-0.52899712724191));
#34215=CARTESIAN_POINT('Ctrl Pts',(-2.02143356304712,1.,-0.524925318333518));
#34216=CARTESIAN_POINT('Ctrl Pts',(-2.01666477917305,1.,-0.520893590399428));
#34217=CARTESIAN_POINT('Ctrl Pts',(-2.01187773939257,1.,-0.516902681728733));
#34218=CARTESIAN_POINT('Ctrl Pts',(-2.00707309946955,1.,-0.512953306961813));
#34219=CARTESIAN_POINT('Ctrl Pts',(-2.00225107134733,1.,-0.509046069886152));
#34220=CARTESIAN_POINT('Ctrl Pts',(-1.99741107463567,1.,-0.505181361323011));
#34221=CARTESIAN_POINT('Ctrl Pts',(-1.9925514912615,1.,-0.501359287727129));
#34222=CARTESIAN_POINT('Ctrl Pts',(-1.98767044752929,1.,-0.497579909545564));
#34223=CARTESIAN_POINT('Ctrl Pts',(-1.9827665876182,1.,-0.493843476541492));
#34224=CARTESIAN_POINT('Ctrl Pts',(-1.97783973019229,1.,-0.490150627860955));
#34225=CARTESIAN_POINT('Ctrl Pts',(-1.97289186263272,1.,-0.486502692907661));
#34226=CARTESIAN_POINT('Ctrl Pts',(-1.96792703422358,1.,-0.482901662120686));
#34227=CARTESIAN_POINT('Ctrl Pts',(-1.96294933055938,1.,-0.479349583074846));
#34228=CARTESIAN_POINT('Ctrl Pts',(-1.95796111148175,1.,-0.475848034683171));
#34229=CARTESIAN_POINT('Ctrl Pts',(-1.95296148278136,1.,-0.472397672264079));
#34230=CARTESIAN_POINT('Ctrl Pts',(-1.94794381136524,1.,-0.468997482913158));
#34231=CARTESIAN_POINT('Ctrl Pts',(-1.94289794196205,1.,-0.465645462026064));
#34232=CARTESIAN_POINT('Ctrl Pts',(-1.93781486640834,1.,-0.462340031009087));
#34233=CARTESIAN_POINT('Ctrl Pts',(-1.93269066517936,1.,-0.459081234547931));
#34234=CARTESIAN_POINT('Ctrl Pts',(-1.92753067150461,1.,-0.455872005174335));
#34235=CARTESIAN_POINT('Ctrl Pts',(-1.9223538064847,1.,-0.452719478359356));
#34236=CARTESIAN_POINT('Ctrl Pts',(-1.91718342555717,1.,-0.449632260106572));
#34237=CARTESIAN_POINT('Ctrl Pts',(-1.91203699981095,1.,-0.446617343485651));
#34238=CARTESIAN_POINT('Ctrl Pts',(-1.90691756144906,1.,-0.44367755684917));
#34239=CARTESIAN_POINT('Ctrl Pts',(-1.90180124389137,1.,-0.44080783370416));
#34240=CARTESIAN_POINT('Ctrl Pts',(-1.89663648956549,1.,-0.437995003948443));
#34241=CARTESIAN_POINT('Ctrl Pts',(-1.89136993975585,1.,-0.43522566096358));
#34242=CARTESIAN_POINT('Ctrl Pts',(-1.88596913666828,1.,-0.432493038548833));
#34243=CARTESIAN_POINT('Ctrl Pts',(-1.88044229001778,1.,-0.429803062482217));
#34244=CARTESIAN_POINT('Ctrl Pts',(-1.87486989291333,1.,-0.427183828518743));
#34245=CARTESIAN_POINT('Ctrl Pts',(-1.8693780394412,1.,-0.424678177290876));
#34246=CARTESIAN_POINT('Ctrl Pts',(-1.86408083333863,1.,-0.422327307417884));
#34247=CARTESIAN_POINT('Ctrl Pts',(-1.8590328109667,1.,-0.420157287975583));
#34248=CARTESIAN_POINT('Ctrl Pts',(-1.8541763285645,1.,-0.418164129144045));
#34249=CARTESIAN_POINT('Ctrl Pts',(-1.84929312930314,1.,-0.416300022039885));
#34250=CARTESIAN_POINT('Ctrl Pts',(-1.84405757074218,1.,-0.414487438255542));
#34251=CARTESIAN_POINT('Ctrl Pts',(-1.8380895347617,1.,-0.412633125322945));
#34252=CARTESIAN_POINT('Ctrl Pts',(-1.83100408895047,1.,-0.410641256301276));
#34253=CARTESIAN_POINT('Ctrl Pts',(-1.82247022677562,1.,-0.408428948106227));
#34254=CARTESIAN_POINT('Ctrl Pts',(-1.81223801812013,1.,-0.405933518407175));
#34255=CARTESIAN_POINT('Ctrl Pts',(-1.80012077173238,1.,-0.403107976163396));
#34256=CARTESIAN_POINT('Ctrl Pts',(-1.78598826343754,1.,-0.399919403774155));
#34257=CARTESIAN_POINT('Ctrl Pts',(-1.76975560043442,1.,-0.396346196110688));
#34258=CARTESIAN_POINT('Ctrl Pts',(-1.75137405310193,1.,-0.392375812285395));
#34259=CARTESIAN_POINT('Ctrl Pts',(-1.73493170972829,1.,-0.388877023502615));
#34260=CARTESIAN_POINT('Ctrl Pts',(-1.72162022244582,1.,-0.386070790323281));
#34261=CARTESIAN_POINT('Ctrl Pts',(-1.71231062891398,1.,-0.384119047314215));
#34262=CARTESIAN_POINT('Ctrl Pts',(-1.7075470150345,1.,-0.383122945602004));
#34263=CARTESIAN_POINT('',(-2.11275013067528,0.,-0.61342227326009));
#34264=CARTESIAN_POINT('Origin',(-2.0698113262342,0.,-0.745574324794401));
#34265=CARTESIAN_POINT('',(-2.0698113262342,1.,-0.745574324794401));
#34266=CARTESIAN_POINT('',(-2.11275013067528,1.,-0.61342227326009));
#34267=CARTESIAN_POINT('',(-2.0698113262342,0.,-0.745574324794401));
#34268=CARTESIAN_POINT('Ctrl Pts',(-1.60662857109684,-1.,-0.693717979106306));
#34269=CARTESIAN_POINT('Ctrl Pts',(-1.60662857109684,1.,-0.693717979106306));
#34270=CARTESIAN_POINT('Ctrl Pts',(-1.61106790958151,-1.,-0.695712097881194));
#34271=CARTESIAN_POINT('Ctrl Pts',(-1.61106790958151,1.,-0.695712097881194));
#34272=CARTESIAN_POINT('Ctrl Pts',(-1.61974673472612,-1.,-0.699605146405088));
#34273=CARTESIAN_POINT('Ctrl Pts',(-1.61974673472612,1.,-0.699605146405088));
#34274=CARTESIAN_POINT('Ctrl Pts',(-1.63216541664676,-1.,-0.705159151988319));
#34275=CARTESIAN_POINT('Ctrl Pts',(-1.63216541664676,1.,-0.705159151988319));
#34276=CARTESIAN_POINT('Ctrl Pts',(-1.64752408832016,-1.,-0.711993139355394));
#34277=CARTESIAN_POINT('Ctrl Pts',(-1.64752408832016,1.,-0.711993139355394));
#34278=CARTESIAN_POINT('Ctrl Pts',(-1.6647288055568,-1.,-0.719585433804282));
#34279=CARTESIAN_POINT('Ctrl Pts',(-1.6647288055568,1.,-0.719585433804282));
#34280=CARTESIAN_POINT('Ctrl Pts',(-1.67996158455503,-1.,-0.726235967997433));
#34281=CARTESIAN_POINT('Ctrl Pts',(-1.67996158455503,1.,-0.726235967997433));
#34282=CARTESIAN_POINT('Ctrl Pts',(-1.69326921975743,-1.,-0.731963238697195));
#34283=CARTESIAN_POINT('Ctrl Pts',(-1.69326921975743,1.,-0.731963238697195));
#34284=CARTESIAN_POINT('Ctrl Pts',(-1.70473309006121,-1.,-0.736799665724771));
#34285=CARTESIAN_POINT('Ctrl Pts',(-1.70473309006121,1.,-0.736799665724771));
#34286=CARTESIAN_POINT('Ctrl Pts',(-1.71447789751927,-1.,-0.740795162032087));
#34287=CARTESIAN_POINT('Ctrl Pts',(-1.71447789751927,1.,-0.740795162032087));
#34288=CARTESIAN_POINT('Ctrl Pts',(-1.7226822991693,-1.,-0.744021445433764));
#34289=CARTESIAN_POINT('Ctrl Pts',(-1.7226822991693,1.,-0.744021445433764));
#34290=CARTESIAN_POINT('Ctrl Pts',(-1.72958533647399,-1.,-0.746574710096436));
#34291=CARTESIAN_POINT('Ctrl Pts',(-1.72958533647399,1.,-0.746574710096436));
#34292=CARTESIAN_POINT('Ctrl Pts',(-1.73550351679848,-1.,-0.748582462954854));
#34293=CARTESIAN_POINT('Ctrl Pts',(-1.73550351679848,1.,-0.748582462954854));
#34294=CARTESIAN_POINT('Ctrl Pts',(-1.74080458266705,-1.,-0.75019343597954));
#34295=CARTESIAN_POINT('Ctrl Pts',(-1.74080458266705,1.,-0.75019343597954));
#34296=CARTESIAN_POINT('Ctrl Pts',(-1.74585086852298,-1.,-0.751555614163629));
#34297=CARTESIAN_POINT('Ctrl Pts',(-1.74585086852298,1.,-0.751555614163629));
#34298=CARTESIAN_POINT('Ctrl Pts',(-1.75095139468809,-1.,-0.752797683531377));
#34299=CARTESIAN_POINT('Ctrl Pts',(-1.75095139468809,1.,-0.752797683531377));
#34300=CARTESIAN_POINT('Ctrl Pts',(-1.75631083600175,-1.,-0.75400925402848));
#34301=CARTESIAN_POINT('Ctrl Pts',(-1.75631083600175,1.,-0.75400925402848));
#34302=CARTESIAN_POINT('Ctrl Pts',(-1.7619781724032,-1.,-0.755220979975262));
#34303=CARTESIAN_POINT('Ctrl Pts',(-1.7619781724032,1.,-0.755220979975262));
#34304=CARTESIAN_POINT('Ctrl Pts',(-1.76789396003141,-1.,-0.756421896028403));
#34305=CARTESIAN_POINT('Ctrl Pts',(-1.76789396003141,1.,-0.756421896028403));
#34306=CARTESIAN_POINT('Ctrl Pts',(-1.77394167108342,-1.,-0.757578264077238));
#34307=CARTESIAN_POINT('Ctrl Pts',(-1.77394167108342,1.,-0.757578264077238));
#34308=CARTESIAN_POINT('Ctrl Pts',(-1.77999411220912,-1.,-0.75865062667738));
#34309=CARTESIAN_POINT('Ctrl Pts',(-1.77999411220912,1.,-0.75865062667738));
#34310=CARTESIAN_POINT('Ctrl Pts',(-1.78596964884526,-1.,-0.759614401109868));
#34311=CARTESIAN_POINT('Ctrl Pts',(-1.78596964884526,1.,-0.759614401109868));
#34312=CARTESIAN_POINT('Ctrl Pts',(-1.79185815610802,-1.,-0.760469555880425));
#34313=CARTESIAN_POINT('Ctrl Pts',(-1.79185815610802,1.,-0.760469555880425));
#34314=CARTESIAN_POINT('Ctrl Pts',(-1.79768986997735,-1.,-0.761229695230359));
#34315=CARTESIAN_POINT('Ctrl Pts',(-1.79768986997735,1.,-0.761229695230359));
#34316=CARTESIAN_POINT('Ctrl Pts',(-1.80351583877334,-1.,-0.761915336443515));
#34317=CARTESIAN_POINT('Ctrl Pts',(-1.80351583877334,1.,-0.761915336443515));
#34318=CARTESIAN_POINT('Ctrl Pts',(-1.80938551463989,-1.,-0.762546129464036));
#34319=CARTESIAN_POINT('Ctrl Pts',(-1.80938551463989,1.,-0.762546129464036));
#34320=CARTESIAN_POINT('Ctrl Pts',(-1.81532118405566,-1.,-0.763132003836783));
#34321=CARTESIAN_POINT('Ctrl Pts',(-1.81532118405566,1.,-0.763132003836783));
#34322=CARTESIAN_POINT('Ctrl Pts',(-1.82131873145297,-1.,-0.763673465462854));
#34323=CARTESIAN_POINT('Ctrl Pts',(-1.82131873145297,1.,-0.763673465462854));
#34324=CARTESIAN_POINT('Ctrl Pts',(-1.8273599120008,-1.,-0.764165902606055));
#34325=CARTESIAN_POINT('Ctrl Pts',(-1.8273599120008,1.,-0.764165902606055));
#34326=CARTESIAN_POINT('Ctrl Pts',(-1.8334207722714,-1.,-0.764602549687845));
#34327=CARTESIAN_POINT('Ctrl Pts',(-1.8334207722714,1.,-0.764602549687845));
#34328=CARTESIAN_POINT('Ctrl Pts',(-1.83948181064823,-1.,-0.764978057881687));
#34329=CARTESIAN_POINT('Ctrl Pts',(-1.83948181064823,1.,-0.764978057881687));
#34330=CARTESIAN_POINT('Ctrl Pts',(-1.8455369887591,-1.,-0.765291664861971));
#34331=CARTESIAN_POINT('Ctrl Pts',(-1.8455369887591,1.,-0.765291664861971));
#34332=CARTESIAN_POINT('Ctrl Pts',(-1.85158945130054,-1.,-0.765545710619023));
#34333=CARTESIAN_POINT('Ctrl Pts',(-1.85158945130054,1.,-0.765545710619023));
#34334=CARTESIAN_POINT('Ctrl Pts',(-1.85764741390391,-1.,-0.765744212909305));
#34335=CARTESIAN_POINT('Ctrl Pts',(-1.85764741390391,1.,-0.765744212909305));
#34336=CARTESIAN_POINT('Ctrl Pts',(-1.86372027063314,-1.,-0.765891519092557));
#34337=CARTESIAN_POINT('Ctrl Pts',(-1.86372027063314,1.,-0.765891519092557));
#34338=CARTESIAN_POINT('Ctrl Pts',(-1.86981398314345,-1.,-0.765990708546111));
#34339=CARTESIAN_POINT('Ctrl Pts',(-1.86981398314345,1.,-0.765990708546111));
#34340=CARTESIAN_POINT('Ctrl Pts',(-1.87592888967886,-1.,-0.766042837036759));
#34341=CARTESIAN_POINT('Ctrl Pts',(-1.87592888967886,1.,-0.766042837036759));
#34342=CARTESIAN_POINT('Ctrl Pts',(-1.88206215302561,-1.,-0.766047794851868));
#34343=CARTESIAN_POINT('Ctrl Pts',(-1.88206215302561,1.,-0.766047794851868));
#34344=CARTESIAN_POINT('Ctrl Pts',(-1.88820926433409,-1.,-0.76600483706209));
#34345=CARTESIAN_POINT('Ctrl Pts',(-1.88820926433409,1.,-0.76600483706209));
#34346=CARTESIAN_POINT('Ctrl Pts',(-1.89436577771389,-1.,-0.765913193856979));
#34347=CARTESIAN_POINT('Ctrl Pts',(-1.89436577771389,1.,-0.765913193856979));
#34348=CARTESIAN_POINT('Ctrl Pts',(-1.90052930393599,-1.,-0.765772772593395));
#34349=CARTESIAN_POINT('Ctrl Pts',(-1.90052930393599,1.,-0.765772772593395));
#34350=CARTESIAN_POINT('Ctrl Pts',(-1.90669961402362,-1.,-0.765584196937936));
#34351=CARTESIAN_POINT('Ctrl Pts',(-1.90669961402362,1.,-0.765584196937936));
#34352=CARTESIAN_POINT('Ctrl Pts',(-1.91287765805174,-1.,-0.765348465884739));
#34353=CARTESIAN_POINT('Ctrl Pts',(-1.91287765805174,1.,-0.765348465884739));
#34354=CARTESIAN_POINT('Ctrl Pts',(-1.91906491634197,-1.,-0.765066729667095));
#34355=CARTESIAN_POINT('Ctrl Pts',(-1.91906491634197,1.,-0.765066729667095));
#34356=CARTESIAN_POINT('Ctrl Pts',(-1.92526263537041,-1.,-0.764740025488189));
#34357=CARTESIAN_POINT('Ctrl Pts',(-1.92526263537041,1.,-0.764740025488189));
#34358=CARTESIAN_POINT('Ctrl Pts',(-1.93147105496367,-1.,-0.764369010673889));
#34359=CARTESIAN_POINT('Ctrl Pts',(-1.93147105496367,1.,-0.764369010673889));
#34360=CARTESIAN_POINT('Ctrl Pts',(-1.93768964875867,-1.,-0.763954049121393));
#34361=CARTESIAN_POINT('Ctrl Pts',(-1.93768964875867,1.,-0.763954049121393));
#34362=CARTESIAN_POINT('Ctrl Pts',(-1.94391746617626,-1.,-0.76349533353858));
#34363=CARTESIAN_POINT('Ctrl Pts',(-1.94391746617626,1.,-0.76349533353858));
#34364=CARTESIAN_POINT('Ctrl Pts',(-1.95015342590025,-1.,-0.762992990878774));
#34365=CARTESIAN_POINT('Ctrl Pts',(-1.95015342590025,1.,-0.762992990878774));
#34366=CARTESIAN_POINT('Ctrl Pts',(-1.95639665309893,-1.,-0.762447203806263));
#34367=CARTESIAN_POINT('Ctrl Pts',(-1.95639665309893,1.,-0.762447203806263));
#34368=CARTESIAN_POINT('Ctrl Pts',(-1.96264672744229,-1.,-0.761858300014575));
#34369=CARTESIAN_POINT('Ctrl Pts',(-1.96264672744229,1.,-0.761858300014575));
#34370=CARTESIAN_POINT('Ctrl Pts',(-1.96890351582545,-1.,-0.761226690483986));
#34371=CARTESIAN_POINT('Ctrl Pts',(-1.96890351582545,1.,-0.761226690483986));
#34372=CARTESIAN_POINT('Ctrl Pts',(-1.97516705321521,-1.,-0.760552825409855));
#34373=CARTESIAN_POINT('Ctrl Pts',(-1.97516705321521,1.,-0.760552825409855));
#34374=CARTESIAN_POINT('Ctrl Pts',(-1.98143741418156,-1.,-0.759837147452135));
#34375=CARTESIAN_POINT('Ctrl Pts',(-1.98143741418156,1.,-0.759837147452135));
#34376=CARTESIAN_POINT('Ctrl Pts',(-1.98771456680806,-1.,-0.759080037802242));
#34377=CARTESIAN_POINT('Ctrl Pts',(-1.98771456680806,1.,-0.759080037802242));
#34378=CARTESIAN_POINT('Ctrl Pts',(-1.9939983109871,-1.,-0.758281796766377));
#34379=CARTESIAN_POINT('Ctrl Pts',(-1.9939983109871,1.,-0.758281796766377));
#34380=CARTESIAN_POINT('Ctrl Pts',(-2.00028834739072,-1.,-0.757442676862341));
#34381=CARTESIAN_POINT('Ctrl Pts',(-2.00028834739072,1.,-0.757442676862341));
#34382=CARTESIAN_POINT('Ctrl Pts',(-2.00658431587682,-1.,-0.756562904646496));
#34383=CARTESIAN_POINT('Ctrl Pts',(-2.00658431587682,1.,-0.756562904646496));
#34384=CARTESIAN_POINT('Ctrl Pts',(-2.01288584328149,-1.,-0.7556427049581));
#34385=CARTESIAN_POINT('Ctrl Pts',(-2.01288584328149,1.,-0.7556427049581));
#34386=CARTESIAN_POINT('Ctrl Pts',(-2.01919259406003,-1.,-0.75468233072352));
#34387=CARTESIAN_POINT('Ctrl Pts',(-2.01919259406003,1.,-0.75468233072352));
#34388=CARTESIAN_POINT('Ctrl Pts',(-2.02550428623587,-1.,-0.753682061113765));
#34389=CARTESIAN_POINT('Ctrl Pts',(-2.02550428623587,1.,-0.753682061113765));
#34390=CARTESIAN_POINT('Ctrl Pts',(-2.03182068456467,-1.,-0.752642180488104));
#34391=CARTESIAN_POINT('Ctrl Pts',(-2.03182068456467,1.,-0.752642180488104));
#34392=CARTESIAN_POINT('Ctrl Pts',(-2.03814160092173,-1.,-0.751562963361383));
#34393=CARTESIAN_POINT('Ctrl Pts',(-2.03814160092173,1.,-0.751562963361383));
#34394=CARTESIAN_POINT('Ctrl Pts',(-2.04446689147754,-1.,-0.750444657874758));
#34395=CARTESIAN_POINT('Ctrl Pts',(-2.04446689147754,1.,-0.750444657874758));
#34396=CARTESIAN_POINT('Ctrl Pts',(-2.05079645591606,-1.,-0.749287468663053));
#34397=CARTESIAN_POINT('Ctrl Pts',(-2.05079645591606,1.,-0.749287468663053));
#34398=CARTESIAN_POINT('Ctrl Pts',(-2.05713023030263,-1.,-0.748091554181101));
#34399=CARTESIAN_POINT('Ctrl Pts',(-2.05713023030263,1.,-0.748091554181101));
#34400=CARTESIAN_POINT('Ctrl Pts',(-2.06220058927162,-1.,-0.747103932785504));
#34401=CARTESIAN_POINT('Ctrl Pts',(-2.06220058927162,1.,-0.747103932785504));
#34402=CARTESIAN_POINT('Ctrl Pts',(-2.06600523016401,-1.,-0.746345871542695));
#34403=CARTESIAN_POINT('Ctrl Pts',(-2.06600523016401,1.,-0.746345871542695));
#34404=CARTESIAN_POINT('Ctrl Pts',(-2.06854248895575,-1.,-0.74583279137781));
#34405=CARTESIAN_POINT('Ctrl Pts',(-2.06854248895575,1.,-0.74583279137781));
#34406=CARTESIAN_POINT('Ctrl Pts',(-2.0698113262342,-1.,-0.745574324794401));
#34407=CARTESIAN_POINT('Ctrl Pts',(-2.0698113262342,1.,-0.745574324794401));
#34408=CARTESIAN_POINT('',(-1.60662857109684,1.,-0.693717979106306));
#34409=CARTESIAN_POINT('Ctrl Pts',(-1.60662857109684,1.,-0.693717979106306));
#34410=CARTESIAN_POINT('Ctrl Pts',(-1.61106790958151,1.,-0.695712097881194));
#34411=CARTESIAN_POINT('Ctrl Pts',(-1.61974673472612,1.,-0.699605146405088));
#34412=CARTESIAN_POINT('Ctrl Pts',(-1.63216541664676,1.,-0.705159151988319));
#34413=CARTESIAN_POINT('Ctrl Pts',(-1.64752408832016,1.,-0.711993139355394));
#34414=CARTESIAN_POINT('Ctrl Pts',(-1.6647288055568,1.,-0.719585433804282));
#34415=CARTESIAN_POINT('Ctrl Pts',(-1.67996158455503,1.,-0.726235967997433));
#34416=CARTESIAN_POINT('Ctrl Pts',(-1.69326921975743,1.,-0.731963238697195));
#34417=CARTESIAN_POINT('Ctrl Pts',(-1.70473309006121,1.,-0.736799665724771));
#34418=CARTESIAN_POINT('Ctrl Pts',(-1.71447789751927,1.,-0.740795162032087));
#34419=CARTESIAN_POINT('Ctrl Pts',(-1.7226822991693,1.,-0.744021445433764));
#34420=CARTESIAN_POINT('Ctrl Pts',(-1.72958533647399,1.,-0.746574710096436));
#34421=CARTESIAN_POINT('Ctrl Pts',(-1.73550351679848,1.,-0.748582462954854));
#34422=CARTESIAN_POINT('Ctrl Pts',(-1.74080458266705,1.,-0.75019343597954));
#34423=CARTESIAN_POINT('Ctrl Pts',(-1.74585086852298,1.,-0.751555614163629));
#34424=CARTESIAN_POINT('Ctrl Pts',(-1.75095139468809,1.,-0.752797683531377));
#34425=CARTESIAN_POINT('Ctrl Pts',(-1.75631083600175,1.,-0.75400925402848));
#34426=CARTESIAN_POINT('Ctrl Pts',(-1.7619781724032,1.,-0.755220979975262));
#34427=CARTESIAN_POINT('Ctrl Pts',(-1.76789396003141,1.,-0.756421896028403));
#34428=CARTESIAN_POINT('Ctrl Pts',(-1.77394167108342,1.,-0.757578264077238));
#34429=CARTESIAN_POINT('Ctrl Pts',(-1.77999411220912,1.,-0.75865062667738));
#34430=CARTESIAN_POINT('Ctrl Pts',(-1.78596964884526,1.,-0.759614401109868));
#34431=CARTESIAN_POINT('Ctrl Pts',(-1.79185815610802,1.,-0.760469555880425));
#34432=CARTESIAN_POINT('Ctrl Pts',(-1.79768986997735,1.,-0.761229695230359));
#34433=CARTESIAN_POINT('Ctrl Pts',(-1.80351583877334,1.,-0.761915336443515));
#34434=CARTESIAN_POINT('Ctrl Pts',(-1.80938551463989,1.,-0.762546129464036));
#34435=CARTESIAN_POINT('Ctrl Pts',(-1.81532118405566,1.,-0.763132003836783));
#34436=CARTESIAN_POINT('Ctrl Pts',(-1.82131873145297,1.,-0.763673465462854));
#34437=CARTESIAN_POINT('Ctrl Pts',(-1.8273599120008,1.,-0.764165902606055));
#34438=CARTESIAN_POINT('Ctrl Pts',(-1.8334207722714,1.,-0.764602549687845));
#34439=CARTESIAN_POINT('Ctrl Pts',(-1.83948181064823,1.,-0.764978057881687));
#34440=CARTESIAN_POINT('Ctrl Pts',(-1.8455369887591,1.,-0.765291664861971));
#34441=CARTESIAN_POINT('Ctrl Pts',(-1.85158945130054,1.,-0.765545710619023));
#34442=CARTESIAN_POINT('Ctrl Pts',(-1.85764741390391,1.,-0.765744212909305));
#34443=CARTESIAN_POINT('Ctrl Pts',(-1.86372027063314,1.,-0.765891519092557));
#34444=CARTESIAN_POINT('Ctrl Pts',(-1.86981398314345,1.,-0.765990708546111));
#34445=CARTESIAN_POINT('Ctrl Pts',(-1.87592888967886,1.,-0.766042837036759));
#34446=CARTESIAN_POINT('Ctrl Pts',(-1.88206215302561,1.,-0.766047794851868));
#34447=CARTESIAN_POINT('Ctrl Pts',(-1.88820926433409,1.,-0.76600483706209));
#34448=CARTESIAN_POINT('Ctrl Pts',(-1.89436577771389,1.,-0.765913193856979));
#34449=CARTESIAN_POINT('Ctrl Pts',(-1.90052930393599,1.,-0.765772772593395));
#34450=CARTESIAN_POINT('Ctrl Pts',(-1.90669961402362,1.,-0.765584196937936));
#34451=CARTESIAN_POINT('Ctrl Pts',(-1.91287765805174,1.,-0.765348465884739));
#34452=CARTESIAN_POINT('Ctrl Pts',(-1.91906491634197,1.,-0.765066729667095));
#34453=CARTESIAN_POINT('Ctrl Pts',(-1.92526263537041,1.,-0.764740025488189));
#34454=CARTESIAN_POINT('Ctrl Pts',(-1.93147105496367,1.,-0.764369010673889));
#34455=CARTESIAN_POINT('Ctrl Pts',(-1.93768964875867,1.,-0.763954049121393));
#34456=CARTESIAN_POINT('Ctrl Pts',(-1.94391746617626,1.,-0.76349533353858));
#34457=CARTESIAN_POINT('Ctrl Pts',(-1.95015342590025,1.,-0.762992990878774));
#34458=CARTESIAN_POINT('Ctrl Pts',(-1.95639665309893,1.,-0.762447203806263));
#34459=CARTESIAN_POINT('Ctrl Pts',(-1.96264672744229,1.,-0.761858300014575));
#34460=CARTESIAN_POINT('Ctrl Pts',(-1.96890351582545,1.,-0.761226690483986));
#34461=CARTESIAN_POINT('Ctrl Pts',(-1.97516705321521,1.,-0.760552825409855));
#34462=CARTESIAN_POINT('Ctrl Pts',(-1.98143741418156,1.,-0.759837147452135));
#34463=CARTESIAN_POINT('Ctrl Pts',(-1.98771456680806,1.,-0.759080037802242));
#34464=CARTESIAN_POINT('Ctrl Pts',(-1.9939983109871,1.,-0.758281796766377));
#34465=CARTESIAN_POINT('Ctrl Pts',(-2.00028834739072,1.,-0.757442676862341));
#34466=CARTESIAN_POINT('Ctrl Pts',(-2.00658431587682,1.,-0.756562904646496));
#34467=CARTESIAN_POINT('Ctrl Pts',(-2.01288584328149,1.,-0.7556427049581));
#34468=CARTESIAN_POINT('Ctrl Pts',(-2.01919259406003,1.,-0.75468233072352));
#34469=CARTESIAN_POINT('Ctrl Pts',(-2.02550428623587,1.,-0.753682061113765));
#34470=CARTESIAN_POINT('Ctrl Pts',(-2.03182068456467,1.,-0.752642180488104));
#34471=CARTESIAN_POINT('Ctrl Pts',(-2.03814160092173,1.,-0.751562963361383));
#34472=CARTESIAN_POINT('Ctrl Pts',(-2.04446689147754,1.,-0.750444657874758));
#34473=CARTESIAN_POINT('Ctrl Pts',(-2.05079645591606,1.,-0.749287468663053));
#34474=CARTESIAN_POINT('Ctrl Pts',(-2.05713023030263,1.,-0.748091554181101));
#34475=CARTESIAN_POINT('Ctrl Pts',(-2.06220058927162,1.,-0.747103932785504));
#34476=CARTESIAN_POINT('Ctrl Pts',(-2.06600523016401,1.,-0.746345871542695));
#34477=CARTESIAN_POINT('Ctrl Pts',(-2.06854248895575,1.,-0.74583279137781));
#34478=CARTESIAN_POINT('Ctrl Pts',(-2.0698113262342,1.,-0.745574324794401));
#34479=CARTESIAN_POINT('',(-1.60662857109684,0.,-0.693717979106306));
#34480=CARTESIAN_POINT('Origin',(0.,0.,0.));
#34481=CARTESIAN_POINT('',(-1.5055822144029,1.,-0.892032620296855));
#34482=CARTESIAN_POINT('Origin',(0.,1.,0.));
#34483=CARTESIAN_POINT('',(-1.5055822144029,0.,-0.892032620296855));
#34484=CARTESIAN_POINT('Ctrl Pts',(-1.81978687191668,-1.,-1.23627494547115));
#34485=CARTESIAN_POINT('Ctrl Pts',(-1.81978687191668,1.,-1.23627494547115));
#34486=CARTESIAN_POINT('Ctrl Pts',(-1.81925017193666,-1.,-1.23509651170476));
#34487=CARTESIAN_POINT('Ctrl Pts',(-1.81925017193666,1.,-1.23509651170476));
#34488=CARTESIAN_POINT('Ctrl Pts',(-1.81817389921279,-1.,-1.2327422452705));
#34489=CARTESIAN_POINT('Ctrl Pts',(-1.81817389921279,1.,-1.2327422452705));
#34490=CARTESIAN_POINT('Ctrl Pts',(-1.8165508718364,-1.,-1.2292186489137));
#34491=CARTESIAN_POINT('Ctrl Pts',(-1.8165508718364,1.,-1.2292186489137));
#34492=CARTESIAN_POINT('Ctrl Pts',(-1.81436959210434,-1.,-1.2245361330495));
#34493=CARTESIAN_POINT('Ctrl Pts',(-1.81436959210434,1.,-1.2245361330495));
#34494=CARTESIAN_POINT('Ctrl Pts',(-1.81161420806656,-1.,-1.21870906103557));
#34495=CARTESIAN_POINT('Ctrl Pts',(-1.81161420806656,1.,-1.21870906103557));
#34496=CARTESIAN_POINT('Ctrl Pts',(-1.80882996917129,-1.,-1.21290815708314));
#34497=CARTESIAN_POINT('Ctrl Pts',(-1.80882996917129,1.,-1.21290815708314));
#34498=CARTESIAN_POINT('Ctrl Pts',(-1.80601678480707,-1.,-1.20713356605475));
#34499=CARTESIAN_POINT('Ctrl Pts',(-1.80601678480707,1.,-1.20713356605475));
#34500=CARTESIAN_POINT('Ctrl Pts',(-1.80317454838603,-1.,-1.20138548938974));
#34501=CARTESIAN_POINT('Ctrl Pts',(-1.80317454838603,1.,-1.20138548938974));
#34502=CARTESIAN_POINT('Ctrl Pts',(-1.80030314369879,-1.,-1.19566418930242));
#34503=CARTESIAN_POINT('Ctrl Pts',(-1.80030314369879,1.,-1.19566418930242));
#34504=CARTESIAN_POINT('Ctrl Pts',(-1.79740245923478,-1.,-1.18996997934445));
#34505=CARTESIAN_POINT('Ctrl Pts',(-1.79740245923478,1.,-1.18996997934445));
#34506=CARTESIAN_POINT('Ctrl Pts',(-1.79447240321515,-1.,-1.18430321697432));
#34507=CARTESIAN_POINT('Ctrl Pts',(-1.79447240321515,1.,-1.18430321697432));
#34508=CARTESIAN_POINT('Ctrl Pts',(-1.79151291552689,-1.,-1.17866429440809));
#34509=CARTESIAN_POINT('Ctrl Pts',(-1.79151291552689,1.,-1.17866429440809));
#34510=CARTESIAN_POINT('Ctrl Pts',(-1.78852398877616,-1.,-1.17305363177328));
#34511=CARTESIAN_POINT('Ctrl Pts',(-1.78852398877616,1.,-1.17305363177328));
#34512=CARTESIAN_POINT('Ctrl Pts',(-1.78550566040443,-1.,-1.16747166312303));
#34513=CARTESIAN_POINT('Ctrl Pts',(-1.78550566040443,1.,-1.16747166312303));
#34514=CARTESIAN_POINT('Ctrl Pts',(-1.78245795881009,-1.,-1.16191881298499));
#34515=CARTESIAN_POINT('Ctrl Pts',(-1.78245795881009,1.,-1.16191881298499));
#34516=CARTESIAN_POINT('Ctrl Pts',(-1.77938085564275,-1.,-1.15639547194698));
#34517=CARTESIAN_POINT('Ctrl Pts',(-1.77938085564275,1.,-1.15639547194698));
#34518=CARTESIAN_POINT('Ctrl Pts',(-1.7762742255701,-1.,-1.15090197841515));
#34519=CARTESIAN_POINT('Ctrl Pts',(-1.7762742255701,1.,-1.15090197841515));
#34520=CARTESIAN_POINT('Ctrl Pts',(-1.77313777896194,-1.,-1.1454385822692));
#34521=CARTESIAN_POINT('Ctrl Pts',(-1.77313777896194,1.,-1.1454385822692));
#34522=CARTESIAN_POINT('Ctrl Pts',(-1.76997111386769,-1.,-1.14000548336975));
#34523=CARTESIAN_POINT('Ctrl Pts',(-1.76997111386769,1.,-1.14000548336975));
#34524=CARTESIAN_POINT('Ctrl Pts',(-1.76677384551862,-1.,-1.1346029180462));
#34525=CARTESIAN_POINT('Ctrl Pts',(-1.76677384551862,1.,-1.1346029180462));
#34526=CARTESIAN_POINT('Ctrl Pts',(-1.7635457196617,-1.,-1.12923123555075));
#34527=CARTESIAN_POINT('Ctrl Pts',(-1.7635457196617,1.,-1.12923123555075));
#34528=CARTESIAN_POINT('Ctrl Pts',(-1.76028671825096,-1.,-1.12389096855086));
#34529=CARTESIAN_POINT('Ctrl Pts',(-1.76028671825096,1.,-1.12389096855086));
#34530=CARTESIAN_POINT('Ctrl Pts',(-1.75699720772105,-1.,-1.11858293216763));
#34531=CARTESIAN_POINT('Ctrl Pts',(-1.75699720772105,1.,-1.11858293216763));
#34532=CARTESIAN_POINT('Ctrl Pts',(-1.7536777209463,-1.,-1.11330807582551));
#34533=CARTESIAN_POINT('Ctrl Pts',(-1.7536777209463,1.,-1.11330807582551));
#34534=CARTESIAN_POINT('Ctrl Pts',(-1.7503286607592,-1.,-1.10806728183007));
#34535=CARTESIAN_POINT('Ctrl Pts',(-1.7503286607592,1.,-1.10806728183007));
#34536=CARTESIAN_POINT('Ctrl Pts',(-1.74695004214923,-1.,-1.10286118991143));
#34537=CARTESIAN_POINT('Ctrl Pts',(-1.74695004214923,1.,-1.10286118991143));
#34538=CARTESIAN_POINT('Ctrl Pts',(-1.74354119236208,-1.,-1.09768999241225));
#34539=CARTESIAN_POINT('Ctrl Pts',(-1.74354119236208,1.,-1.09768999241225));
#34540=CARTESIAN_POINT('Ctrl Pts',(-1.74010053962247,-1.,-1.09255329056493));
#34541=CARTESIAN_POINT('Ctrl Pts',(-1.74010053962247,1.,-1.09255329056493));
#34542=CARTESIAN_POINT('Ctrl Pts',(-1.73662628326091,-1.,-1.08745056285427));
#34543=CARTESIAN_POINT('Ctrl Pts',(-1.73662628326091,1.,-1.08745056285427));
#34544=CARTESIAN_POINT('Ctrl Pts',(-1.73311705663407,-1.,-1.08238162784749));
#34545=CARTESIAN_POINT('Ctrl Pts',(-1.73311705663407,1.,-1.08238162784749));
#34546=CARTESIAN_POINT('Ctrl Pts',(-1.72957248977424,-1.,-1.0773470373727));
#34547=CARTESIAN_POINT('Ctrl Pts',(-1.72957248977424,1.,-1.0773470373727));
#34548=CARTESIAN_POINT('Ctrl Pts',(-1.72599406198488,-1.,-1.07234866990252));
#34549=CARTESIAN_POINT('Ctrl Pts',(-1.72599406198488,1.,-1.07234866990252));
#34550=CARTESIAN_POINT('Ctrl Pts',(-1.72238500928453,-1.,-1.06738966975462));
#34551=CARTESIAN_POINT('Ctrl Pts',(-1.72238500928453,1.,-1.06738966975462));
#34552=CARTESIAN_POINT('Ctrl Pts',(-1.71874858456904,-1.,-1.06247324680647));
#34553=CARTESIAN_POINT('Ctrl Pts',(-1.71874858456904,1.,-1.06247324680647));
#34554=CARTESIAN_POINT('Ctrl Pts',(-1.7150865442702,-1.,-1.05760163192479));
#34555=CARTESIAN_POINT('Ctrl Pts',(-1.7150865442702,1.,-1.05760163192479));
#34556=CARTESIAN_POINT('Ctrl Pts',(-1.71139783543989,-1.,-1.05277517202855));
#34557=CARTESIAN_POINT('Ctrl Pts',(-1.71139783543989,1.,-1.05277517202855));
#34558=CARTESIAN_POINT('Ctrl Pts',(-1.70767646263649,-1.,-1.04799085404995));
#34559=CARTESIAN_POINT('Ctrl Pts',(-1.70767646263649,1.,-1.04799085404995));
#34560=CARTESIAN_POINT('Ctrl Pts',(-1.70391338707982,-1.,-1.04324363334554));
#34561=CARTESIAN_POINT('Ctrl Pts',(-1.70391338707982,1.,-1.04324363334554));
#34562=CARTESIAN_POINT('Ctrl Pts',(-1.70010052930962,-1.,-1.03852922490789));
#34563=CARTESIAN_POINT('Ctrl Pts',(-1.70010052930962,1.,-1.03852922490789));
#34564=CARTESIAN_POINT('Ctrl Pts',(-1.69623414782771,-1.,-1.03384646003588));
#34565=CARTESIAN_POINT('Ctrl Pts',(-1.69623414782771,1.,-1.03384646003588));
#34566=CARTESIAN_POINT('Ctrl Pts',(-1.69231840863458,-1.,-1.02919977579147));
#34567=CARTESIAN_POINT('Ctrl Pts',(-1.69231840863458,1.,-1.02919977579147));
#34568=CARTESIAN_POINT('Ctrl Pts',(-1.68836910178447,-1.,-1.02460180535255));
#34569=CARTESIAN_POINT('Ctrl Pts',(-1.68836910178447,1.,-1.02460180535255));
#34570=CARTESIAN_POINT('Ctrl Pts',(-1.68440578021706,-1.,-1.02006795074201));
#34571=CARTESIAN_POINT('Ctrl Pts',(-1.68440578021706,1.,-1.02006795074201));
#34572=CARTESIAN_POINT('Ctrl Pts',(-1.68044289894798,-1.,-1.01561026162773));
#34573=CARTESIAN_POINT('Ctrl Pts',(-1.68044289894798,1.,-1.01561026162773));
#34574=CARTESIAN_POINT('Ctrl Pts',(-1.67648246776464,-1.,-1.01123236493511));
#34575=CARTESIAN_POINT('Ctrl Pts',(-1.67648246776464,1.,-1.01123236493511));
#34576=CARTESIAN_POINT('Ctrl Pts',(-1.67250335383293,-1.,-1.00692206696414));
#34577=CARTESIAN_POINT('Ctrl Pts',(-1.67250335383293,1.,-1.00692206696414));
#34578=CARTESIAN_POINT('Ctrl Pts',(-1.66846059277303,-1.,-1.00265091003727));
#34579=CARTESIAN_POINT('Ctrl Pts',(-1.66846059277303,1.,-1.00265091003727));
#34580=CARTESIAN_POINT('Ctrl Pts',(-1.66430758030376,-1.,-0.998389654952758));
#34581=CARTESIAN_POINT('Ctrl Pts',(-1.66430758030376,1.,-0.998389654952758));
#34582=CARTESIAN_POINT('Ctrl Pts',(-1.66001553809947,-1.,-0.994121836661306));
#34583=CARTESIAN_POINT('Ctrl Pts',(-1.66001553809947,1.,-0.994121836661306));
#34584=CARTESIAN_POINT('Ctrl Pts',(-1.65559044289699,-1.,-0.989855627854165));
#34585=CARTESIAN_POINT('Ctrl Pts',(-1.65559044289699,1.,-0.989855627854165));
#34586=CARTESIAN_POINT('Ctrl Pts',(-1.65110016612638,-1.,-0.985642622920821));
#34587=CARTESIAN_POINT('Ctrl Pts',(-1.65110016612638,1.,-0.985642622920821));
#34588=CARTESIAN_POINT('Ctrl Pts',(-1.64665139190656,-1.,-0.981562530939489));
#34589=CARTESIAN_POINT('Ctrl Pts',(-1.64665139190656,1.,-0.981562530939489));
#34590=CARTESIAN_POINT('Ctrl Pts',(-1.64233990826687,-1.,-0.977689794119416));
#34591=CARTESIAN_POINT('Ctrl Pts',(-1.64233990826687,1.,-0.977689794119416));
#34592=CARTESIAN_POINT('Ctrl Pts',(-1.63820952658144,-1.,-0.974066058287418));
#34593=CARTESIAN_POINT('Ctrl Pts',(-1.63820952658144,1.,-0.974066058287418));
#34594=CARTESIAN_POINT('Ctrl Pts',(-1.63420665729798,-1.,-0.970669715997509));
#34595=CARTESIAN_POINT('Ctrl Pts',(-1.63420665729798,1.,-0.970669715997509));
#34596=CARTESIAN_POINT('Ctrl Pts',(-1.63013849959461,-1.,-0.967387853230345));
#34597=CARTESIAN_POINT('Ctrl Pts',(-1.63013849959461,1.,-0.967387853230345));
#34598=CARTESIAN_POINT('Ctrl Pts',(-1.62571930670187,-1.,-0.964046107040536));
#34599=CARTESIAN_POINT('Ctrl Pts',(-1.62571930670187,1.,-0.964046107040536));
#34600=CARTESIAN_POINT('Ctrl Pts',(-1.62061638140221,-1.,-0.960438326101729));
#34601=CARTESIAN_POINT('Ctrl Pts',(-1.62061638140221,1.,-0.960438326101729));
#34602=CARTESIAN_POINT('Ctrl Pts',(-1.61449324337085,-1.,-0.956354422920671));
#34603=CARTESIAN_POINT('Ctrl Pts',(-1.61449324337085,1.,-0.956354422920671));
#34604=CARTESIAN_POINT('Ctrl Pts',(-1.60706069896936,-1.,-0.951613284356035));
#34605=CARTESIAN_POINT('Ctrl Pts',(-1.60706069896936,1.,-0.951613284356035));
#34606=CARTESIAN_POINT('Ctrl Pts',(-1.59810042043673,-1.,-0.946078063315257));
#34607=CARTESIAN_POINT('Ctrl Pts',(-1.59810042043673,1.,-0.946078063315257));
#34608=CARTESIAN_POINT('Ctrl Pts',(-1.58744937487176,-1.,-0.939646377893399));
#34609=CARTESIAN_POINT('Ctrl Pts',(-1.58744937487176,1.,-0.939646377893399));
#34610=CARTESIAN_POINT('Ctrl Pts',(-1.57499388382243,-1.,-0.932246680108685));
#34611=CARTESIAN_POINT('Ctrl Pts',(-1.57499388382243,1.,-0.932246680108685));
#34612=CARTESIAN_POINT('Ctrl Pts',(-1.56065988578893,-1.,-0.923832188944341));
#34613=CARTESIAN_POINT('Ctrl Pts',(-1.56065988578893,1.,-0.923832188944341));
#34614=CARTESIAN_POINT('Ctrl Pts',(-1.54440491149498,-1.,-0.914375919026456));
#34615=CARTESIAN_POINT('Ctrl Pts',(-1.54440491149498,1.,-0.914375919026456));
#34616=CARTESIAN_POINT('Ctrl Pts',(-1.52984849887993,-1.,-0.905967409625651));
#34617=CARTESIAN_POINT('Ctrl Pts',(-1.52984849887993,1.,-0.905967409625651));
#34618=CARTESIAN_POINT('Ctrl Pts',(-1.51805569590094,-1.,-0.899185047483511));
#34619=CARTESIAN_POINT('Ctrl Pts',(-1.51805569590094,1.,-0.899185047483511));
#34620=CARTESIAN_POINT('Ctrl Pts',(-1.50980486806688,-1.,-0.894452006964543));
#34621=CARTESIAN_POINT('Ctrl Pts',(-1.50980486806688,1.,-0.894452006964543));
#34622=CARTESIAN_POINT('Ctrl Pts',(-1.5055822144029,-1.,-0.892032620296855));
#34623=CARTESIAN_POINT('Ctrl Pts',(-1.5055822144029,1.,-0.892032620296855));
#34624=CARTESIAN_POINT('',(-1.81978687191668,1.,-1.23627494547115));
#34625=CARTESIAN_POINT('Ctrl Pts',(-1.81978687191668,1.,-1.23627494547115));
#34626=CARTESIAN_POINT('Ctrl Pts',(-1.81925017193666,1.,-1.23509651170476));
#34627=CARTESIAN_POINT('Ctrl Pts',(-1.81817389921279,1.,-1.2327422452705));
#34628=CARTESIAN_POINT('Ctrl Pts',(-1.8165508718364,1.,-1.2292186489137));
#34629=CARTESIAN_POINT('Ctrl Pts',(-1.81436959210434,1.,-1.2245361330495));
#34630=CARTESIAN_POINT('Ctrl Pts',(-1.81161420806656,1.,-1.21870906103557));
#34631=CARTESIAN_POINT('Ctrl Pts',(-1.80882996917129,1.,-1.21290815708314));
#34632=CARTESIAN_POINT('Ctrl Pts',(-1.80601678480707,1.,-1.20713356605475));
#34633=CARTESIAN_POINT('Ctrl Pts',(-1.80317454838603,1.,-1.20138548938974));
#34634=CARTESIAN_POINT('Ctrl Pts',(-1.80030314369879,1.,-1.19566418930242));
#34635=CARTESIAN_POINT('Ctrl Pts',(-1.79740245923478,1.,-1.18996997934445));
#34636=CARTESIAN_POINT('Ctrl Pts',(-1.79447240321515,1.,-1.18430321697432));
#34637=CARTESIAN_POINT('Ctrl Pts',(-1.79151291552689,1.,-1.17866429440809));
#34638=CARTESIAN_POINT('Ctrl Pts',(-1.78852398877616,1.,-1.17305363177328));
#34639=CARTESIAN_POINT('Ctrl Pts',(-1.78550566040443,1.,-1.16747166312303));
#34640=CARTESIAN_POINT('Ctrl Pts',(-1.78245795881009,1.,-1.16191881298499));
#34641=CARTESIAN_POINT('Ctrl Pts',(-1.77938085564275,1.,-1.15639547194698));
#34642=CARTESIAN_POINT('Ctrl Pts',(-1.7762742255701,1.,-1.15090197841515));
#34643=CARTESIAN_POINT('Ctrl Pts',(-1.77313777896194,1.,-1.1454385822692));
#34644=CARTESIAN_POINT('Ctrl Pts',(-1.76997111386769,1.,-1.14000548336975));
#34645=CARTESIAN_POINT('Ctrl Pts',(-1.76677384551862,1.,-1.1346029180462));
#34646=CARTESIAN_POINT('Ctrl Pts',(-1.7635457196617,1.,-1.12923123555075));
#34647=CARTESIAN_POINT('Ctrl Pts',(-1.76028671825096,1.,-1.12389096855086));
#34648=CARTESIAN_POINT('Ctrl Pts',(-1.75699720772105,1.,-1.11858293216763));
#34649=CARTESIAN_POINT('Ctrl Pts',(-1.7536777209463,1.,-1.11330807582551));
#34650=CARTESIAN_POINT('Ctrl Pts',(-1.7503286607592,1.,-1.10806728183007));
#34651=CARTESIAN_POINT('Ctrl Pts',(-1.74695004214923,1.,-1.10286118991143));
#34652=CARTESIAN_POINT('Ctrl Pts',(-1.74354119236208,1.,-1.09768999241225));
#34653=CARTESIAN_POINT('Ctrl Pts',(-1.74010053962247,1.,-1.09255329056493));
#34654=CARTESIAN_POINT('Ctrl Pts',(-1.73662628326091,1.,-1.08745056285427));
#34655=CARTESIAN_POINT('Ctrl Pts',(-1.73311705663407,1.,-1.08238162784749));
#34656=CARTESIAN_POINT('Ctrl Pts',(-1.72957248977424,1.,-1.0773470373727));
#34657=CARTESIAN_POINT('Ctrl Pts',(-1.72599406198488,1.,-1.07234866990252));
#34658=CARTESIAN_POINT('Ctrl Pts',(-1.72238500928453,1.,-1.06738966975462));
#34659=CARTESIAN_POINT('Ctrl Pts',(-1.71874858456904,1.,-1.06247324680647));
#34660=CARTESIAN_POINT('Ctrl Pts',(-1.7150865442702,1.,-1.05760163192479));
#34661=CARTESIAN_POINT('Ctrl Pts',(-1.71139783543989,1.,-1.05277517202855));
#34662=CARTESIAN_POINT('Ctrl Pts',(-1.70767646263649,1.,-1.04799085404995));
#34663=CARTESIAN_POINT('Ctrl Pts',(-1.70391338707982,1.,-1.04324363334554));
#34664=CARTESIAN_POINT('Ctrl Pts',(-1.70010052930962,1.,-1.03852922490789));
#34665=CARTESIAN_POINT('Ctrl Pts',(-1.69623414782771,1.,-1.03384646003588));
#34666=CARTESIAN_POINT('Ctrl Pts',(-1.69231840863458,1.,-1.02919977579147));
#34667=CARTESIAN_POINT('Ctrl Pts',(-1.68836910178447,1.,-1.02460180535255));
#34668=CARTESIAN_POINT('Ctrl Pts',(-1.68440578021706,1.,-1.02006795074201));
#34669=CARTESIAN_POINT('Ctrl Pts',(-1.68044289894798,1.,-1.01561026162773));
#34670=CARTESIAN_POINT('Ctrl Pts',(-1.67648246776464,1.,-1.01123236493511));
#34671=CARTESIAN_POINT('Ctrl Pts',(-1.67250335383293,1.,-1.00692206696414));
#34672=CARTESIAN_POINT('Ctrl Pts',(-1.66846059277303,1.,-1.00265091003727));
#34673=CARTESIAN_POINT('Ctrl Pts',(-1.66430758030376,1.,-0.998389654952758));
#34674=CARTESIAN_POINT('Ctrl Pts',(-1.66001553809947,1.,-0.994121836661306));
#34675=CARTESIAN_POINT('Ctrl Pts',(-1.65559044289699,1.,-0.989855627854165));
#34676=CARTESIAN_POINT('Ctrl Pts',(-1.65110016612638,1.,-0.985642622920821));
#34677=CARTESIAN_POINT('Ctrl Pts',(-1.64665139190656,1.,-0.981562530939489));
#34678=CARTESIAN_POINT('Ctrl Pts',(-1.64233990826687,1.,-0.977689794119416));
#34679=CARTESIAN_POINT('Ctrl Pts',(-1.63820952658144,1.,-0.974066058287418));
#34680=CARTESIAN_POINT('Ctrl Pts',(-1.63420665729798,1.,-0.970669715997509));
#34681=CARTESIAN_POINT('Ctrl Pts',(-1.63013849959461,1.,-0.967387853230345));
#34682=CARTESIAN_POINT('Ctrl Pts',(-1.62571930670187,1.,-0.964046107040536));
#34683=CARTESIAN_POINT('Ctrl Pts',(-1.62061638140221,1.,-0.960438326101729));
#34684=CARTESIAN_POINT('Ctrl Pts',(-1.61449324337085,1.,-0.956354422920671));
#34685=CARTESIAN_POINT('Ctrl Pts',(-1.60706069896936,1.,-0.951613284356035));
#34686=CARTESIAN_POINT('Ctrl Pts',(-1.59810042043673,1.,-0.946078063315257));
#34687=CARTESIAN_POINT('Ctrl Pts',(-1.58744937487176,1.,-0.939646377893399));
#34688=CARTESIAN_POINT('Ctrl Pts',(-1.57499388382243,1.,-0.932246680108685));
#34689=CARTESIAN_POINT('Ctrl Pts',(-1.56065988578893,1.,-0.923832188944341));
#34690=CARTESIAN_POINT('Ctrl Pts',(-1.54440491149498,1.,-0.914375919026456));
#34691=CARTESIAN_POINT('Ctrl Pts',(-1.52984849887993,1.,-0.905967409625651));
#34692=CARTESIAN_POINT('Ctrl Pts',(-1.51805569590094,1.,-0.899185047483511));
#34693=CARTESIAN_POINT('Ctrl Pts',(-1.50980486806688,1.,-0.894452006964543));
#34694=CARTESIAN_POINT('Ctrl Pts',(-1.5055822144029,1.,-0.892032620296855));
#34695=CARTESIAN_POINT('',(-1.81978687191668,0.,-1.23627494547115));
#34696=CARTESIAN_POINT('Origin',(-1.73811241238545,0.,-1.34869019493419));
#34697=CARTESIAN_POINT('',(-1.73811241238545,1.,-1.34869019493419));
#34698=CARTESIAN_POINT('',(-1.81978687191668,1.,-1.23627494547115));
#34699=CARTESIAN_POINT('',(-1.73811241238545,0.,-1.34869019493419));
#34700=CARTESIAN_POINT('Ctrl Pts',(-1.31362392696032,-1.,-1.15624053661742));
#34701=CARTESIAN_POINT('Ctrl Pts',(-1.31362392696032,1.,-1.15624053661742));
#34702=CARTESIAN_POINT('Ctrl Pts',(-1.31722977216397,-1.,-1.15950888730809));
#34703=CARTESIAN_POINT('Ctrl Pts',(-1.31722977216397,1.,-1.15950888730809));
#34704=CARTESIAN_POINT('Ctrl Pts',(-1.32428080721772,-1.,-1.16589330093588));
#34705=CARTESIAN_POINT('Ctrl Pts',(-1.32428080721772,1.,-1.16589330093588));
#34706=CARTESIAN_POINT('Ctrl Pts',(-1.33437539347008,-1.,-1.17501305789857));
#34707=CARTESIAN_POINT('Ctrl Pts',(-1.33437539347008,1.,-1.17501305789857));
#34708=CARTESIAN_POINT('Ctrl Pts',(-1.34687054001093,-1.,-1.18625865667441));
#34709=CARTESIAN_POINT('Ctrl Pts',(-1.34687054001093,1.,-1.18625865667441));
#34710=CARTESIAN_POINT('Ctrl Pts',(-1.36088705043885,-1.,-1.1987959077932));
#34711=CARTESIAN_POINT('Ctrl Pts',(-1.36088705043885,1.,-1.1987959077932));
#34712=CARTESIAN_POINT('Ctrl Pts',(-1.37331915607905,-1.,-1.20982812925645));
#34713=CARTESIAN_POINT('Ctrl Pts',(-1.37331915607905,1.,-1.20982812925645));
#34714=CARTESIAN_POINT('Ctrl Pts',(-1.38420564527715,-1.,-1.21938737280852));
#34715=CARTESIAN_POINT('Ctrl Pts',(-1.38420564527715,1.,-1.21938737280852));
#34716=CARTESIAN_POINT('Ctrl Pts',(-1.39361389568796,-1.,-1.22752961899387));
#34717=CARTESIAN_POINT('Ctrl Pts',(-1.39361389568796,1.,-1.22752961899387));
#34718=CARTESIAN_POINT('Ctrl Pts',(-1.40164708206106,-1.,-1.23434087290423));
#34719=CARTESIAN_POINT('Ctrl Pts',(-1.40164708206106,1.,-1.23434087290423));
#34720=CARTESIAN_POINT('Ctrl Pts',(-1.40845295531283,-1.,-1.23994455029534));
#34721=CARTESIAN_POINT('Ctrl Pts',(-1.40845295531283,1.,-1.23994455029534));
#34722=CARTESIAN_POINT('Ctrl Pts',(-1.41422913175179,-1.,-1.24450600513056));
#34723=CARTESIAN_POINT('Ctrl Pts',(-1.41422913175179,1.,-1.24450600513056));
#34724=CARTESIAN_POINT('Ctrl Pts',(-1.41923722596025,-1.,-1.24824430986571));
#34725=CARTESIAN_POINT('Ctrl Pts',(-1.41923722596025,1.,-1.24824430986571));
#34726=CARTESIAN_POINT('Ctrl Pts',(-1.42378102115575,-1.,-1.2514145557001));
#34727=CARTESIAN_POINT('Ctrl Pts',(-1.42378102115575,1.,-1.2514145557001));
#34728=CARTESIAN_POINT('Ctrl Pts',(-1.42815938799387,-1.,-1.25426945222639));
#34729=CARTESIAN_POINT('Ctrl Pts',(-1.42815938799387,1.,-1.25426945222639));
#34730=CARTESIAN_POINT('Ctrl Pts',(-1.43262645609691,-1.,-1.25702687965755));
#34731=CARTESIAN_POINT('Ctrl Pts',(-1.43262645609691,1.,-1.25702687965755));
#34732=CARTESIAN_POINT('Ctrl Pts',(-1.43734919180848,-1.,-1.25983531012005));
#34733=CARTESIAN_POINT('Ctrl Pts',(-1.43734919180848,1.,-1.25983531012005));
#34734=CARTESIAN_POINT('Ctrl Pts',(-1.44236470511303,-1.,-1.26273903323859));
#34735=CARTESIAN_POINT('Ctrl Pts',(-1.44236470511303,1.,-1.26273903323859));
#34736=CARTESIAN_POINT('Ctrl Pts',(-1.44761985001662,-1.,-1.26570925118868));
#34737=CARTESIAN_POINT('Ctrl Pts',(-1.44761985001662,1.,-1.26570925118868));
#34738=CARTESIAN_POINT('Ctrl Pts',(-1.45301422764247,-1.,-1.2686778680489));
#34739=CARTESIAN_POINT('Ctrl Pts',(-1.45301422764247,1.,-1.2686778680489));
#34740=CARTESIAN_POINT('Ctrl Pts',(-1.45843906294697,-1.,-1.27156805265289));
#34741=CARTESIAN_POINT('Ctrl Pts',(-1.45843906294697,1.,-1.27156805265289));
#34742=CARTESIAN_POINT('Ctrl Pts',(-1.46382431332476,-1.,-1.27433119897822));
#34743=CARTESIAN_POINT('Ctrl Pts',(-1.46382431332476,1.,-1.27433119897822));
#34744=CARTESIAN_POINT('Ctrl Pts',(-1.46916035917133,-1.,-1.27696414831089));
#34745=CARTESIAN_POINT('Ctrl Pts',(-1.46916035917133,1.,-1.27696414831089));
#34746=CARTESIAN_POINT('Ctrl Pts',(-1.4744717526707,-1.,-1.2794891824849));
#34747=CARTESIAN_POINT('Ctrl Pts',(-1.4744717526707,1.,-1.2794891824849));
#34748=CARTESIAN_POINT('Ctrl Pts',(-1.47980070347095,-1.,-1.28194158939517));
#34749=CARTESIAN_POINT('Ctrl Pts',(-1.47980070347095,1.,-1.28194158939517));
#34750=CARTESIAN_POINT('Ctrl Pts',(-1.4851881711891,-1.,-1.28435533880201));
#34751=CARTESIAN_POINT('Ctrl Pts',(-1.4851881711891,1.,-1.28435533880201));
#34752=CARTESIAN_POINT('Ctrl Pts',(-1.4906522831278,-1.,-1.2867467611644));
#34753=CARTESIAN_POINT('Ctrl Pts',(-1.4906522831278,1.,-1.2867467611644));
#34754=CARTESIAN_POINT('Ctrl Pts',(-1.49618896881754,-1.,-1.28911506584254));
#34755=CARTESIAN_POINT('Ctrl Pts',(-1.49618896881754,1.,-1.28911506584254));
#34756=CARTESIAN_POINT('Ctrl Pts',(-1.50178230149776,-1.,-1.29145022885181));
#34757=CARTESIAN_POINT('Ctrl Pts',(-1.50178230149776,1.,-1.29145022885181));
#34758=CARTESIAN_POINT('Ctrl Pts',(-1.50741159078365,-1.,-1.29373841372842));
#34759=CARTESIAN_POINT('Ctrl Pts',(-1.50741159078365,1.,-1.29373841372842));
#34760=CARTESIAN_POINT('Ctrl Pts',(-1.51305994241402,-1.,-1.29596850710509));
#34761=CARTESIAN_POINT('Ctrl Pts',(-1.51305994241402,1.,-1.29596850710509));
#34762=CARTESIAN_POINT('Ctrl Pts',(-1.51872184912724,-1.,-1.29813791800747));
#34763=CARTESIAN_POINT('Ctrl Pts',(-1.51872184912724,1.,-1.29813791800747));
#34764=CARTESIAN_POINT('Ctrl Pts',(-1.52439957861062,-1.,-1.30024984366328));
#34765=CARTESIAN_POINT('Ctrl Pts',(-1.52439957861062,1.,-1.30024984366328));
#34766=CARTESIAN_POINT('Ctrl Pts',(-1.53009970283891,-1.,-1.30231064395568));
#34767=CARTESIAN_POINT('Ctrl Pts',(-1.53009970283891,1.,-1.30231064395568));
#34768=CARTESIAN_POINT('Ctrl Pts',(-1.53582981268977,-1.,-1.30432735639489));
#34769=CARTESIAN_POINT('Ctrl Pts',(-1.53582981268977,1.,-1.30432735639489));
#34770=CARTESIAN_POINT('Ctrl Pts',(-1.54159462645432,-1.,-1.30630475189556));
#34771=CARTESIAN_POINT('Ctrl Pts',(-1.54159462645432,1.,-1.30630475189556));
#34772=CARTESIAN_POINT('Ctrl Pts',(-1.54739413957185,-1.,-1.30824393907473));
#34773=CARTESIAN_POINT('Ctrl Pts',(-1.54739413957185,1.,-1.30824393907473));
#34774=CARTESIAN_POINT('Ctrl Pts',(-1.55322568759481,-1.,-1.31014393684222));
#34775=CARTESIAN_POINT('Ctrl Pts',(-1.55322568759481,1.,-1.31014393684222));
#34776=CARTESIAN_POINT('Ctrl Pts',(-1.55908521254821,-1.,-1.31200264341696));
#34777=CARTESIAN_POINT('Ctrl Pts',(-1.55908521254821,1.,-1.31200264341696));
#34778=CARTESIAN_POINT('Ctrl Pts',(-1.56496872402353,-1.,-1.31381795281002));
#34779=CARTESIAN_POINT('Ctrl Pts',(-1.56496872402353,1.,-1.31381795281002));
#34780=CARTESIAN_POINT('Ctrl Pts',(-1.57087397835723,-1.,-1.31558903860016));
#34781=CARTESIAN_POINT('Ctrl Pts',(-1.57087397835723,1.,-1.31558903860016));
#34782=CARTESIAN_POINT('Ctrl Pts',(-1.5768005650559,-1.,-1.31731642317187));
#34783=CARTESIAN_POINT('Ctrl Pts',(-1.5768005650559,1.,-1.31731642317187));
#34784=CARTESIAN_POINT('Ctrl Pts',(-1.58274907898834,-1.,-1.31900135021432));
#34785=CARTESIAN_POINT('Ctrl Pts',(-1.58274907898834,1.,-1.31900135021432));
#34786=CARTESIAN_POINT('Ctrl Pts',(-1.58872057258245,-1.,-1.32064537110892));
#34787=CARTESIAN_POINT('Ctrl Pts',(-1.58872057258245,1.,-1.32064537110892));
#34788=CARTESIAN_POINT('Ctrl Pts',(-1.59471591079403,-1.,-1.32224985747682));
#34789=CARTESIAN_POINT('Ctrl Pts',(-1.59471591079403,1.,-1.32224985747682));
#34790=CARTESIAN_POINT('Ctrl Pts',(-1.60073511858687,-1.,-1.32381550858256));
#34791=CARTESIAN_POINT('Ctrl Pts',(-1.60073511858687,1.,-1.32381550858256));
#34792=CARTESIAN_POINT('Ctrl Pts',(-1.60677758290954,-1.,-1.32534250785782));
#34793=CARTESIAN_POINT('Ctrl Pts',(-1.60677758290954,1.,-1.32534250785782));
#34794=CARTESIAN_POINT('Ctrl Pts',(-1.6128423401575,-1.,-1.32683074483356));
#34795=CARTESIAN_POINT('Ctrl Pts',(-1.6128423401575,1.,-1.32683074483356));
#34796=CARTESIAN_POINT('Ctrl Pts',(-1.61892832270724,-1.,-1.32828000610449));
#34797=CARTESIAN_POINT('Ctrl Pts',(-1.61892832270724,1.,-1.32828000610449));
#34798=CARTESIAN_POINT('Ctrl Pts',(-1.62503464209797,-1.,-1.3296901950568));
#34799=CARTESIAN_POINT('Ctrl Pts',(-1.62503464209797,1.,-1.3296901950568));
#34800=CARTESIAN_POINT('Ctrl Pts',(-1.63116079730923,-1.,-1.33106149345645));
#34801=CARTESIAN_POINT('Ctrl Pts',(-1.63116079730923,1.,-1.33106149345645));
#34802=CARTESIAN_POINT('Ctrl Pts',(-1.63730653475089,-1.,-1.33239425103724));
#34803=CARTESIAN_POINT('Ctrl Pts',(-1.63730653475089,1.,-1.33239425103724));
#34804=CARTESIAN_POINT('Ctrl Pts',(-1.6434717485603,-1.,-1.33368890676572));
#34805=CARTESIAN_POINT('Ctrl Pts',(-1.6434717485603,1.,-1.33368890676572));
#34806=CARTESIAN_POINT('Ctrl Pts',(-1.6496563728683,-1.,-1.33494590467993));
#34807=CARTESIAN_POINT('Ctrl Pts',(-1.6496563728683,1.,-1.33494590467993));
#34808=CARTESIAN_POINT('Ctrl Pts',(-1.65586025952593,-1.,-1.33616559745172));
#34809=CARTESIAN_POINT('Ctrl Pts',(-1.65586025952593,1.,-1.33616559745172));
#34810=CARTESIAN_POINT('Ctrl Pts',(-1.66208312541983,-1.,-1.33734820885262));
#34811=CARTESIAN_POINT('Ctrl Pts',(-1.66208312541983,1.,-1.33734820885262));
#34812=CARTESIAN_POINT('Ctrl Pts',(-1.66832460783989,-1.,-1.33849388654388));
#34813=CARTESIAN_POINT('Ctrl Pts',(-1.66832460783989,1.,-1.33849388654388));
#34814=CARTESIAN_POINT('Ctrl Pts',(-1.67458429426086,-1.,-1.3396027347034));
#34815=CARTESIAN_POINT('Ctrl Pts',(-1.67458429426086,1.,-1.3396027347034));
#34816=CARTESIAN_POINT('Ctrl Pts',(-1.68086176030362,-1.,-1.34067485185203));
#34817=CARTESIAN_POINT('Ctrl Pts',(-1.68086176030362,1.,-1.34067485185203));
#34818=CARTESIAN_POINT('Ctrl Pts',(-1.68715660868764,-1.,-1.341710374848));
#34819=CARTESIAN_POINT('Ctrl Pts',(-1.68715660868764,1.,-1.341710374848));
#34820=CARTESIAN_POINT('Ctrl Pts',(-1.6934684849687,-1.,-1.34270948206319));
#34821=CARTESIAN_POINT('Ctrl Pts',(-1.6934684849687,1.,-1.34270948206319));
#34822=CARTESIAN_POINT('Ctrl Pts',(-1.69979707754427,-1.,-1.34367237124483));
#34823=CARTESIAN_POINT('Ctrl Pts',(-1.69979707754427,1.,-1.34367237124483));
#34824=CARTESIAN_POINT('Ctrl Pts',(-1.70614212266738,-1.,-1.34459924533831));
#34825=CARTESIAN_POINT('Ctrl Pts',(-1.70614212266738,1.,-1.34459924533831));
#34826=CARTESIAN_POINT('Ctrl Pts',(-1.71250340686822,-1.,-1.34549029589416));
#34827=CARTESIAN_POINT('Ctrl Pts',(-1.71250340686822,1.,-1.34549029589416));
#34828=CARTESIAN_POINT('Ctrl Pts',(-1.7188807715049,-1.,-1.34634568653227));
#34829=CARTESIAN_POINT('Ctrl Pts',(-1.7188807715049,1.,-1.34634568653227));
#34830=CARTESIAN_POINT('Ctrl Pts',(-1.72527410680674,-1.,-1.34716554819527));
#34831=CARTESIAN_POINT('Ctrl Pts',(-1.72527410680674,1.,-1.34716554819527));
#34832=CARTESIAN_POINT('Ctrl Pts',(-1.7304014965394,-1.,-1.34779309152035));
#34833=CARTESIAN_POINT('Ctrl Pts',(-1.7304014965394,1.,-1.34779309152035));
#34834=CARTESIAN_POINT('Ctrl Pts',(-1.73425417885907,-1.,-1.34824783112887));
#34835=CARTESIAN_POINT('Ctrl Pts',(-1.73425417885907,1.,-1.34824783112887));
#34836=CARTESIAN_POINT('Ctrl Pts',(-1.73682580585691,-1.,-1.34854391898045));
#34837=CARTESIAN_POINT('Ctrl Pts',(-1.73682580585691,1.,-1.34854391898045));
#34838=CARTESIAN_POINT('Ctrl Pts',(-1.73811241238545,-1.,-1.34869019493419));
#34839=CARTESIAN_POINT('Ctrl Pts',(-1.73811241238545,1.,-1.34869019493419));
#34840=CARTESIAN_POINT('',(-1.31362392696032,1.,-1.15624053661742));
#34841=CARTESIAN_POINT('Ctrl Pts',(-1.31362392696032,1.,-1.15624053661742));
#34842=CARTESIAN_POINT('Ctrl Pts',(-1.31722977216397,1.,-1.15950888730809));
#34843=CARTESIAN_POINT('Ctrl Pts',(-1.32428080721772,1.,-1.16589330093588));
#34844=CARTESIAN_POINT('Ctrl Pts',(-1.33437539347008,1.,-1.17501305789857));
#34845=CARTESIAN_POINT('Ctrl Pts',(-1.34687054001093,1.,-1.18625865667441));
#34846=CARTESIAN_POINT('Ctrl Pts',(-1.36088705043885,1.,-1.1987959077932));
#34847=CARTESIAN_POINT('Ctrl Pts',(-1.37331915607905,1.,-1.20982812925645));
#34848=CARTESIAN_POINT('Ctrl Pts',(-1.38420564527715,1.,-1.21938737280852));
#34849=CARTESIAN_POINT('Ctrl Pts',(-1.39361389568796,1.,-1.22752961899387));
#34850=CARTESIAN_POINT('Ctrl Pts',(-1.40164708206106,1.,-1.23434087290423));
#34851=CARTESIAN_POINT('Ctrl Pts',(-1.40845295531283,1.,-1.23994455029534));
#34852=CARTESIAN_POINT('Ctrl Pts',(-1.41422913175179,1.,-1.24450600513056));
#34853=CARTESIAN_POINT('Ctrl Pts',(-1.41923722596025,1.,-1.24824430986571));
#34854=CARTESIAN_POINT('Ctrl Pts',(-1.42378102115575,1.,-1.2514145557001));
#34855=CARTESIAN_POINT('Ctrl Pts',(-1.42815938799387,1.,-1.25426945222639));
#34856=CARTESIAN_POINT('Ctrl Pts',(-1.43262645609691,1.,-1.25702687965755));
#34857=CARTESIAN_POINT('Ctrl Pts',(-1.43734919180848,1.,-1.25983531012005));
#34858=CARTESIAN_POINT('Ctrl Pts',(-1.44236470511303,1.,-1.26273903323859));
#34859=CARTESIAN_POINT('Ctrl Pts',(-1.44761985001662,1.,-1.26570925118868));
#34860=CARTESIAN_POINT('Ctrl Pts',(-1.45301422764247,1.,-1.2686778680489));
#34861=CARTESIAN_POINT('Ctrl Pts',(-1.45843906294697,1.,-1.27156805265289));
#34862=CARTESIAN_POINT('Ctrl Pts',(-1.46382431332476,1.,-1.27433119897822));
#34863=CARTESIAN_POINT('Ctrl Pts',(-1.46916035917133,1.,-1.27696414831089));
#34864=CARTESIAN_POINT('Ctrl Pts',(-1.4744717526707,1.,-1.2794891824849));
#34865=CARTESIAN_POINT('Ctrl Pts',(-1.47980070347095,1.,-1.28194158939517));
#34866=CARTESIAN_POINT('Ctrl Pts',(-1.4851881711891,1.,-1.28435533880201));
#34867=CARTESIAN_POINT('Ctrl Pts',(-1.4906522831278,1.,-1.2867467611644));
#34868=CARTESIAN_POINT('Ctrl Pts',(-1.49618896881754,1.,-1.28911506584254));
#34869=CARTESIAN_POINT('Ctrl Pts',(-1.50178230149776,1.,-1.29145022885181));
#34870=CARTESIAN_POINT('Ctrl Pts',(-1.50741159078365,1.,-1.29373841372842));
#34871=CARTESIAN_POINT('Ctrl Pts',(-1.51305994241402,1.,-1.29596850710509));
#34872=CARTESIAN_POINT('Ctrl Pts',(-1.51872184912724,1.,-1.29813791800747));
#34873=CARTESIAN_POINT('Ctrl Pts',(-1.52439957861062,1.,-1.30024984366328));
#34874=CARTESIAN_POINT('Ctrl Pts',(-1.53009970283891,1.,-1.30231064395568));
#34875=CARTESIAN_POINT('Ctrl Pts',(-1.53582981268977,1.,-1.30432735639489));
#34876=CARTESIAN_POINT('Ctrl Pts',(-1.54159462645432,1.,-1.30630475189556));
#34877=CARTESIAN_POINT('Ctrl Pts',(-1.54739413957185,1.,-1.30824393907473));
#34878=CARTESIAN_POINT('Ctrl Pts',(-1.55322568759481,1.,-1.31014393684222));
#34879=CARTESIAN_POINT('Ctrl Pts',(-1.55908521254821,1.,-1.31200264341696));
#34880=CARTESIAN_POINT('Ctrl Pts',(-1.56496872402353,1.,-1.31381795281002));
#34881=CARTESIAN_POINT('Ctrl Pts',(-1.57087397835723,1.,-1.31558903860016));
#34882=CARTESIAN_POINT('Ctrl Pts',(-1.5768005650559,1.,-1.31731642317187));
#34883=CARTESIAN_POINT('Ctrl Pts',(-1.58274907898834,1.,-1.31900135021432));
#34884=CARTESIAN_POINT('Ctrl Pts',(-1.58872057258245,1.,-1.32064537110892));
#34885=CARTESIAN_POINT('Ctrl Pts',(-1.59471591079403,1.,-1.32224985747682));
#34886=CARTESIAN_POINT('Ctrl Pts',(-1.60073511858687,1.,-1.32381550858256));
#34887=CARTESIAN_POINT('Ctrl Pts',(-1.60677758290954,1.,-1.32534250785782));
#34888=CARTESIAN_POINT('Ctrl Pts',(-1.6128423401575,1.,-1.32683074483356));
#34889=CARTESIAN_POINT('Ctrl Pts',(-1.61892832270724,1.,-1.32828000610449));
#34890=CARTESIAN_POINT('Ctrl Pts',(-1.62503464209797,1.,-1.3296901950568));
#34891=CARTESIAN_POINT('Ctrl Pts',(-1.63116079730923,1.,-1.33106149345645));
#34892=CARTESIAN_POINT('Ctrl Pts',(-1.63730653475089,1.,-1.33239425103724));
#34893=CARTESIAN_POINT('Ctrl Pts',(-1.6434717485603,1.,-1.33368890676572));
#34894=CARTESIAN_POINT('Ctrl Pts',(-1.6496563728683,1.,-1.33494590467993));
#34895=CARTESIAN_POINT('Ctrl Pts',(-1.65586025952593,1.,-1.33616559745172));
#34896=CARTESIAN_POINT('Ctrl Pts',(-1.66208312541983,1.,-1.33734820885262));
#34897=CARTESIAN_POINT('Ctrl Pts',(-1.66832460783989,1.,-1.33849388654388));
#34898=CARTESIAN_POINT('Ctrl Pts',(-1.67458429426086,1.,-1.3396027347034));
#34899=CARTESIAN_POINT('Ctrl Pts',(-1.68086176030362,1.,-1.34067485185203));
#34900=CARTESIAN_POINT('Ctrl Pts',(-1.68715660868764,1.,-1.341710374848));
#34901=CARTESIAN_POINT('Ctrl Pts',(-1.6934684849687,1.,-1.34270948206319));
#34902=CARTESIAN_POINT('Ctrl Pts',(-1.69979707754427,1.,-1.34367237124483));
#34903=CARTESIAN_POINT('Ctrl Pts',(-1.70614212266738,1.,-1.34459924533831));
#34904=CARTESIAN_POINT('Ctrl Pts',(-1.71250340686822,1.,-1.34549029589416));
#34905=CARTESIAN_POINT('Ctrl Pts',(-1.7188807715049,1.,-1.34634568653227));
#34906=CARTESIAN_POINT('Ctrl Pts',(-1.72527410680674,1.,-1.34716554819527));
#34907=CARTESIAN_POINT('Ctrl Pts',(-1.7304014965394,1.,-1.34779309152035));
#34908=CARTESIAN_POINT('Ctrl Pts',(-1.73425417885907,1.,-1.34824783112887));
#34909=CARTESIAN_POINT('Ctrl Pts',(-1.73682580585691,1.,-1.34854391898045));
#34910=CARTESIAN_POINT('Ctrl Pts',(-1.73811241238545,1.,-1.34869019493419));
#34911=CARTESIAN_POINT('',(-1.31362392696032,0.,-1.15624053661742));
#34912=CARTESIAN_POINT('Origin',(0.,0.,0.));
#34913=CARTESIAN_POINT('',(-1.15624053661742,1.,-1.31362392696033));
#34914=CARTESIAN_POINT('Origin',(0.,1.,0.));
#34915=CARTESIAN_POINT('',(-1.15624053661742,0.,-1.31362392696033));
#34916=CARTESIAN_POINT('Ctrl Pts',(-1.34869019493419,-1.,-1.73811241238545));
#34917=CARTESIAN_POINT('Ctrl Pts',(-1.34869019493419,1.,-1.73811241238545));
#34918=CARTESIAN_POINT('Ctrl Pts',(-1.34854391898145,-1.,-1.73682580585819));
#34919=CARTESIAN_POINT('Ctrl Pts',(-1.34854391898145,1.,-1.73682580585819));
#34920=CARTESIAN_POINT('Ctrl Pts',(-1.34824783113158,-1.,-1.73425417886255));
#34921=CARTESIAN_POINT('Ctrl Pts',(-1.34824783113158,1.,-1.73425417886255));
#34922=CARTESIAN_POINT('Ctrl Pts',(-1.3477930915247,-1.,-1.73040149654497));
#34923=CARTESIAN_POINT('Ctrl Pts',(-1.3477930915247,1.,-1.73040149654497));
#34924=CARTESIAN_POINT('Ctrl Pts',(-1.34716554820013,-1.,-1.72527410681298));
#34925=CARTESIAN_POINT('Ctrl Pts',(-1.34716554820013,1.,-1.72527410681298));
#34926=CARTESIAN_POINT('Ctrl Pts',(-1.34634568653586,-1.,-1.7188807715095));
#34927=CARTESIAN_POINT('Ctrl Pts',(-1.34634568653586,1.,-1.7188807715095));
#34928=CARTESIAN_POINT('Ctrl Pts',(-1.34549029589563,-1.,-1.71250340687011));
#34929=CARTESIAN_POINT('Ctrl Pts',(-1.34549029589563,1.,-1.71250340687011));
#34930=CARTESIAN_POINT('Ctrl Pts',(-1.34459924533783,-1.,-1.70614212266676));
#34931=CARTESIAN_POINT('Ctrl Pts',(-1.34459924533783,1.,-1.70614212266676));
#34932=CARTESIAN_POINT('Ctrl Pts',(-1.34367237124322,-1.,-1.69979707754221));
#34933=CARTESIAN_POINT('Ctrl Pts',(-1.34367237124322,1.,-1.69979707754221));
#34934=CARTESIAN_POINT('Ctrl Pts',(-1.34270948206139,-1.,-1.6934684849664));
#34935=CARTESIAN_POINT('Ctrl Pts',(-1.34270948206139,1.,-1.6934684849664));
#34936=CARTESIAN_POINT('Ctrl Pts',(-1.34171037484673,-1.,-1.68715660868602));
#34937=CARTESIAN_POINT('Ctrl Pts',(-1.34171037484673,1.,-1.68715660868602));
#34938=CARTESIAN_POINT('Ctrl Pts',(-1.3406748518516,-1.,-1.68086176030308));
#34939=CARTESIAN_POINT('Ctrl Pts',(-1.3406748518516,1.,-1.68086176030308));
#34940=CARTESIAN_POINT('Ctrl Pts',(-1.33960273470372,-1.,-1.67458429426126));
#34941=CARTESIAN_POINT('Ctrl Pts',(-1.33960273470372,1.,-1.67458429426126));
#34942=CARTESIAN_POINT('Ctrl Pts',(-1.33849388654458,-1.,-1.66832460784078));
#34943=CARTESIAN_POINT('Ctrl Pts',(-1.33849388654458,1.,-1.66832460784078));
#34944=CARTESIAN_POINT('Ctrl Pts',(-1.33734820885331,-1.,-1.66208312542073));
#34945=CARTESIAN_POINT('Ctrl Pts',(-1.33734820885331,1.,-1.66208312542073));
#34946=CARTESIAN_POINT('Ctrl Pts',(-1.33616559745217,-1.,-1.65586025952651));
#34947=CARTESIAN_POINT('Ctrl Pts',(-1.33616559745217,1.,-1.65586025952651));
#34948=CARTESIAN_POINT('Ctrl Pts',(-1.33494590468003,-1.,-1.64965637286843));
#34949=CARTESIAN_POINT('Ctrl Pts',(-1.33494590468003,1.,-1.64965637286843));
#34950=CARTESIAN_POINT('Ctrl Pts',(-1.33368890676554,-1.,-1.64347174856007));
#34951=CARTESIAN_POINT('Ctrl Pts',(-1.33368890676554,1.,-1.64347174856007));
#34952=CARTESIAN_POINT('Ctrl Pts',(-1.33239425103694,-1.,-1.6373065347505));
#34953=CARTESIAN_POINT('Ctrl Pts',(-1.33239425103694,1.,-1.6373065347505));
#34954=CARTESIAN_POINT('Ctrl Pts',(-1.33106149345618,-1.,-1.63116079730887));
#34955=CARTESIAN_POINT('Ctrl Pts',(-1.33106149345618,1.,-1.63116079730887));
#34956=CARTESIAN_POINT('Ctrl Pts',(-1.32969019505665,-1.,-1.62503464209777));
#34957=CARTESIAN_POINT('Ctrl Pts',(-1.32969019505665,1.,-1.62503464209777));
#34958=CARTESIAN_POINT('Ctrl Pts',(-1.32828000610448,-1.,-1.61892832270723));
#34959=CARTESIAN_POINT('Ctrl Pts',(-1.32828000610448,1.,-1.61892832270723));
#34960=CARTESIAN_POINT('Ctrl Pts',(-1.32683074483365,-1.,-1.61284234015762));
#34961=CARTESIAN_POINT('Ctrl Pts',(-1.32683074483365,1.,-1.61284234015762));
#34962=CARTESIAN_POINT('Ctrl Pts',(-1.32534250785794,-1.,-1.6067775829097));
#34963=CARTESIAN_POINT('Ctrl Pts',(-1.32534250785794,1.,-1.6067775829097));
#34964=CARTESIAN_POINT('Ctrl Pts',(-1.32381550858266,-1.,-1.600735118587));
#34965=CARTESIAN_POINT('Ctrl Pts',(-1.32381550858266,1.,-1.600735118587));
#34966=CARTESIAN_POINT('Ctrl Pts',(-1.32224985747686,-1.,-1.59471591079408));
#34967=CARTESIAN_POINT('Ctrl Pts',(-1.32224985747686,1.,-1.59471591079408));
#34968=CARTESIAN_POINT('Ctrl Pts',(-1.32064537110891,-1.,-1.58872057258244));
#34969=CARTESIAN_POINT('Ctrl Pts',(-1.32064537110891,1.,-1.58872057258244));
#34970=CARTESIAN_POINT('Ctrl Pts',(-1.31900135021428,-1.,-1.58274907898829));
#34971=CARTESIAN_POINT('Ctrl Pts',(-1.31900135021428,1.,-1.58274907898829));
#34972=CARTESIAN_POINT('Ctrl Pts',(-1.31731642317183,-1.,-1.57680056505585));
#34973=CARTESIAN_POINT('Ctrl Pts',(-1.31731642317183,1.,-1.57680056505585));
#34974=CARTESIAN_POINT('Ctrl Pts',(-1.31558903860015,-1.,-1.57087397835721));
#34975=CARTESIAN_POINT('Ctrl Pts',(-1.31558903860015,1.,-1.57087397835721));
#34976=CARTESIAN_POINT('Ctrl Pts',(-1.31381795281002,-1.,-1.56496872402352));
#34977=CARTESIAN_POINT('Ctrl Pts',(-1.31381795281002,1.,-1.56496872402352));
#34978=CARTESIAN_POINT('Ctrl Pts',(-1.31200264341696,-1.,-1.55908521254822));
#34979=CARTESIAN_POINT('Ctrl Pts',(-1.31200264341696,1.,-1.55908521254822));
#34980=CARTESIAN_POINT('Ctrl Pts',(-1.31014393684221,-1.,-1.55322568759481));
#34981=CARTESIAN_POINT('Ctrl Pts',(-1.31014393684221,1.,-1.55322568759481));
#34982=CARTESIAN_POINT('Ctrl Pts',(-1.30824393907471,-1.,-1.54739413957183));
#34983=CARTESIAN_POINT('Ctrl Pts',(-1.30824393907471,1.,-1.54739413957183));
#34984=CARTESIAN_POINT('Ctrl Pts',(-1.30630475189553,-1.,-1.54159462645428));
#34985=CARTESIAN_POINT('Ctrl Pts',(-1.30630475189553,1.,-1.54159462645428));
#34986=CARTESIAN_POINT('Ctrl Pts',(-1.30432735639487,-1.,-1.53582981268976));
#34987=CARTESIAN_POINT('Ctrl Pts',(-1.30432735639487,1.,-1.53582981268976));
#34988=CARTESIAN_POINT('Ctrl Pts',(-1.3023106439557,-1.,-1.53009970283893));
#34989=CARTESIAN_POINT('Ctrl Pts',(-1.3023106439557,1.,-1.53009970283893));
#34990=CARTESIAN_POINT('Ctrl Pts',(-1.30024984366334,-1.,-1.5243995786107));
#34991=CARTESIAN_POINT('Ctrl Pts',(-1.30024984366334,1.,-1.5243995786107));
#34992=CARTESIAN_POINT('Ctrl Pts',(-1.29813791800757,-1.,-1.51872184912735));
#34993=CARTESIAN_POINT('Ctrl Pts',(-1.29813791800757,1.,-1.51872184912735));
#34994=CARTESIAN_POINT('Ctrl Pts',(-1.29596850710518,-1.,-1.51305994241412));
#34995=CARTESIAN_POINT('Ctrl Pts',(-1.29596850710518,1.,-1.51305994241412));
#34996=CARTESIAN_POINT('Ctrl Pts',(-1.29373841372843,-1.,-1.50741159078367));
#34997=CARTESIAN_POINT('Ctrl Pts',(-1.29373841372843,1.,-1.50741159078367));
#34998=CARTESIAN_POINT('Ctrl Pts',(-1.29145022885171,-1.,-1.50178230149764));
#34999=CARTESIAN_POINT('Ctrl Pts',(-1.29145022885171,1.,-1.50178230149764));
#35000=CARTESIAN_POINT('Ctrl Pts',(-1.28911506584232,-1.,-1.49618896881729));
#35001=CARTESIAN_POINT('Ctrl Pts',(-1.28911506584232,1.,-1.49618896881729));
#35002=CARTESIAN_POINT('Ctrl Pts',(-1.28674676116415,-1.,-1.4906522831275));
#35003=CARTESIAN_POINT('Ctrl Pts',(-1.28674676116415,1.,-1.4906522831275));
#35004=CARTESIAN_POINT('Ctrl Pts',(-1.28435533880184,-1.,-1.48518817118891));
#35005=CARTESIAN_POINT('Ctrl Pts',(-1.28435533880184,1.,-1.48518817118891));
#35006=CARTESIAN_POINT('Ctrl Pts',(-1.28194158939522,-1.,-1.47980070347102));
#35007=CARTESIAN_POINT('Ctrl Pts',(-1.28194158939522,1.,-1.47980070347102));
#35008=CARTESIAN_POINT('Ctrl Pts',(-1.27948918248524,-1.,-1.4744717526711));
#35009=CARTESIAN_POINT('Ctrl Pts',(-1.27948918248524,1.,-1.4744717526711));
#35010=CARTESIAN_POINT('Ctrl Pts',(-1.27696414831144,-1.,-1.46916035917197));
#35011=CARTESIAN_POINT('Ctrl Pts',(-1.27696414831144,1.,-1.46916035917197));
#35012=CARTESIAN_POINT('Ctrl Pts',(-1.27433119897877,-1.,-1.4638243133254));
#35013=CARTESIAN_POINT('Ctrl Pts',(-1.27433119897877,1.,-1.4638243133254));
#35014=CARTESIAN_POINT('Ctrl Pts',(-1.27156805265312,-1.,-1.45843906294725));
#35015=CARTESIAN_POINT('Ctrl Pts',(-1.27156805265312,1.,-1.45843906294725));
#35016=CARTESIAN_POINT('Ctrl Pts',(-1.26867786804854,-1.,-1.45301422764205));
#35017=CARTESIAN_POINT('Ctrl Pts',(-1.26867786804854,1.,-1.45301422764205));
#35018=CARTESIAN_POINT('Ctrl Pts',(-1.26570925118767,-1.,-1.44761985001544));
#35019=CARTESIAN_POINT('Ctrl Pts',(-1.26570925118767,1.,-1.44761985001544));
#35020=CARTESIAN_POINT('Ctrl Pts',(-1.26273903323723,-1.,-1.44236470511145));
#35021=CARTESIAN_POINT('Ctrl Pts',(-1.26273903323723,1.,-1.44236470511145));
#35022=CARTESIAN_POINT('Ctrl Pts',(-1.25983531011894,-1.,-1.43734919180719));
#35023=CARTESIAN_POINT('Ctrl Pts',(-1.25983531011894,1.,-1.43734919180719));
#35024=CARTESIAN_POINT('Ctrl Pts',(-1.25702687965744,-1.,-1.43262645609679));
#35025=CARTESIAN_POINT('Ctrl Pts',(-1.25702687965744,1.,-1.43262645609679));
#35026=CARTESIAN_POINT('Ctrl Pts',(-1.25426945222783,-1.,-1.42815938799555));
#35027=CARTESIAN_POINT('Ctrl Pts',(-1.25426945222783,1.,-1.42815938799555));
#35028=CARTESIAN_POINT('Ctrl Pts',(-1.25141455570299,-1.,-1.42378102115911));
#35029=CARTESIAN_POINT('Ctrl Pts',(-1.25141455570299,1.,-1.42378102115911));
#35030=CARTESIAN_POINT('Ctrl Pts',(-1.24824430986911,-1.,-1.41923722596421));
#35031=CARTESIAN_POINT('Ctrl Pts',(-1.24824430986911,1.,-1.41923722596421));
#35032=CARTESIAN_POINT('Ctrl Pts',(-1.24450600513278,-1.,-1.41422913175437));
#35033=CARTESIAN_POINT('Ctrl Pts',(-1.24450600513278,1.,-1.41422913175437));
#35034=CARTESIAN_POINT('Ctrl Pts',(-1.23994455029421,-1.,-1.40845295531151));
#35035=CARTESIAN_POINT('Ctrl Pts',(-1.23994455029421,1.,-1.40845295531151));
#35036=CARTESIAN_POINT('Ctrl Pts',(-1.23434087289768,-1.,-1.40164708205345));
#35037=CARTESIAN_POINT('Ctrl Pts',(-1.23434087289768,1.,-1.40164708205345));
#35038=CARTESIAN_POINT('Ctrl Pts',(-1.22752961898063,-1.,-1.39361389567257));
#35039=CARTESIAN_POINT('Ctrl Pts',(-1.22752961898063,1.,-1.39361389567257));
#35040=CARTESIAN_POINT('Ctrl Pts',(-1.21938737278853,-1.,-1.38420564525391));
#35041=CARTESIAN_POINT('Ctrl Pts',(-1.21938737278853,1.,-1.38420564525391));
#35042=CARTESIAN_POINT('Ctrl Pts',(-1.20982812923113,-1.,-1.37331915604962));
#35043=CARTESIAN_POINT('Ctrl Pts',(-1.20982812923113,1.,-1.37331915604962));
#35044=CARTESIAN_POINT('Ctrl Pts',(-1.1987959077656,-1.,-1.36088705040677));
#35045=CARTESIAN_POINT('Ctrl Pts',(-1.1987959077656,1.,-1.36088705040677));
#35046=CARTESIAN_POINT('Ctrl Pts',(-1.18625865664915,-1.,-1.34687053998157));
#35047=CARTESIAN_POINT('Ctrl Pts',(-1.18625865664915,1.,-1.34687053998157));
#35048=CARTESIAN_POINT('Ctrl Pts',(-1.17501305787994,-1.,-1.33437539344842));
#35049=CARTESIAN_POINT('Ctrl Pts',(-1.17501305787994,1.,-1.33437539344842));
#35050=CARTESIAN_POINT('Ctrl Pts',(-1.16589330092532,-1.,-1.32428080720544));
#35051=CARTESIAN_POINT('Ctrl Pts',(-1.16589330092532,1.,-1.32428080720544));
#35052=CARTESIAN_POINT('Ctrl Pts',(-1.15950888730433,-1.,-1.3172297721596));
#35053=CARTESIAN_POINT('Ctrl Pts',(-1.15950888730433,1.,-1.3172297721596));
#35054=CARTESIAN_POINT('Ctrl Pts',(-1.15624053661742,-1.,-1.31362392696033));
#35055=CARTESIAN_POINT('Ctrl Pts',(-1.15624053661742,1.,-1.31362392696033));
#35056=CARTESIAN_POINT('',(-1.34869019493419,1.,-1.73811241238545));
#35057=CARTESIAN_POINT('Ctrl Pts',(-1.34869019493419,1.,-1.73811241238545));
#35058=CARTESIAN_POINT('Ctrl Pts',(-1.34854391898145,1.,-1.73682580585819));
#35059=CARTESIAN_POINT('Ctrl Pts',(-1.34824783113158,1.,-1.73425417886255));
#35060=CARTESIAN_POINT('Ctrl Pts',(-1.3477930915247,1.,-1.73040149654497));
#35061=CARTESIAN_POINT('Ctrl Pts',(-1.34716554820013,1.,-1.72527410681298));
#35062=CARTESIAN_POINT('Ctrl Pts',(-1.34634568653586,1.,-1.7188807715095));
#35063=CARTESIAN_POINT('Ctrl Pts',(-1.34549029589563,1.,-1.71250340687011));
#35064=CARTESIAN_POINT('Ctrl Pts',(-1.34459924533783,1.,-1.70614212266676));
#35065=CARTESIAN_POINT('Ctrl Pts',(-1.34367237124322,1.,-1.69979707754221));
#35066=CARTESIAN_POINT('Ctrl Pts',(-1.34270948206139,1.,-1.6934684849664));
#35067=CARTESIAN_POINT('Ctrl Pts',(-1.34171037484673,1.,-1.68715660868602));
#35068=CARTESIAN_POINT('Ctrl Pts',(-1.3406748518516,1.,-1.68086176030308));
#35069=CARTESIAN_POINT('Ctrl Pts',(-1.33960273470372,1.,-1.67458429426126));
#35070=CARTESIAN_POINT('Ctrl Pts',(-1.33849388654458,1.,-1.66832460784078));
#35071=CARTESIAN_POINT('Ctrl Pts',(-1.33734820885331,1.,-1.66208312542073));
#35072=CARTESIAN_POINT('Ctrl Pts',(-1.33616559745217,1.,-1.65586025952651));
#35073=CARTESIAN_POINT('Ctrl Pts',(-1.33494590468003,1.,-1.64965637286843));
#35074=CARTESIAN_POINT('Ctrl Pts',(-1.33368890676554,1.,-1.64347174856007));
#35075=CARTESIAN_POINT('Ctrl Pts',(-1.33239425103694,1.,-1.6373065347505));
#35076=CARTESIAN_POINT('Ctrl Pts',(-1.33106149345618,1.,-1.63116079730887));
#35077=CARTESIAN_POINT('Ctrl Pts',(-1.32969019505665,1.,-1.62503464209777));
#35078=CARTESIAN_POINT('Ctrl Pts',(-1.32828000610448,1.,-1.61892832270723));
#35079=CARTESIAN_POINT('Ctrl Pts',(-1.32683074483365,1.,-1.61284234015762));
#35080=CARTESIAN_POINT('Ctrl Pts',(-1.32534250785794,1.,-1.6067775829097));
#35081=CARTESIAN_POINT('Ctrl Pts',(-1.32381550858266,1.,-1.600735118587));
#35082=CARTESIAN_POINT('Ctrl Pts',(-1.32224985747686,1.,-1.59471591079408));
#35083=CARTESIAN_POINT('Ctrl Pts',(-1.32064537110891,1.,-1.58872057258244));
#35084=CARTESIAN_POINT('Ctrl Pts',(-1.31900135021428,1.,-1.58274907898829));
#35085=CARTESIAN_POINT('Ctrl Pts',(-1.31731642317183,1.,-1.57680056505585));
#35086=CARTESIAN_POINT('Ctrl Pts',(-1.31558903860015,1.,-1.57087397835721));
#35087=CARTESIAN_POINT('Ctrl Pts',(-1.31381795281002,1.,-1.56496872402352));
#35088=CARTESIAN_POINT('Ctrl Pts',(-1.31200264341696,1.,-1.55908521254822));
#35089=CARTESIAN_POINT('Ctrl Pts',(-1.31014393684221,1.,-1.55322568759481));
#35090=CARTESIAN_POINT('Ctrl Pts',(-1.30824393907471,1.,-1.54739413957183));
#35091=CARTESIAN_POINT('Ctrl Pts',(-1.30630475189553,1.,-1.54159462645428));
#35092=CARTESIAN_POINT('Ctrl Pts',(-1.30432735639487,1.,-1.53582981268976));
#35093=CARTESIAN_POINT('Ctrl Pts',(-1.3023106439557,1.,-1.53009970283893));
#35094=CARTESIAN_POINT('Ctrl Pts',(-1.30024984366334,1.,-1.5243995786107));
#35095=CARTESIAN_POINT('Ctrl Pts',(-1.29813791800757,1.,-1.51872184912735));
#35096=CARTESIAN_POINT('Ctrl Pts',(-1.29596850710518,1.,-1.51305994241412));
#35097=CARTESIAN_POINT('Ctrl Pts',(-1.29373841372843,1.,-1.50741159078367));
#35098=CARTESIAN_POINT('Ctrl Pts',(-1.29145022885171,1.,-1.50178230149764));
#35099=CARTESIAN_POINT('Ctrl Pts',(-1.28911506584232,1.,-1.49618896881729));
#35100=CARTESIAN_POINT('Ctrl Pts',(-1.28674676116415,1.,-1.4906522831275));
#35101=CARTESIAN_POINT('Ctrl Pts',(-1.28435533880184,1.,-1.48518817118891));
#35102=CARTESIAN_POINT('Ctrl Pts',(-1.28194158939522,1.,-1.47980070347102));
#35103=CARTESIAN_POINT('Ctrl Pts',(-1.27948918248524,1.,-1.4744717526711));
#35104=CARTESIAN_POINT('Ctrl Pts',(-1.27696414831144,1.,-1.46916035917197));
#35105=CARTESIAN_POINT('Ctrl Pts',(-1.27433119897877,1.,-1.4638243133254));
#35106=CARTESIAN_POINT('Ctrl Pts',(-1.27156805265312,1.,-1.45843906294725));
#35107=CARTESIAN_POINT('Ctrl Pts',(-1.26867786804854,1.,-1.45301422764205));
#35108=CARTESIAN_POINT('Ctrl Pts',(-1.26570925118767,1.,-1.44761985001544));
#35109=CARTESIAN_POINT('Ctrl Pts',(-1.26273903323723,1.,-1.44236470511145));
#35110=CARTESIAN_POINT('Ctrl Pts',(-1.25983531011894,1.,-1.43734919180719));
#35111=CARTESIAN_POINT('Ctrl Pts',(-1.25702687965744,1.,-1.43262645609679));
#35112=CARTESIAN_POINT('Ctrl Pts',(-1.25426945222783,1.,-1.42815938799555));
#35113=CARTESIAN_POINT('Ctrl Pts',(-1.25141455570299,1.,-1.42378102115911));
#35114=CARTESIAN_POINT('Ctrl Pts',(-1.24824430986911,1.,-1.41923722596421));
#35115=CARTESIAN_POINT('Ctrl Pts',(-1.24450600513278,1.,-1.41422913175437));
#35116=CARTESIAN_POINT('Ctrl Pts',(-1.23994455029421,1.,-1.40845295531151));
#35117=CARTESIAN_POINT('Ctrl Pts',(-1.23434087289768,1.,-1.40164708205345));
#35118=CARTESIAN_POINT('Ctrl Pts',(-1.22752961898063,1.,-1.39361389567257));
#35119=CARTESIAN_POINT('Ctrl Pts',(-1.21938737278853,1.,-1.38420564525391));
#35120=CARTESIAN_POINT('Ctrl Pts',(-1.20982812923113,1.,-1.37331915604962));
#35121=CARTESIAN_POINT('Ctrl Pts',(-1.1987959077656,1.,-1.36088705040677));
#35122=CARTESIAN_POINT('Ctrl Pts',(-1.18625865664915,1.,-1.34687053998157));
#35123=CARTESIAN_POINT('Ctrl Pts',(-1.17501305787994,1.,-1.33437539344842));
#35124=CARTESIAN_POINT('Ctrl Pts',(-1.16589330092532,1.,-1.32428080720544));
#35125=CARTESIAN_POINT('Ctrl Pts',(-1.15950888730433,1.,-1.3172297721596));
#35126=CARTESIAN_POINT('Ctrl Pts',(-1.15624053661742,1.,-1.31362392696033));
#35127=CARTESIAN_POINT('',(-1.34869019493419,0.,-1.73811241238545));
#35128=CARTESIAN_POINT('Origin',(-1.23627494547115,0.,-1.81978687191668));
#35129=CARTESIAN_POINT('',(-1.23627494547115,1.,-1.81978687191668));
#35130=CARTESIAN_POINT('',(-1.34869019493419,1.,-1.73811241238545));
#35131=CARTESIAN_POINT('',(-1.23627494547115,0.,-1.81978687191668));
#35132=CARTESIAN_POINT('Ctrl Pts',(-0.892032620296855,-1.,-1.5055822144029));
#35133=CARTESIAN_POINT('Ctrl Pts',(-0.892032620296855,1.,-1.5055822144029));
#35134=CARTESIAN_POINT('Ctrl Pts',(-0.894452006967538,-1.,-1.50980486807181));
#35135=CARTESIAN_POINT('Ctrl Pts',(-0.894452006967538,1.,-1.50980486807181));
#35136=CARTESIAN_POINT('Ctrl Pts',(-0.89918504749193,-1.,-1.51805569591479));
#35137=CARTESIAN_POINT('Ctrl Pts',(-0.89918504749193,1.,-1.51805569591479));
#35138=CARTESIAN_POINT('Ctrl Pts',(-0.905967409640499,-1.,-1.52984849890434));
#35139=CARTESIAN_POINT('Ctrl Pts',(-0.905967409640499,1.,-1.52984849890434));
#35140=CARTESIAN_POINT('Ctrl Pts',(-0.91437591904658,-1.,-1.54440491152808));
#35141=CARTESIAN_POINT('Ctrl Pts',(-0.91437591904658,1.,-1.54440491152808));
#35142=CARTESIAN_POINT('Ctrl Pts',(-0.923832188966322,-1.,-1.56065988582509));
#35143=CARTESIAN_POINT('Ctrl Pts',(-0.923832188966322,1.,-1.56065988582509));
#35144=CARTESIAN_POINT('Ctrl Pts',(-0.932246680128849,-1.,-1.57499388385561));
#35145=CARTESIAN_POINT('Ctrl Pts',(-0.932246680128849,1.,-1.57499388385561));
#35146=CARTESIAN_POINT('Ctrl Pts',(-0.939646377909319,-1.,-1.58744937489796));
#35147=CARTESIAN_POINT('Ctrl Pts',(-0.939646377909319,1.,-1.58744937489796));
#35148=CARTESIAN_POINT('Ctrl Pts',(-0.946078063325796,-1.,-1.59810042045408));
#35149=CARTESIAN_POINT('Ctrl Pts',(-0.946078063325796,1.,-1.59810042045408));
#35150=CARTESIAN_POINT('Ctrl Pts',(-0.951613284361248,-1.,-1.60706069897794));
#35151=CARTESIAN_POINT('Ctrl Pts',(-0.951613284361248,1.,-1.60706069897794));
#35152=CARTESIAN_POINT('Ctrl Pts',(-0.956354422921573,-1.,-1.61449324337233));
#35153=CARTESIAN_POINT('Ctrl Pts',(-0.956354422921573,1.,-1.61449324337233));
#35154=CARTESIAN_POINT('Ctrl Pts',(-0.960438326099958,-1.,-1.62061638139929));
#35155=CARTESIAN_POINT('Ctrl Pts',(-0.960438326099958,1.,-1.62061638139929));
#35156=CARTESIAN_POINT('Ctrl Pts',(-0.964046107037821,-1.,-1.6257193066974));
#35157=CARTESIAN_POINT('Ctrl Pts',(-0.964046107037821,1.,-1.6257193066974));
#35158=CARTESIAN_POINT('Ctrl Pts',(-0.967387853228041,-1.,-1.63013849959083));
#35159=CARTESIAN_POINT('Ctrl Pts',(-0.967387853228041,1.,-1.63013849959083));
#35160=CARTESIAN_POINT('Ctrl Pts',(-0.970669715996356,-1.,-1.63420665729609));
#35161=CARTESIAN_POINT('Ctrl Pts',(-0.970669715996356,1.,-1.63420665729609));
#35162=CARTESIAN_POINT('Ctrl Pts',(-0.974066058287501,-1.,-1.63820952658157));
#35163=CARTESIAN_POINT('Ctrl Pts',(-0.974066058287501,1.,-1.63820952658157));
#35164=CARTESIAN_POINT('Ctrl Pts',(-0.977689794120297,-1.,-1.64233990826831));
#35165=CARTESIAN_POINT('Ctrl Pts',(-0.977689794120297,1.,-1.64233990826831));
#35166=CARTESIAN_POINT('Ctrl Pts',(-0.981562530940574,-1.,-1.64665139190834));
#35167=CARTESIAN_POINT('Ctrl Pts',(-0.981562530940574,1.,-1.64665139190834));
#35168=CARTESIAN_POINT('Ctrl Pts',(-0.985642622921626,-1.,-1.6511001661277));
#35169=CARTESIAN_POINT('Ctrl Pts',(-0.985642622921626,1.,-1.6511001661277));
#35170=CARTESIAN_POINT('Ctrl Pts',(-0.98985562785445,-1.,-1.65559044289746));
#35171=CARTESIAN_POINT('Ctrl Pts',(-0.98985562785445,1.,-1.65559044289746));
#35172=CARTESIAN_POINT('Ctrl Pts',(-0.994121836661116,-1.,-1.66001553809916));
#35173=CARTESIAN_POINT('Ctrl Pts',(-0.994121836661116,1.,-1.66001553809916));
#35174=CARTESIAN_POINT('Ctrl Pts',(-0.998389654952317,-1.,-1.66430758030304));
#35175=CARTESIAN_POINT('Ctrl Pts',(-0.998389654952317,1.,-1.66430758030304));
#35176=CARTESIAN_POINT('Ctrl Pts',(-1.00265091003682,-1.,-1.66846059277231));
#35177=CARTESIAN_POINT('Ctrl Pts',(-1.00265091003682,1.,-1.66846059277231));
#35178=CARTESIAN_POINT('Ctrl Pts',(-1.00692206696387,-1.,-1.67250335383248));
#35179=CARTESIAN_POINT('Ctrl Pts',(-1.00692206696387,1.,-1.67250335383248));
#35180=CARTESIAN_POINT('Ctrl Pts',(-1.01123236493507,-1.,-1.67648246776457));
#35181=CARTESIAN_POINT('Ctrl Pts',(-1.01123236493507,1.,-1.67648246776457));
#35182=CARTESIAN_POINT('Ctrl Pts',(-1.01561026162787,-1.,-1.6804428989482));
#35183=CARTESIAN_POINT('Ctrl Pts',(-1.01561026162787,1.,-1.6804428989482));
#35184=CARTESIAN_POINT('Ctrl Pts',(-1.02006795074222,-1.,-1.68440578021739));
#35185=CARTESIAN_POINT('Ctrl Pts',(-1.02006795074222,1.,-1.68440578021739));
#35186=CARTESIAN_POINT('Ctrl Pts',(-1.02460180535272,-1.,-1.68836910178475));
#35187=CARTESIAN_POINT('Ctrl Pts',(-1.02460180535272,1.,-1.68836910178475));
#35188=CARTESIAN_POINT('Ctrl Pts',(-1.02919977579155,-1.,-1.69231840863471));
#35189=CARTESIAN_POINT('Ctrl Pts',(-1.02919977579155,1.,-1.69231840863471));
#35190=CARTESIAN_POINT('Ctrl Pts',(-1.03384646003587,-1.,-1.69623414782769));
#35191=CARTESIAN_POINT('Ctrl Pts',(-1.03384646003587,1.,-1.69623414782769));
#35192=CARTESIAN_POINT('Ctrl Pts',(-1.03852922490782,-1.,-1.70010052930951));
#35193=CARTESIAN_POINT('Ctrl Pts',(-1.03852922490782,1.,-1.70010052930951));
#35194=CARTESIAN_POINT('Ctrl Pts',(-1.04324363334546,-1.,-1.70391338707969));
#35195=CARTESIAN_POINT('Ctrl Pts',(-1.04324363334546,1.,-1.70391338707969));
#35196=CARTESIAN_POINT('Ctrl Pts',(-1.0479908540499,-1.,-1.70767646263641));
#35197=CARTESIAN_POINT('Ctrl Pts',(-1.0479908540499,1.,-1.70767646263641));
#35198=CARTESIAN_POINT('Ctrl Pts',(-1.05277517202854,-1.,-1.71139783543986));
#35199=CARTESIAN_POINT('Ctrl Pts',(-1.05277517202854,1.,-1.71139783543986));
#35200=CARTESIAN_POINT('Ctrl Pts',(-1.05760163192481,-1.,-1.71508654427022));
#35201=CARTESIAN_POINT('Ctrl Pts',(-1.05760163192481,1.,-1.71508654427022));
#35202=CARTESIAN_POINT('Ctrl Pts',(-1.0624732468065,-1.,-1.71874858456908));
#35203=CARTESIAN_POINT('Ctrl Pts',(-1.0624732468065,1.,-1.71874858456908));
#35204=CARTESIAN_POINT('Ctrl Pts',(-1.06738966975463,-1.,-1.72238500928456));
#35205=CARTESIAN_POINT('Ctrl Pts',(-1.06738966975463,1.,-1.72238500928456));
#35206=CARTESIAN_POINT('Ctrl Pts',(-1.07234866990252,-1.,-1.72599406198489));
#35207=CARTESIAN_POINT('Ctrl Pts',(-1.07234866990252,1.,-1.72599406198489));
#35208=CARTESIAN_POINT('Ctrl Pts',(-1.0773470373727,-1.,-1.72957248977424));
#35209=CARTESIAN_POINT('Ctrl Pts',(-1.0773470373727,1.,-1.72957248977424));
#35210=CARTESIAN_POINT('Ctrl Pts',(-1.08238162784749,-1.,-1.73311705663407));
#35211=CARTESIAN_POINT('Ctrl Pts',(-1.08238162784749,1.,-1.73311705663407));
#35212=CARTESIAN_POINT('Ctrl Pts',(-1.08745056285429,-1.,-1.73662628326093));
#35213=CARTESIAN_POINT('Ctrl Pts',(-1.08745056285429,1.,-1.73662628326093));
#35214=CARTESIAN_POINT('Ctrl Pts',(-1.09255329056496,-1.,-1.74010053962252));
#35215=CARTESIAN_POINT('Ctrl Pts',(-1.09255329056496,1.,-1.74010053962252));
#35216=CARTESIAN_POINT('Ctrl Pts',(-1.09768999241229,-1.,-1.74354119236212));
#35217=CARTESIAN_POINT('Ctrl Pts',(-1.09768999241229,1.,-1.74354119236212));
#35218=CARTESIAN_POINT('Ctrl Pts',(-1.10286118991144,-1.,-1.74695004214924));
#35219=CARTESIAN_POINT('Ctrl Pts',(-1.10286118991144,1.,-1.74695004214924));
#35220=CARTESIAN_POINT('Ctrl Pts',(-1.10806728183003,-1.,-1.75032866075914));
#35221=CARTESIAN_POINT('Ctrl Pts',(-1.10806728183003,1.,-1.75032866075914));
#35222=CARTESIAN_POINT('Ctrl Pts',(-1.11330807582542,-1.,-1.75367772094617));
#35223=CARTESIAN_POINT('Ctrl Pts',(-1.11330807582542,1.,-1.75367772094617));
#35224=CARTESIAN_POINT('Ctrl Pts',(-1.11858293216752,-1.,-1.75699720772089));
#35225=CARTESIAN_POINT('Ctrl Pts',(-1.11858293216752,1.,-1.75699720772089));
#35226=CARTESIAN_POINT('Ctrl Pts',(-1.12389096855078,-1.,-1.76028671825084));
#35227=CARTESIAN_POINT('Ctrl Pts',(-1.12389096855078,1.,-1.76028671825084));
#35228=CARTESIAN_POINT('Ctrl Pts',(-1.12923123555076,-1.,-1.76354571966171));
#35229=CARTESIAN_POINT('Ctrl Pts',(-1.12923123555076,1.,-1.76354571966171));
#35230=CARTESIAN_POINT('Ctrl Pts',(-1.13460291804635,-1.,-1.76677384551883));
#35231=CARTESIAN_POINT('Ctrl Pts',(-1.13460291804635,1.,-1.76677384551883));
#35232=CARTESIAN_POINT('Ctrl Pts',(-1.14000548337,-1.,-1.76997111386806));
#35233=CARTESIAN_POINT('Ctrl Pts',(-1.14000548337,1.,-1.76997111386806));
#35234=CARTESIAN_POINT('Ctrl Pts',(-1.14543858226948,-1.,-1.77313777896234));
#35235=CARTESIAN_POINT('Ctrl Pts',(-1.14543858226948,1.,-1.77313777896234));
#35236=CARTESIAN_POINT('Ctrl Pts',(-1.15090197841531,-1.,-1.77627422557034));
#35237=CARTESIAN_POINT('Ctrl Pts',(-1.15090197841531,1.,-1.77627422557034));
#35238=CARTESIAN_POINT('Ctrl Pts',(-1.15639547194689,-1.,-1.77938085564261));
#35239=CARTESIAN_POINT('Ctrl Pts',(-1.15639547194689,1.,-1.77938085564261));
#35240=CARTESIAN_POINT('Ctrl Pts',(-1.16191881298458,-1.,-1.78245795880949));
#35241=CARTESIAN_POINT('Ctrl Pts',(-1.16191881298458,1.,-1.78245795880949));
#35242=CARTESIAN_POINT('Ctrl Pts',(-1.16747166312239,-1.,-1.78550566040349));
#35243=CARTESIAN_POINT('Ctrl Pts',(-1.16747166312239,1.,-1.78550566040349));
#35244=CARTESIAN_POINT('Ctrl Pts',(-1.17305363177265,-1.,-1.78852398877523));
#35245=CARTESIAN_POINT('Ctrl Pts',(-1.17305363177265,1.,-1.78852398877523));
#35246=CARTESIAN_POINT('Ctrl Pts',(-1.17866429440781,-1.,-1.79151291552646));
#35247=CARTESIAN_POINT('Ctrl Pts',(-1.17866429440781,1.,-1.79151291552646));
#35248=CARTESIAN_POINT('Ctrl Pts',(-1.18430321697471,-1.,-1.79447240321572));
#35249=CARTESIAN_POINT('Ctrl Pts',(-1.18430321697471,1.,-1.79447240321572));
#35250=CARTESIAN_POINT('Ctrl Pts',(-1.1899699793456,-1.,-1.79740245923649));
#35251=CARTESIAN_POINT('Ctrl Pts',(-1.1899699793456,1.,-1.79740245923649));
#35252=CARTESIAN_POINT('Ctrl Pts',(-1.19566418930405,-1.,-1.80030314370121));
#35253=CARTESIAN_POINT('Ctrl Pts',(-1.19566418930405,1.,-1.80030314370121));
#35254=CARTESIAN_POINT('Ctrl Pts',(-1.2013854893912,-1.,-1.8031745483882));
#35255=CARTESIAN_POINT('Ctrl Pts',(-1.2013854893912,1.,-1.8031745483882));
#35256=CARTESIAN_POINT('Ctrl Pts',(-1.20713356605519,-1.,-1.80601678480772));
#35257=CARTESIAN_POINT('Ctrl Pts',(-1.20713356605519,1.,-1.80601678480772));
#35258=CARTESIAN_POINT('Ctrl Pts',(-1.2129081570818,-1.,-1.80882996916931));
#35259=CARTESIAN_POINT('Ctrl Pts',(-1.2129081570818,1.,-1.80882996916931));
#35260=CARTESIAN_POINT('Ctrl Pts',(-1.2187090610323,-1.,-1.81161420806172));
#35261=CARTESIAN_POINT('Ctrl Pts',(-1.2187090610323,1.,-1.81161420806172));
#35262=CARTESIAN_POINT('Ctrl Pts',(-1.22453613304507,-1.,-1.81436959209778));
#35263=CARTESIAN_POINT('Ctrl Pts',(-1.22453613304507,1.,-1.81436959209778));
#35264=CARTESIAN_POINT('Ctrl Pts',(-1.22921864890975,-1.,-1.81655087183054));
#35265=CARTESIAN_POINT('Ctrl Pts',(-1.22921864890975,1.,-1.81655087183054));
#35266=CARTESIAN_POINT('Ctrl Pts',(-1.23274224526804,-1.,-1.81817389920914));
#35267=CARTESIAN_POINT('Ctrl Pts',(-1.23274224526804,1.,-1.81817389920914));
#35268=CARTESIAN_POINT('Ctrl Pts',(-1.23509651170384,-1.,-1.81925017193531));
#35269=CARTESIAN_POINT('Ctrl Pts',(-1.23509651170384,1.,-1.81925017193531));
#35270=CARTESIAN_POINT('Ctrl Pts',(-1.23627494547115,-1.,-1.81978687191668));
#35271=CARTESIAN_POINT('Ctrl Pts',(-1.23627494547115,1.,-1.81978687191668));
#35272=CARTESIAN_POINT('',(-0.892032620296855,1.,-1.5055822144029));
#35273=CARTESIAN_POINT('Ctrl Pts',(-0.892032620296855,1.,-1.5055822144029));
#35274=CARTESIAN_POINT('Ctrl Pts',(-0.894452006967538,1.,-1.50980486807181));
#35275=CARTESIAN_POINT('Ctrl Pts',(-0.89918504749193,1.,-1.51805569591479));
#35276=CARTESIAN_POINT('Ctrl Pts',(-0.905967409640499,1.,-1.52984849890434));
#35277=CARTESIAN_POINT('Ctrl Pts',(-0.91437591904658,1.,-1.54440491152808));
#35278=CARTESIAN_POINT('Ctrl Pts',(-0.923832188966322,1.,-1.56065988582509));
#35279=CARTESIAN_POINT('Ctrl Pts',(-0.932246680128849,1.,-1.57499388385561));
#35280=CARTESIAN_POINT('Ctrl Pts',(-0.939646377909319,1.,-1.58744937489796));
#35281=CARTESIAN_POINT('Ctrl Pts',(-0.946078063325796,1.,-1.59810042045408));
#35282=CARTESIAN_POINT('Ctrl Pts',(-0.951613284361248,1.,-1.60706069897794));
#35283=CARTESIAN_POINT('Ctrl Pts',(-0.956354422921573,1.,-1.61449324337233));
#35284=CARTESIAN_POINT('Ctrl Pts',(-0.960438326099958,1.,-1.62061638139929));
#35285=CARTESIAN_POINT('Ctrl Pts',(-0.964046107037821,1.,-1.6257193066974));
#35286=CARTESIAN_POINT('Ctrl Pts',(-0.967387853228041,1.,-1.63013849959083));
#35287=CARTESIAN_POINT('Ctrl Pts',(-0.970669715996356,1.,-1.63420665729609));
#35288=CARTESIAN_POINT('Ctrl Pts',(-0.974066058287501,1.,-1.63820952658157));
#35289=CARTESIAN_POINT('Ctrl Pts',(-0.977689794120297,1.,-1.64233990826831));
#35290=CARTESIAN_POINT('Ctrl Pts',(-0.981562530940574,1.,-1.64665139190834));
#35291=CARTESIAN_POINT('Ctrl Pts',(-0.985642622921626,1.,-1.6511001661277));
#35292=CARTESIAN_POINT('Ctrl Pts',(-0.98985562785445,1.,-1.65559044289746));
#35293=CARTESIAN_POINT('Ctrl Pts',(-0.994121836661116,1.,-1.66001553809916));
#35294=CARTESIAN_POINT('Ctrl Pts',(-0.998389654952317,1.,-1.66430758030304));
#35295=CARTESIAN_POINT('Ctrl Pts',(-1.00265091003682,1.,-1.66846059277231));
#35296=CARTESIAN_POINT('Ctrl Pts',(-1.00692206696387,1.,-1.67250335383248));
#35297=CARTESIAN_POINT('Ctrl Pts',(-1.01123236493507,1.,-1.67648246776457));
#35298=CARTESIAN_POINT('Ctrl Pts',(-1.01561026162787,1.,-1.6804428989482));
#35299=CARTESIAN_POINT('Ctrl Pts',(-1.02006795074222,1.,-1.68440578021739));
#35300=CARTESIAN_POINT('Ctrl Pts',(-1.02460180535272,1.,-1.68836910178475));
#35301=CARTESIAN_POINT('Ctrl Pts',(-1.02919977579155,1.,-1.69231840863471));
#35302=CARTESIAN_POINT('Ctrl Pts',(-1.03384646003587,1.,-1.69623414782769));
#35303=CARTESIAN_POINT('Ctrl Pts',(-1.03852922490782,1.,-1.70010052930951));
#35304=CARTESIAN_POINT('Ctrl Pts',(-1.04324363334546,1.,-1.70391338707969));
#35305=CARTESIAN_POINT('Ctrl Pts',(-1.0479908540499,1.,-1.70767646263641));
#35306=CARTESIAN_POINT('Ctrl Pts',(-1.05277517202854,1.,-1.71139783543986));
#35307=CARTESIAN_POINT('Ctrl Pts',(-1.05760163192481,1.,-1.71508654427022));
#35308=CARTESIAN_POINT('Ctrl Pts',(-1.0624732468065,1.,-1.71874858456908));
#35309=CARTESIAN_POINT('Ctrl Pts',(-1.06738966975463,1.,-1.72238500928456));
#35310=CARTESIAN_POINT('Ctrl Pts',(-1.07234866990252,1.,-1.72599406198489));
#35311=CARTESIAN_POINT('Ctrl Pts',(-1.0773470373727,1.,-1.72957248977424));
#35312=CARTESIAN_POINT('Ctrl Pts',(-1.08238162784749,1.,-1.73311705663407));
#35313=CARTESIAN_POINT('Ctrl Pts',(-1.08745056285429,1.,-1.73662628326093));
#35314=CARTESIAN_POINT('Ctrl Pts',(-1.09255329056496,1.,-1.74010053962252));
#35315=CARTESIAN_POINT('Ctrl Pts',(-1.09768999241229,1.,-1.74354119236212));
#35316=CARTESIAN_POINT('Ctrl Pts',(-1.10286118991144,1.,-1.74695004214924));
#35317=CARTESIAN_POINT('Ctrl Pts',(-1.10806728183003,1.,-1.75032866075914));
#35318=CARTESIAN_POINT('Ctrl Pts',(-1.11330807582542,1.,-1.75367772094617));
#35319=CARTESIAN_POINT('Ctrl Pts',(-1.11858293216752,1.,-1.75699720772089));
#35320=CARTESIAN_POINT('Ctrl Pts',(-1.12389096855078,1.,-1.76028671825084));
#35321=CARTESIAN_POINT('Ctrl Pts',(-1.12923123555076,1.,-1.76354571966171));
#35322=CARTESIAN_POINT('Ctrl Pts',(-1.13460291804635,1.,-1.76677384551883));
#35323=CARTESIAN_POINT('Ctrl Pts',(-1.14000548337,1.,-1.76997111386806));
#35324=CARTESIAN_POINT('Ctrl Pts',(-1.14543858226948,1.,-1.77313777896234));
#35325=CARTESIAN_POINT('Ctrl Pts',(-1.15090197841531,1.,-1.77627422557034));
#35326=CARTESIAN_POINT('Ctrl Pts',(-1.15639547194689,1.,-1.77938085564261));
#35327=CARTESIAN_POINT('Ctrl Pts',(-1.16191881298458,1.,-1.78245795880949));
#35328=CARTESIAN_POINT('Ctrl Pts',(-1.16747166312239,1.,-1.78550566040349));
#35329=CARTESIAN_POINT('Ctrl Pts',(-1.17305363177265,1.,-1.78852398877523));
#35330=CARTESIAN_POINT('Ctrl Pts',(-1.17866429440781,1.,-1.79151291552646));
#35331=CARTESIAN_POINT('Ctrl Pts',(-1.18430321697471,1.,-1.79447240321572));
#35332=CARTESIAN_POINT('Ctrl Pts',(-1.1899699793456,1.,-1.79740245923649));
#35333=CARTESIAN_POINT('Ctrl Pts',(-1.19566418930405,1.,-1.80030314370121));
#35334=CARTESIAN_POINT('Ctrl Pts',(-1.2013854893912,1.,-1.8031745483882));
#35335=CARTESIAN_POINT('Ctrl Pts',(-1.20713356605519,1.,-1.80601678480772));
#35336=CARTESIAN_POINT('Ctrl Pts',(-1.2129081570818,1.,-1.80882996916931));
#35337=CARTESIAN_POINT('Ctrl Pts',(-1.2187090610323,1.,-1.81161420806172));
#35338=CARTESIAN_POINT('Ctrl Pts',(-1.22453613304507,1.,-1.81436959209778));
#35339=CARTESIAN_POINT('Ctrl Pts',(-1.22921864890975,1.,-1.81655087183054));
#35340=CARTESIAN_POINT('Ctrl Pts',(-1.23274224526804,1.,-1.81817389920914));
#35341=CARTESIAN_POINT('Ctrl Pts',(-1.23509651170384,1.,-1.81925017193531));
#35342=CARTESIAN_POINT('Ctrl Pts',(-1.23627494547115,1.,-1.81978687191668));
#35343=CARTESIAN_POINT('',(-0.892032620296856,0.,-1.5055822144029));
#35344=CARTESIAN_POINT('Origin',(0.,0.,0.));
#35345=CARTESIAN_POINT('',(-0.693717979106305,1.,-1.60662857109684));
#35346=CARTESIAN_POINT('Origin',(0.,1.,0.));
#35347=CARTESIAN_POINT('',(-0.693717979106306,0.,-1.60662857109684));
#35348=CARTESIAN_POINT('Ctrl Pts',(-0.745574324794401,-1.,-2.0698113262342));
#35349=CARTESIAN_POINT('Ctrl Pts',(-0.745574324794401,1.,-2.0698113262342));
#35350=CARTESIAN_POINT('Ctrl Pts',(-0.745832791378367,-1.,-2.06854248895728));
#35351=CARTESIAN_POINT('Ctrl Pts',(-0.745832791378367,1.,-2.06854248895728));
#35352=CARTESIAN_POINT('Ctrl Pts',(-0.7463458715442,-1.,-2.06600523016815));
#35353=CARTESIAN_POINT('Ctrl Pts',(-0.7463458715442,1.,-2.06600523016815));
#35354=CARTESIAN_POINT('Ctrl Pts',(-0.747103932787919,-1.,-2.06220058927826));
#35355=CARTESIAN_POINT('Ctrl Pts',(-0.747103932787919,1.,-2.06220058927826));
#35356=CARTESIAN_POINT('Ctrl Pts',(-0.748091554183802,-1.,-2.05713023031006));
#35357=CARTESIAN_POINT('Ctrl Pts',(-0.748091554183802,1.,-2.05713023031006));
#35358=CARTESIAN_POINT('Ctrl Pts',(-0.749287468665046,-1.,-2.05079645592154));
#35359=CARTESIAN_POINT('Ctrl Pts',(-0.749287468665046,1.,-2.05079645592154));
#35360=CARTESIAN_POINT('Ctrl Pts',(-0.750444657875576,-1.,-2.04446689147979));
#35361=CARTESIAN_POINT('Ctrl Pts',(-0.750444657875576,1.,-2.04446689147979));
#35362=CARTESIAN_POINT('Ctrl Pts',(-0.751562963361115,-1.,-2.03814160092099));
#35363=CARTESIAN_POINT('Ctrl Pts',(-0.751562963361115,1.,-2.03814160092099));
#35364=CARTESIAN_POINT('Ctrl Pts',(-0.752642180487211,-1.,-2.03182068456221));
#35365=CARTESIAN_POINT('Ctrl Pts',(-0.752642180487211,1.,-2.03182068456221));
#35366=CARTESIAN_POINT('Ctrl Pts',(-0.753682061112768,-1.,-2.02550428623313));
#35367=CARTESIAN_POINT('Ctrl Pts',(-0.753682061112768,1.,-2.02550428623313));
#35368=CARTESIAN_POINT('Ctrl Pts',(-0.754682330722816,-1.,-2.01919259405809));
#35369=CARTESIAN_POINT('Ctrl Pts',(-0.754682330722816,1.,-2.01919259405809));
#35370=CARTESIAN_POINT('Ctrl Pts',(-0.755642704957865,-1.,-2.01288584328084));
#35371=CARTESIAN_POINT('Ctrl Pts',(-0.755642704957865,1.,-2.01288584328084));
#35372=CARTESIAN_POINT('Ctrl Pts',(-0.75656290464667,-1.,-2.0065843158773));
#35373=CARTESIAN_POINT('Ctrl Pts',(-0.75656290464667,1.,-2.0065843158773));
#35374=CARTESIAN_POINT('Ctrl Pts',(-0.757442676862724,-1.,-2.00028834739178));
#35375=CARTESIAN_POINT('Ctrl Pts',(-0.757442676862724,1.,-2.00028834739178));
#35376=CARTESIAN_POINT('Ctrl Pts',(-0.758281796766761,-1.,-1.99399831098817));
#35377=CARTESIAN_POINT('Ctrl Pts',(-0.758281796766761,1.,-1.99399831098817));
#35378=CARTESIAN_POINT('Ctrl Pts',(-0.759080037802488,-1.,-1.98771456680874));
#35379=CARTESIAN_POINT('Ctrl Pts',(-0.759080037802488,1.,-1.98771456680874));
#35380=CARTESIAN_POINT('Ctrl Pts',(-0.75983714745219,-1.,-1.98143741418172));
#35381=CARTESIAN_POINT('Ctrl Pts',(-0.75983714745219,1.,-1.98143741418172));
#35382=CARTESIAN_POINT('Ctrl Pts',(-0.760552825409757,-1.,-1.97516705321494));
#35383=CARTESIAN_POINT('Ctrl Pts',(-0.760552825409757,1.,-1.97516705321494));
#35384=CARTESIAN_POINT('Ctrl Pts',(-0.76122669048382,-1.,-1.96890351582499));
#35385=CARTESIAN_POINT('Ctrl Pts',(-0.76122669048382,1.,-1.96890351582499));
#35386=CARTESIAN_POINT('Ctrl Pts',(-0.761858300014423,-1.,-1.96264672744186));
#35387=CARTESIAN_POINT('Ctrl Pts',(-0.761858300014423,1.,-1.96264672744186));
#35388=CARTESIAN_POINT('Ctrl Pts',(-0.762447203806179,-1.,-1.95639665309869));
#35389=CARTESIAN_POINT('Ctrl Pts',(-0.762447203806179,1.,-1.95639665309869));
#35390=CARTESIAN_POINT('Ctrl Pts',(-0.762992990878769,-1.,-1.95015342590024));
#35391=CARTESIAN_POINT('Ctrl Pts',(-0.762992990878769,1.,-1.95015342590024));
#35392=CARTESIAN_POINT('Ctrl Pts',(-0.763495333538629,-1.,-1.9439174661764));
#35393=CARTESIAN_POINT('Ctrl Pts',(-0.763495333538629,1.,-1.9439174661764));
#35394=CARTESIAN_POINT('Ctrl Pts',(-0.763954049121458,-1.,-1.93768964875886));
#35395=CARTESIAN_POINT('Ctrl Pts',(-0.763954049121458,1.,-1.93768964875886));
#35396=CARTESIAN_POINT('Ctrl Pts',(-0.764369010673941,-1.,-1.93147105496382));
#35397=CARTESIAN_POINT('Ctrl Pts',(-0.764369010673941,1.,-1.93147105496382));
#35398=CARTESIAN_POINT('Ctrl Pts',(-0.764740025488211,-1.,-1.92526263537048));
#35399=CARTESIAN_POINT('Ctrl Pts',(-0.764740025488211,1.,-1.92526263537048));
#35400=CARTESIAN_POINT('Ctrl Pts',(-0.765066729667088,-1.,-1.91906491634196));
#35401=CARTESIAN_POINT('Ctrl Pts',(-0.765066729667088,1.,-1.91906491634196));
#35402=CARTESIAN_POINT('Ctrl Pts',(-0.765348465884722,-1.,-1.91287765805169));
#35403=CARTESIAN_POINT('Ctrl Pts',(-0.765348465884722,1.,-1.91287765805169));
#35404=CARTESIAN_POINT('Ctrl Pts',(-0.765584196937919,-1.,-1.90669961402356));
#35405=CARTESIAN_POINT('Ctrl Pts',(-0.765584196937919,1.,-1.90669961402356));
#35406=CARTESIAN_POINT('Ctrl Pts',(-0.765772772593386,-1.,-1.90052930393596));
#35407=CARTESIAN_POINT('Ctrl Pts',(-0.765772772593386,1.,-1.90052930393596));
#35408=CARTESIAN_POINT('Ctrl Pts',(-0.765913193856978,-1.,-1.89436577771388));
#35409=CARTESIAN_POINT('Ctrl Pts',(-0.765913193856978,1.,-1.89436577771388));
#35410=CARTESIAN_POINT('Ctrl Pts',(-0.766004837062091,-1.,-1.88820926433409));
#35411=CARTESIAN_POINT('Ctrl Pts',(-0.766004837062091,1.,-1.88820926433409));
#35412=CARTESIAN_POINT('Ctrl Pts',(-0.766047794851865,-1.,-1.88206215302561));
#35413=CARTESIAN_POINT('Ctrl Pts',(-0.766047794851865,1.,-1.88206215302561));
#35414=CARTESIAN_POINT('Ctrl Pts',(-0.766042837036744,-1.,-1.87592888967883));
#35415=CARTESIAN_POINT('Ctrl Pts',(-0.766042837036744,1.,-1.87592888967883));
#35416=CARTESIAN_POINT('Ctrl Pts',(-0.765990708546091,-1.,-1.86981398314341));
#35417=CARTESIAN_POINT('Ctrl Pts',(-0.765990708546091,1.,-1.86981398314341));
#35418=CARTESIAN_POINT('Ctrl Pts',(-0.765891519092547,-1.,-1.86372027063312));
#35419=CARTESIAN_POINT('Ctrl Pts',(-0.765891519092547,1.,-1.86372027063312));
#35420=CARTESIAN_POINT('Ctrl Pts',(-0.765744212909318,-1.,-1.85764741390394));
#35421=CARTESIAN_POINT('Ctrl Pts',(-0.765744212909318,1.,-1.85764741390394));
#35422=CARTESIAN_POINT('Ctrl Pts',(-0.765545710619062,-1.,-1.85158945130063));
#35423=CARTESIAN_POINT('Ctrl Pts',(-0.765545710619062,1.,-1.85158945130063));
#35424=CARTESIAN_POINT('Ctrl Pts',(-0.765291664862029,-1.,-1.84553698875924));
#35425=CARTESIAN_POINT('Ctrl Pts',(-0.765291664862029,1.,-1.84553698875924));
#35426=CARTESIAN_POINT('Ctrl Pts',(-0.764978057881737,-1.,-1.83948181064835));
#35427=CARTESIAN_POINT('Ctrl Pts',(-0.764978057881737,1.,-1.83948181064835));
#35428=CARTESIAN_POINT('Ctrl Pts',(-0.764602549687853,-1.,-1.83342077227142));
#35429=CARTESIAN_POINT('Ctrl Pts',(-0.764602549687853,1.,-1.83342077227142));
#35430=CARTESIAN_POINT('Ctrl Pts',(-0.764165902605995,-1.,-1.82735991200065));
#35431=CARTESIAN_POINT('Ctrl Pts',(-0.764165902605995,1.,-1.82735991200065));
#35432=CARTESIAN_POINT('Ctrl Pts',(-0.763673465462726,-1.,-1.82131873145266));
#35433=CARTESIAN_POINT('Ctrl Pts',(-0.763673465462726,1.,-1.82131873145266));
#35434=CARTESIAN_POINT('Ctrl Pts',(-0.763132003836634,-1.,-1.8153211840553));
#35435=CARTESIAN_POINT('Ctrl Pts',(-0.763132003836634,1.,-1.8153211840553));
#35436=CARTESIAN_POINT('Ctrl Pts',(-0.762546129463938,-1.,-1.80938551463965));
#35437=CARTESIAN_POINT('Ctrl Pts',(-0.762546129463938,1.,-1.80938551463965));
#35438=CARTESIAN_POINT('Ctrl Pts',(-0.761915336443547,-1.,-1.80351583877342));
#35439=CARTESIAN_POINT('Ctrl Pts',(-0.761915336443547,1.,-1.80351583877342));
#35440=CARTESIAN_POINT('Ctrl Pts',(-0.761229695230558,-1.,-1.79768986997783));
#35441=CARTESIAN_POINT('Ctrl Pts',(-0.761229695230558,1.,-1.79768986997783));
#35442=CARTESIAN_POINT('Ctrl Pts',(-0.760469555880749,-1.,-1.7918581561088));
#35443=CARTESIAN_POINT('Ctrl Pts',(-0.760469555880749,1.,-1.7918581561088));
#35444=CARTESIAN_POINT('Ctrl Pts',(-0.759614401110189,-1.,-1.78596964884604));
#35445=CARTESIAN_POINT('Ctrl Pts',(-0.759614401110189,1.,-1.78596964884604));
#35446=CARTESIAN_POINT('Ctrl Pts',(-0.758650626677518,-1.,-1.77999411220945));
#35447=CARTESIAN_POINT('Ctrl Pts',(-0.758650626677518,1.,-1.77999411220945));
#35448=CARTESIAN_POINT('Ctrl Pts',(-0.757578264077029,-1.,-1.77394167108292));
#35449=CARTESIAN_POINT('Ctrl Pts',(-0.757578264077029,1.,-1.77394167108292));
#35450=CARTESIAN_POINT('Ctrl Pts',(-0.75642189602781,-1.,-1.76789396002998));
#35451=CARTESIAN_POINT('Ctrl Pts',(-0.75642189602781,1.,-1.76789396002998));
#35452=CARTESIAN_POINT('Ctrl Pts',(-0.755220979974461,-1.,-1.76197817240128));
#35453=CARTESIAN_POINT('Ctrl Pts',(-0.755220979974461,1.,-1.76197817240128));
#35454=CARTESIAN_POINT('Ctrl Pts',(-0.754009254027829,-1.,-1.75631083600019));
#35455=CARTESIAN_POINT('Ctrl Pts',(-0.754009254027829,1.,-1.75631083600019));
#35456=CARTESIAN_POINT('Ctrl Pts',(-0.752797683531314,-1.,-1.75095139468794));
#35457=CARTESIAN_POINT('Ctrl Pts',(-0.752797683531314,1.,-1.75095139468794));
#35458=CARTESIAN_POINT('Ctrl Pts',(-0.751555614164482,-1.,-1.74585086852502));
#35459=CARTESIAN_POINT('Ctrl Pts',(-0.751555614164482,1.,-1.74585086852502));
#35460=CARTESIAN_POINT('Ctrl Pts',(-0.750193435981249,-1.,-1.74080458267114));
#35461=CARTESIAN_POINT('Ctrl Pts',(-0.750193435981249,1.,-1.74080458267114));
#35462=CARTESIAN_POINT('Ctrl Pts',(-0.74858246295687,-1.,-1.7355035168033));
#35463=CARTESIAN_POINT('Ctrl Pts',(-0.74858246295687,1.,-1.7355035168033));
#35464=CARTESIAN_POINT('Ctrl Pts',(-0.746574710097752,-1.,-1.72958533647714));
#35465=CARTESIAN_POINT('Ctrl Pts',(-0.746574710097752,1.,-1.72958533647714));
#35466=CARTESIAN_POINT('Ctrl Pts',(-0.744021445433093,-1.,-1.72268229916769));
#35467=CARTESIAN_POINT('Ctrl Pts',(-0.744021445433093,1.,-1.72268229916769));
#35468=CARTESIAN_POINT('Ctrl Pts',(-0.74079516202821,-1.,-1.71447789751001));
#35469=CARTESIAN_POINT('Ctrl Pts',(-0.74079516202821,1.,-1.71447789751001));
#35470=CARTESIAN_POINT('Ctrl Pts',(-0.736799665716932,-1.,-1.70473309004249));
#35471=CARTESIAN_POINT('Ctrl Pts',(-0.736799665716932,1.,-1.70473309004249));
#35472=CARTESIAN_POINT('Ctrl Pts',(-0.731963238685357,-1.,-1.69326921972915));
#35473=CARTESIAN_POINT('Ctrl Pts',(-0.731963238685357,1.,-1.69326921972915));
#35474=CARTESIAN_POINT('Ctrl Pts',(-0.726235967982445,-1.,-1.67996158451922));
#35475=CARTESIAN_POINT('Ctrl Pts',(-0.726235967982445,1.,-1.67996158451922));
#35476=CARTESIAN_POINT('Ctrl Pts',(-0.71958543378795,-1.,-1.66472880551777));
#35477=CARTESIAN_POINT('Ctrl Pts',(-0.71958543378795,1.,-1.66472880551777));
#35478=CARTESIAN_POINT('Ctrl Pts',(-0.711993139340447,-1.,-1.64752408828442));
#35479=CARTESIAN_POINT('Ctrl Pts',(-0.711993139340447,1.,-1.64752408828442));
#35480=CARTESIAN_POINT('Ctrl Pts',(-0.705159151977294,-1.,-1.6321654166204));
#35481=CARTESIAN_POINT('Ctrl Pts',(-0.705159151977294,1.,-1.6321654166204));
#35482=CARTESIAN_POINT('Ctrl Pts',(-0.699605146398837,-1.,-1.61974673471117));
#35483=CARTESIAN_POINT('Ctrl Pts',(-0.699605146398837,1.,-1.61974673471117));
#35484=CARTESIAN_POINT('Ctrl Pts',(-0.69571209787897,-1.,-1.61106790957619));
#35485=CARTESIAN_POINT('Ctrl Pts',(-0.69571209787897,1.,-1.61106790957619));
#35486=CARTESIAN_POINT('Ctrl Pts',(-0.693717979106305,-1.,-1.60662857109684));
#35487=CARTESIAN_POINT('Ctrl Pts',(-0.693717979106305,1.,-1.60662857109684));
#35488=CARTESIAN_POINT('',(-0.745574324794401,1.,-2.0698113262342));
#35489=CARTESIAN_POINT('Ctrl Pts',(-0.745574324794401,1.,-2.0698113262342));
#35490=CARTESIAN_POINT('Ctrl Pts',(-0.745832791378367,1.,-2.06854248895728));
#35491=CARTESIAN_POINT('Ctrl Pts',(-0.7463458715442,1.,-2.06600523016815));
#35492=CARTESIAN_POINT('Ctrl Pts',(-0.747103932787919,1.,-2.06220058927826));
#35493=CARTESIAN_POINT('Ctrl Pts',(-0.748091554183802,1.,-2.05713023031006));
#35494=CARTESIAN_POINT('Ctrl Pts',(-0.749287468665046,1.,-2.05079645592154));
#35495=CARTESIAN_POINT('Ctrl Pts',(-0.750444657875576,1.,-2.04446689147979));
#35496=CARTESIAN_POINT('Ctrl Pts',(-0.751562963361115,1.,-2.03814160092099));
#35497=CARTESIAN_POINT('Ctrl Pts',(-0.752642180487211,1.,-2.03182068456221));
#35498=CARTESIAN_POINT('Ctrl Pts',(-0.753682061112768,1.,-2.02550428623313));
#35499=CARTESIAN_POINT('Ctrl Pts',(-0.754682330722816,1.,-2.01919259405809));
#35500=CARTESIAN_POINT('Ctrl Pts',(-0.755642704957865,1.,-2.01288584328084));
#35501=CARTESIAN_POINT('Ctrl Pts',(-0.75656290464667,1.,-2.0065843158773));
#35502=CARTESIAN_POINT('Ctrl Pts',(-0.757442676862724,1.,-2.00028834739178));
#35503=CARTESIAN_POINT('Ctrl Pts',(-0.758281796766761,1.,-1.99399831098817));
#35504=CARTESIAN_POINT('Ctrl Pts',(-0.759080037802488,1.,-1.98771456680874));
#35505=CARTESIAN_POINT('Ctrl Pts',(-0.75983714745219,1.,-1.98143741418172));
#35506=CARTESIAN_POINT('Ctrl Pts',(-0.760552825409757,1.,-1.97516705321494));
#35507=CARTESIAN_POINT('Ctrl Pts',(-0.76122669048382,1.,-1.96890351582499));
#35508=CARTESIAN_POINT('Ctrl Pts',(-0.761858300014423,1.,-1.96264672744186));
#35509=CARTESIAN_POINT('Ctrl Pts',(-0.762447203806179,1.,-1.95639665309869));
#35510=CARTESIAN_POINT('Ctrl Pts',(-0.762992990878769,1.,-1.95015342590024));
#35511=CARTESIAN_POINT('Ctrl Pts',(-0.763495333538629,1.,-1.9439174661764));
#35512=CARTESIAN_POINT('Ctrl Pts',(-0.763954049121458,1.,-1.93768964875886));
#35513=CARTESIAN_POINT('Ctrl Pts',(-0.764369010673941,1.,-1.93147105496382));
#35514=CARTESIAN_POINT('Ctrl Pts',(-0.764740025488211,1.,-1.92526263537048));
#35515=CARTESIAN_POINT('Ctrl Pts',(-0.765066729667088,1.,-1.91906491634196));
#35516=CARTESIAN_POINT('Ctrl Pts',(-0.765348465884722,1.,-1.91287765805169));
#35517=CARTESIAN_POINT('Ctrl Pts',(-0.765584196937919,1.,-1.90669961402356));
#35518=CARTESIAN_POINT('Ctrl Pts',(-0.765772772593386,1.,-1.90052930393596));
#35519=CARTESIAN_POINT('Ctrl Pts',(-0.765913193856978,1.,-1.89436577771388));
#35520=CARTESIAN_POINT('Ctrl Pts',(-0.766004837062091,1.,-1.88820926433409));
#35521=CARTESIAN_POINT('Ctrl Pts',(-0.766047794851865,1.,-1.88206215302561));
#35522=CARTESIAN_POINT('Ctrl Pts',(-0.766042837036744,1.,-1.87592888967883));
#35523=CARTESIAN_POINT('Ctrl Pts',(-0.765990708546091,1.,-1.86981398314341));
#35524=CARTESIAN_POINT('Ctrl Pts',(-0.765891519092547,1.,-1.86372027063312));
#35525=CARTESIAN_POINT('Ctrl Pts',(-0.765744212909318,1.,-1.85764741390394));
#35526=CARTESIAN_POINT('Ctrl Pts',(-0.765545710619062,1.,-1.85158945130063));
#35527=CARTESIAN_POINT('Ctrl Pts',(-0.765291664862029,1.,-1.84553698875924));
#35528=CARTESIAN_POINT('Ctrl Pts',(-0.764978057881737,1.,-1.83948181064835));
#35529=CARTESIAN_POINT('Ctrl Pts',(-0.764602549687853,1.,-1.83342077227142));
#35530=CARTESIAN_POINT('Ctrl Pts',(-0.764165902605995,1.,-1.82735991200065));
#35531=CARTESIAN_POINT('Ctrl Pts',(-0.763673465462726,1.,-1.82131873145266));
#35532=CARTESIAN_POINT('Ctrl Pts',(-0.763132003836634,1.,-1.8153211840553));
#35533=CARTESIAN_POINT('Ctrl Pts',(-0.762546129463938,1.,-1.80938551463965));
#35534=CARTESIAN_POINT('Ctrl Pts',(-0.761915336443547,1.,-1.80351583877342));
#35535=CARTESIAN_POINT('Ctrl Pts',(-0.761229695230558,1.,-1.79768986997783));
#35536=CARTESIAN_POINT('Ctrl Pts',(-0.760469555880749,1.,-1.7918581561088));
#35537=CARTESIAN_POINT('Ctrl Pts',(-0.759614401110189,1.,-1.78596964884604));
#35538=CARTESIAN_POINT('Ctrl Pts',(-0.758650626677518,1.,-1.77999411220945));
#35539=CARTESIAN_POINT('Ctrl Pts',(-0.757578264077029,1.,-1.77394167108292));
#35540=CARTESIAN_POINT('Ctrl Pts',(-0.75642189602781,1.,-1.76789396002998));
#35541=CARTESIAN_POINT('Ctrl Pts',(-0.755220979974461,1.,-1.76197817240128));
#35542=CARTESIAN_POINT('Ctrl Pts',(-0.754009254027829,1.,-1.75631083600019));
#35543=CARTESIAN_POINT('Ctrl Pts',(-0.752797683531314,1.,-1.75095139468794));
#35544=CARTESIAN_POINT('Ctrl Pts',(-0.751555614164482,1.,-1.74585086852502));
#35545=CARTESIAN_POINT('Ctrl Pts',(-0.750193435981249,1.,-1.74080458267114));
#35546=CARTESIAN_POINT('Ctrl Pts',(-0.74858246295687,1.,-1.7355035168033));
#35547=CARTESIAN_POINT('Ctrl Pts',(-0.746574710097752,1.,-1.72958533647714));
#35548=CARTESIAN_POINT('Ctrl Pts',(-0.744021445433093,1.,-1.72268229916769));
#35549=CARTESIAN_POINT('Ctrl Pts',(-0.74079516202821,1.,-1.71447789751001));
#35550=CARTESIAN_POINT('Ctrl Pts',(-0.736799665716932,1.,-1.70473309004249));
#35551=CARTESIAN_POINT('Ctrl Pts',(-0.731963238685357,1.,-1.69326921972915));
#35552=CARTESIAN_POINT('Ctrl Pts',(-0.726235967982445,1.,-1.67996158451922));
#35553=CARTESIAN_POINT('Ctrl Pts',(-0.71958543378795,1.,-1.66472880551777));
#35554=CARTESIAN_POINT('Ctrl Pts',(-0.711993139340447,1.,-1.64752408828442));
#35555=CARTESIAN_POINT('Ctrl Pts',(-0.705159151977294,1.,-1.6321654166204));
#35556=CARTESIAN_POINT('Ctrl Pts',(-0.699605146398837,1.,-1.61974673471117));
#35557=CARTESIAN_POINT('Ctrl Pts',(-0.69571209787897,1.,-1.61106790957619));
#35558=CARTESIAN_POINT('Ctrl Pts',(-0.693717979106305,1.,-1.60662857109684));
#35559=CARTESIAN_POINT('',(-0.745574324794401,0.,-2.0698113262342));
#35560=CARTESIAN_POINT('Origin',(-0.61342227326009,0.,-2.11275013067528));
#35561=CARTESIAN_POINT('',(-0.61342227326009,1.,-2.11275013067528));
#35562=CARTESIAN_POINT('',(-0.745574324794401,1.,-2.0698113262342));
#35563=CARTESIAN_POINT('',(-0.61342227326009,0.,-2.11275013067528));
#35564=CARTESIAN_POINT('Ctrl Pts',(-0.383122945602004,-1.,-1.7075470150345));
#35565=CARTESIAN_POINT('Ctrl Pts',(-0.383122945602004,1.,-1.7075470150345));
#35566=CARTESIAN_POINT('Ctrl Pts',(-0.384119047315542,-1.,-1.71231062891958));
#35567=CARTESIAN_POINT('Ctrl Pts',(-0.384119047315542,1.,-1.71231062891958));
#35568=CARTESIAN_POINT('Ctrl Pts',(-0.38607079032701,-1.,-1.72162022246158));
#35569=CARTESIAN_POINT('Ctrl Pts',(-0.38607079032701,1.,-1.72162022246158));
#35570=CARTESIAN_POINT('Ctrl Pts',(-0.388877023509191,-1.,-1.7349317097561));
#35571=CARTESIAN_POINT('Ctrl Pts',(-0.388877023509191,1.,-1.7349317097561));
#35572=CARTESIAN_POINT('Ctrl Pts',(-0.392375812294307,-1.,-1.75137405313962));
#35573=CARTESIAN_POINT('Ctrl Pts',(-0.392375812294307,1.,-1.75137405313962));
#35574=CARTESIAN_POINT('Ctrl Pts',(-0.39634619612042,-1.,-1.7697556004756));
#35575=CARTESIAN_POINT('Ctrl Pts',(-0.39634619612042,1.,-1.7697556004756));
#35576=CARTESIAN_POINT('Ctrl Pts',(-0.39991940378308,-1.,-1.78598826347533));
#35577=CARTESIAN_POINT('Ctrl Pts',(-0.39991940378308,1.,-1.78598826347533));
#35578=CARTESIAN_POINT('Ctrl Pts',(-0.403107976170441,-1.,-1.80012077176221));
#35579=CARTESIAN_POINT('Ctrl Pts',(-0.403107976170441,1.,-1.80012077176221));
#35580=CARTESIAN_POINT('Ctrl Pts',(-0.405933518411838,-1.,-1.81223801813988));
#35581=CARTESIAN_POINT('Ctrl Pts',(-0.405933518411838,1.,-1.81223801813988));
#35582=CARTESIAN_POINT('Ctrl Pts',(-0.408428948108533,-1.,-1.8224702267854));
#35583=CARTESIAN_POINT('Ctrl Pts',(-0.408428948108533,1.,-1.8224702267854));
#35584=CARTESIAN_POINT('Ctrl Pts',(-0.410641256301675,-1.,-1.83100408895216));
#35585=CARTESIAN_POINT('Ctrl Pts',(-0.410641256301675,1.,-1.83100408895216));
#35586=CARTESIAN_POINT('Ctrl Pts',(-0.412633125322162,-1.,-1.83808953475839));
#35587=CARTESIAN_POINT('Ctrl Pts',(-0.412633125322162,1.,-1.83808953475839));
#35588=CARTESIAN_POINT('Ctrl Pts',(-0.41448743825434,-1.,-1.8440575707371));
#35589=CARTESIAN_POINT('Ctrl Pts',(-0.41448743825434,1.,-1.8440575707371));
#35590=CARTESIAN_POINT('Ctrl Pts',(-0.416300022038864,-1.,-1.84929312929882));
#35591=CARTESIAN_POINT('Ctrl Pts',(-0.416300022038864,1.,-1.84929312929882));
#35592=CARTESIAN_POINT('Ctrl Pts',(-0.418164129143534,-1.,-1.85417632856234));
#35593=CARTESIAN_POINT('Ctrl Pts',(-0.418164129143534,1.,-1.85417632856234));
#35594=CARTESIAN_POINT('Ctrl Pts',(-0.420157287975619,-1.,-1.85903281096686));
#35595=CARTESIAN_POINT('Ctrl Pts',(-0.420157287975619,1.,-1.85903281096686));
#35596=CARTESIAN_POINT('Ctrl Pts',(-0.422327307418275,-1.,-1.86408083334028));
#35597=CARTESIAN_POINT('Ctrl Pts',(-0.422327307418275,1.,-1.86408083334028));
#35598=CARTESIAN_POINT('Ctrl Pts',(-0.424678177291359,-1.,-1.86937803944323));
#35599=CARTESIAN_POINT('Ctrl Pts',(-0.424678177291359,1.,-1.86937803944323));
#35600=CARTESIAN_POINT('Ctrl Pts',(-0.427183828519102,-1.,-1.87486989291484));
#35601=CARTESIAN_POINT('Ctrl Pts',(-0.427183828519102,1.,-1.87486989291484));
#35602=CARTESIAN_POINT('Ctrl Pts',(-0.429803062482344,-1.,-1.88044229001832));
#35603=CARTESIAN_POINT('Ctrl Pts',(-0.429803062482344,1.,-1.88044229001832));
#35604=CARTESIAN_POINT('Ctrl Pts',(-0.432493038548748,-1.,-1.88596913666793));
#35605=CARTESIAN_POINT('Ctrl Pts',(-0.432493038548748,1.,-1.88596913666793));
#35606=CARTESIAN_POINT('Ctrl Pts',(-0.435225660963383,-1.,-1.89136993975504));
#35607=CARTESIAN_POINT('Ctrl Pts',(-0.435225660963383,1.,-1.89136993975504));
#35608=CARTESIAN_POINT('Ctrl Pts',(-0.437995003948244,-1.,-1.89663648956466));
#35609=CARTESIAN_POINT('Ctrl Pts',(-0.437995003948244,1.,-1.89663648956466));
#35610=CARTESIAN_POINT('Ctrl Pts',(-0.440807833704038,-1.,-1.90180124389086));
#35611=CARTESIAN_POINT('Ctrl Pts',(-0.440807833704038,1.,-1.90180124389086));
#35612=CARTESIAN_POINT('Ctrl Pts',(-0.443677556849151,-1.,-1.90691756144898));
#35613=CARTESIAN_POINT('Ctrl Pts',(-0.443677556849151,1.,-1.90691756144898));
#35614=CARTESIAN_POINT('Ctrl Pts',(-0.446617343485711,-1.,-1.9120369998112));
#35615=CARTESIAN_POINT('Ctrl Pts',(-0.446617343485711,1.,-1.9120369998112));
#35616=CARTESIAN_POINT('Ctrl Pts',(-0.449632260106662,-1.,-1.91718342555755));
#35617=CARTESIAN_POINT('Ctrl Pts',(-0.449632260106662,1.,-1.91718342555755));
#35618=CARTESIAN_POINT('Ctrl Pts',(-0.452719478359432,-1.,-1.92235380648502));
#35619=CARTESIAN_POINT('Ctrl Pts',(-0.452719478359432,1.,-1.92235380648502));
#35620=CARTESIAN_POINT('Ctrl Pts',(-0.455872005174371,-1.,-1.92753067150476));
#35621=CARTESIAN_POINT('Ctrl Pts',(-0.455872005174371,1.,-1.92753067150476));
#35622=CARTESIAN_POINT('Ctrl Pts',(-0.459081234547926,-1.,-1.93269066517934));
#35623=CARTESIAN_POINT('Ctrl Pts',(-0.459081234547926,1.,-1.93269066517934));
#35624=CARTESIAN_POINT('Ctrl Pts',(-0.462340031009056,-1.,-1.93781486640821));
#35625=CARTESIAN_POINT('Ctrl Pts',(-0.462340031009056,1.,-1.93781486640821));
#35626=CARTESIAN_POINT('Ctrl Pts',(-0.46564546202603,-1.,-1.9428979419619));
#35627=CARTESIAN_POINT('Ctrl Pts',(-0.46564546202603,1.,-1.9428979419619));
#35628=CARTESIAN_POINT('Ctrl Pts',(-0.468997482913135,-1.,-1.94794381136514));
#35629=CARTESIAN_POINT('Ctrl Pts',(-0.468997482913135,1.,-1.94794381136514));
#35630=CARTESIAN_POINT('Ctrl Pts',(-0.472397672264072,-1.,-1.95296148278133));
#35631=CARTESIAN_POINT('Ctrl Pts',(-0.472397672264072,1.,-1.95296148278133));
#35632=CARTESIAN_POINT('Ctrl Pts',(-0.475848034683176,-1.,-1.95796111148177));
#35633=CARTESIAN_POINT('Ctrl Pts',(-0.475848034683176,1.,-1.95796111148177));
#35634=CARTESIAN_POINT('Ctrl Pts',(-0.479349583074855,-1.,-1.96294933055943));
#35635=CARTESIAN_POINT('Ctrl Pts',(-0.479349583074855,1.,-1.96294933055943));
#35636=CARTESIAN_POINT('Ctrl Pts',(-0.482901662120691,-1.,-1.96792703422362));
#35637=CARTESIAN_POINT('Ctrl Pts',(-0.482901662120691,1.,-1.96792703422362));
#35638=CARTESIAN_POINT('Ctrl Pts',(-0.486502692907659,-1.,-1.97289186263272));
#35639=CARTESIAN_POINT('Ctrl Pts',(-0.486502692907659,1.,-1.97289186263272));
#35640=CARTESIAN_POINT('Ctrl Pts',(-0.490150627860952,-1.,-1.97783973019229));
#35641=CARTESIAN_POINT('Ctrl Pts',(-0.490150627860952,1.,-1.97783973019229));
#35642=CARTESIAN_POINT('Ctrl Pts',(-0.493843476541495,-1.,-1.98276658761821));
#35643=CARTESIAN_POINT('Ctrl Pts',(-0.493843476541495,1.,-1.98276658761821));
#35644=CARTESIAN_POINT('Ctrl Pts',(-0.497579909545574,-1.,-1.98767044752932));
#35645=CARTESIAN_POINT('Ctrl Pts',(-0.497579909545574,1.,-1.98767044752932));
#35646=CARTESIAN_POINT('Ctrl Pts',(-0.501359287727146,-1.,-1.99255149126155));
#35647=CARTESIAN_POINT('Ctrl Pts',(-0.501359287727146,1.,-1.99255149126155));
#35648=CARTESIAN_POINT('Ctrl Pts',(-0.505181361323026,-1.,-1.99741107463572));
#35649=CARTESIAN_POINT('Ctrl Pts',(-0.505181361323026,1.,-1.99741107463572));
#35650=CARTESIAN_POINT('Ctrl Pts',(-0.509046069886157,-1.,-2.00225107134734));
#35651=CARTESIAN_POINT('Ctrl Pts',(-0.509046069886157,1.,-2.00225107134734));
#35652=CARTESIAN_POINT('Ctrl Pts',(-0.512953306961792,-1.,-2.00707309946949));
#35653=CARTESIAN_POINT('Ctrl Pts',(-0.512953306961792,1.,-2.00707309946949));
#35654=CARTESIAN_POINT('Ctrl Pts',(-0.516902681728687,-1.,-2.01187773939242));
#35655=CARTESIAN_POINT('Ctrl Pts',(-0.516902681728687,1.,-2.01187773939242));
#35656=CARTESIAN_POINT('Ctrl Pts',(-0.52089359039937,-1.,-2.01666477917286));
#35657=CARTESIAN_POINT('Ctrl Pts',(-0.52089359039937,1.,-2.01666477917286));
#35658=CARTESIAN_POINT('Ctrl Pts',(-0.524925318333476,-1.,-2.02143356304698));
#35659=CARTESIAN_POINT('Ctrl Pts',(-0.524925318333476,1.,-2.02143356304698));
#35660=CARTESIAN_POINT('Ctrl Pts',(-0.528997127241914,-1.,-2.0261832908329));
#35661=CARTESIAN_POINT('Ctrl Pts',(-0.528997127241914,1.,-2.0261832908329));
#35662=CARTESIAN_POINT('Ctrl Pts',(-0.533108355132977,-1.,-2.03091336214426));
#35663=CARTESIAN_POINT('Ctrl Pts',(-0.533108355132977,1.,-2.03091336214426));
#35664=CARTESIAN_POINT('Ctrl Pts',(-0.537258489833262,-1.,-2.03562362954037));
#35665=CARTESIAN_POINT('Ctrl Pts',(-0.537258489833262,1.,-2.03562362954037));
#35666=CARTESIAN_POINT('Ctrl Pts',(-0.541447120615659,-1.,-2.04031422690527));
#35667=CARTESIAN_POINT('Ctrl Pts',(-0.541447120615659,1.,-2.04031422690527));
#35668=CARTESIAN_POINT('Ctrl Pts',(-0.54567390381743,-1.,-2.04498544714588));
#35669=CARTESIAN_POINT('Ctrl Pts',(-0.54567390381743,1.,-2.04498544714588));
#35670=CARTESIAN_POINT('Ctrl Pts',(-0.549938525150295,-1.,-2.04963761077958));
#35671=CARTESIAN_POINT('Ctrl Pts',(-0.549938525150295,1.,-2.04963761077958));
#35672=CARTESIAN_POINT('Ctrl Pts',(-0.554240657463906,-1.,-2.05427091604413));
#35673=CARTESIAN_POINT('Ctrl Pts',(-0.554240657463906,1.,-2.05427091604413));
#35674=CARTESIAN_POINT('Ctrl Pts',(-0.558579940185151,-1.,-2.05888537756462));
#35675=CARTESIAN_POINT('Ctrl Pts',(-0.558579940185151,1.,-2.05888537756462));
#35676=CARTESIAN_POINT('Ctrl Pts',(-0.562955993082261,-1.,-2.06348090160589));
#35677=CARTESIAN_POINT('Ctrl Pts',(-0.562955993082261,1.,-2.06348090160589));
#35678=CARTESIAN_POINT('Ctrl Pts',(-0.567368421181087,-1.,-2.06805732997334));
#35679=CARTESIAN_POINT('Ctrl Pts',(-0.567368421181087,1.,-2.06805732997334));
#35680=CARTESIAN_POINT('Ctrl Pts',(-0.571816823242603,-1.,-2.07261449292824));
#35681=CARTESIAN_POINT('Ctrl Pts',(-0.571816823242603,1.,-2.07261449292824));
#35682=CARTESIAN_POINT('Ctrl Pts',(-0.576300797416844,-1.,-2.07715226767559));
#35683=CARTESIAN_POINT('Ctrl Pts',(-0.576300797416844,1.,-2.07715226767559));
#35684=CARTESIAN_POINT('Ctrl Pts',(-0.580819952108063,-1.,-2.08167059018418));
#35685=CARTESIAN_POINT('Ctrl Pts',(-0.580819952108063,1.,-2.08167059018418));
#35686=CARTESIAN_POINT('Ctrl Pts',(-0.585373918991617,-1.,-2.08616943727951));
#35687=CARTESIAN_POINT('Ctrl Pts',(-0.585373918991617,1.,-2.08616943727951));
#35688=CARTESIAN_POINT('Ctrl Pts',(-0.589962365403406,-1.,-2.09064881812129));
#35689=CARTESIAN_POINT('Ctrl Pts',(-0.589962365403406,1.,-2.09064881812129));
#35690=CARTESIAN_POINT('Ctrl Pts',(-0.594585006052162,-1.,-2.0951087622027));
#35691=CARTESIAN_POINT('Ctrl Pts',(-0.594585006052162,1.,-2.0951087622027));
#35692=CARTESIAN_POINT('Ctrl Pts',(-0.599241616420533,-1.,-2.0995493086477));
#35693=CARTESIAN_POINT('Ctrl Pts',(-0.599241616420533,1.,-2.0995493086477));
#35694=CARTESIAN_POINT('Ctrl Pts',(-0.60393203073603,-1.,-2.10397049886949));
#35695=CARTESIAN_POINT('Ctrl Pts',(-0.60393203073603,1.,-2.10397049886949));
#35696=CARTESIAN_POINT('Ctrl Pts',(-0.607711315454876,-1.,-2.1074919961518));
#35697=CARTESIAN_POINT('Ctrl Pts',(-0.607711315454876,1.,-2.1074919961518));
#35698=CARTESIAN_POINT('Ctrl Pts',(-0.610560911689899,-1.,-2.11012443807238));
#35699=CARTESIAN_POINT('Ctrl Pts',(-0.610560911689899,1.,-2.11012443807238));
#35700=CARTESIAN_POINT('Ctrl Pts',(-0.6124673655618,-1.,-2.11187554259986));
#35701=CARTESIAN_POINT('Ctrl Pts',(-0.6124673655618,1.,-2.11187554259986));
#35702=CARTESIAN_POINT('Ctrl Pts',(-0.61342227326009,-1.,-2.11275013067528));
#35703=CARTESIAN_POINT('Ctrl Pts',(-0.61342227326009,1.,-2.11275013067528));
#35704=CARTESIAN_POINT('',(-0.383122945602004,1.,-1.7075470150345));
#35705=CARTESIAN_POINT('Ctrl Pts',(-0.383122945602004,1.,-1.7075470150345));
#35706=CARTESIAN_POINT('Ctrl Pts',(-0.384119047315542,1.,-1.71231062891958));
#35707=CARTESIAN_POINT('Ctrl Pts',(-0.38607079032701,1.,-1.72162022246158));
#35708=CARTESIAN_POINT('Ctrl Pts',(-0.388877023509191,1.,-1.7349317097561));
#35709=CARTESIAN_POINT('Ctrl Pts',(-0.392375812294307,1.,-1.75137405313962));
#35710=CARTESIAN_POINT('Ctrl Pts',(-0.39634619612042,1.,-1.7697556004756));
#35711=CARTESIAN_POINT('Ctrl Pts',(-0.39991940378308,1.,-1.78598826347533));
#35712=CARTESIAN_POINT('Ctrl Pts',(-0.403107976170441,1.,-1.80012077176221));
#35713=CARTESIAN_POINT('Ctrl Pts',(-0.405933518411838,1.,-1.81223801813988));
#35714=CARTESIAN_POINT('Ctrl Pts',(-0.408428948108533,1.,-1.8224702267854));
#35715=CARTESIAN_POINT('Ctrl Pts',(-0.410641256301675,1.,-1.83100408895216));
#35716=CARTESIAN_POINT('Ctrl Pts',(-0.412633125322162,1.,-1.83808953475839));
#35717=CARTESIAN_POINT('Ctrl Pts',(-0.41448743825434,1.,-1.8440575707371));
#35718=CARTESIAN_POINT('Ctrl Pts',(-0.416300022038864,1.,-1.84929312929882));
#35719=CARTESIAN_POINT('Ctrl Pts',(-0.418164129143534,1.,-1.85417632856234));
#35720=CARTESIAN_POINT('Ctrl Pts',(-0.420157287975619,1.,-1.85903281096686));
#35721=CARTESIAN_POINT('Ctrl Pts',(-0.422327307418275,1.,-1.86408083334028));
#35722=CARTESIAN_POINT('Ctrl Pts',(-0.424678177291359,1.,-1.86937803944323));
#35723=CARTESIAN_POINT('Ctrl Pts',(-0.427183828519102,1.,-1.87486989291484));
#35724=CARTESIAN_POINT('Ctrl Pts',(-0.429803062482344,1.,-1.88044229001832));
#35725=CARTESIAN_POINT('Ctrl Pts',(-0.432493038548748,1.,-1.88596913666793));
#35726=CARTESIAN_POINT('Ctrl Pts',(-0.435225660963383,1.,-1.89136993975504));
#35727=CARTESIAN_POINT('Ctrl Pts',(-0.437995003948244,1.,-1.89663648956466));
#35728=CARTESIAN_POINT('Ctrl Pts',(-0.440807833704038,1.,-1.90180124389086));
#35729=CARTESIAN_POINT('Ctrl Pts',(-0.443677556849151,1.,-1.90691756144898));
#35730=CARTESIAN_POINT('Ctrl Pts',(-0.446617343485711,1.,-1.9120369998112));
#35731=CARTESIAN_POINT('Ctrl Pts',(-0.449632260106662,1.,-1.91718342555755));
#35732=CARTESIAN_POINT('Ctrl Pts',(-0.452719478359432,1.,-1.92235380648502));
#35733=CARTESIAN_POINT('Ctrl Pts',(-0.455872005174371,1.,-1.92753067150476));
#35734=CARTESIAN_POINT('Ctrl Pts',(-0.459081234547926,1.,-1.93269066517934));
#35735=CARTESIAN_POINT('Ctrl Pts',(-0.462340031009056,1.,-1.93781486640821));
#35736=CARTESIAN_POINT('Ctrl Pts',(-0.46564546202603,1.,-1.9428979419619));
#35737=CARTESIAN_POINT('Ctrl Pts',(-0.468997482913135,1.,-1.94794381136514));
#35738=CARTESIAN_POINT('Ctrl Pts',(-0.472397672264072,1.,-1.95296148278133));
#35739=CARTESIAN_POINT('Ctrl Pts',(-0.475848034683176,1.,-1.95796111148177));
#35740=CARTESIAN_POINT('Ctrl Pts',(-0.479349583074855,1.,-1.96294933055943));
#35741=CARTESIAN_POINT('Ctrl Pts',(-0.482901662120691,1.,-1.96792703422362));
#35742=CARTESIAN_POINT('Ctrl Pts',(-0.486502692907659,1.,-1.97289186263272));
#35743=CARTESIAN_POINT('Ctrl Pts',(-0.490150627860952,1.,-1.97783973019229));
#35744=CARTESIAN_POINT('Ctrl Pts',(-0.493843476541495,1.,-1.98276658761821));
#35745=CARTESIAN_POINT('Ctrl Pts',(-0.497579909545574,1.,-1.98767044752932));
#35746=CARTESIAN_POINT('Ctrl Pts',(-0.501359287727146,1.,-1.99255149126155));
#35747=CARTESIAN_POINT('Ctrl Pts',(-0.505181361323026,1.,-1.99741107463572));
#35748=CARTESIAN_POINT('Ctrl Pts',(-0.509046069886157,1.,-2.00225107134734));
#35749=CARTESIAN_POINT('Ctrl Pts',(-0.512953306961792,1.,-2.00707309946949));
#35750=CARTESIAN_POINT('Ctrl Pts',(-0.516902681728687,1.,-2.01187773939242));
#35751=CARTESIAN_POINT('Ctrl Pts',(-0.52089359039937,1.,-2.01666477917286));
#35752=CARTESIAN_POINT('Ctrl Pts',(-0.524925318333476,1.,-2.02143356304698));
#35753=CARTESIAN_POINT('Ctrl Pts',(-0.528997127241914,1.,-2.0261832908329));
#35754=CARTESIAN_POINT('Ctrl Pts',(-0.533108355132977,1.,-2.03091336214426));
#35755=CARTESIAN_POINT('Ctrl Pts',(-0.537258489833262,1.,-2.03562362954037));
#35756=CARTESIAN_POINT('Ctrl Pts',(-0.541447120615659,1.,-2.04031422690527));
#35757=CARTESIAN_POINT('Ctrl Pts',(-0.54567390381743,1.,-2.04498544714588));
#35758=CARTESIAN_POINT('Ctrl Pts',(-0.549938525150295,1.,-2.04963761077958));
#35759=CARTESIAN_POINT('Ctrl Pts',(-0.554240657463906,1.,-2.05427091604413));
#35760=CARTESIAN_POINT('Ctrl Pts',(-0.558579940185151,1.,-2.05888537756462));
#35761=CARTESIAN_POINT('Ctrl Pts',(-0.562955993082261,1.,-2.06348090160589));
#35762=CARTESIAN_POINT('Ctrl Pts',(-0.567368421181087,1.,-2.06805732997334));
#35763=CARTESIAN_POINT('Ctrl Pts',(-0.571816823242603,1.,-2.07261449292824));
#35764=CARTESIAN_POINT('Ctrl Pts',(-0.576300797416844,1.,-2.07715226767559));
#35765=CARTESIAN_POINT('Ctrl Pts',(-0.580819952108063,1.,-2.08167059018418));
#35766=CARTESIAN_POINT('Ctrl Pts',(-0.585373918991617,1.,-2.08616943727951));
#35767=CARTESIAN_POINT('Ctrl Pts',(-0.589962365403406,1.,-2.09064881812129));
#35768=CARTESIAN_POINT('Ctrl Pts',(-0.594585006052162,1.,-2.0951087622027));
#35769=CARTESIAN_POINT('Ctrl Pts',(-0.599241616420533,1.,-2.0995493086477));
#35770=CARTESIAN_POINT('Ctrl Pts',(-0.60393203073603,1.,-2.10397049886949));
#35771=CARTESIAN_POINT('Ctrl Pts',(-0.607711315454876,1.,-2.1074919961518));
#35772=CARTESIAN_POINT('Ctrl Pts',(-0.610560911689899,1.,-2.11012443807238));
#35773=CARTESIAN_POINT('Ctrl Pts',(-0.6124673655618,1.,-2.11187554259986));
#35774=CARTESIAN_POINT('Ctrl Pts',(-0.61342227326009,1.,-2.11275013067528));
#35775=CARTESIAN_POINT('',(-0.383122945602003,0.,-1.7075470150345));
#35776=CARTESIAN_POINT('Origin',(0.,0.,0.));
#35777=CARTESIAN_POINT('',(-0.163289472382896,1.,-1.74236521665491));
#35778=CARTESIAN_POINT('Origin',(0.,1.,0.));
#35779=CARTESIAN_POINT('',(-0.163289472382896,0.,-1.74236521665491));
#35780=CARTESIAN_POINT('Ctrl Pts',(-0.0694764450219581,-1.,-2.19890268624765));
#35781=CARTESIAN_POINT('Ctrl Pts',(-0.0694764450219581,1.,-2.19890268624765));
#35782=CARTESIAN_POINT('Ctrl Pts',(-0.070114353632549,-1.,-2.19777582085423));
#35783=CARTESIAN_POINT('Ctrl Pts',(-0.070114353632549,1.,-2.19777582085423));
#35784=CARTESIAN_POINT('Ctrl Pts',(-0.0713863779526154,-1.,-2.19552129484002));
#35785=CARTESIAN_POINT('Ctrl Pts',(-0.0713863779526154,1.,-2.19552129484002));
#35786=CARTESIAN_POINT('Ctrl Pts',(-0.0732830357306725,-1.,-2.19213712013662));
#35787=CARTESIAN_POINT('Ctrl Pts',(-0.0732830357306725,1.,-2.19213712013662));
#35788=CARTESIAN_POINT('Ctrl Pts',(-0.0757891465836148,-1.,-2.1876201139953));
#35789=CARTESIAN_POINT('Ctrl Pts',(-0.0757891465836148,1.,-2.1876201139953));
#35790=CARTESIAN_POINT('Ctrl Pts',(-0.0788837727685243,-1.,-2.18196589448887));
#35791=CARTESIAN_POINT('Ctrl Pts',(-0.0788837727685243,1.,-2.18196589448887));
#35792=CARTESIAN_POINT('Ctrl Pts',(-0.0819402680872765,-1.,-2.176303712113));
#35793=CARTESIAN_POINT('Ctrl Pts',(-0.0819402680872765,1.,-2.176303712113));
#35794=CARTESIAN_POINT('Ctrl Pts',(-0.0849584620835372,-1.,-2.17063357870952));
#35795=CARTESIAN_POINT('Ctrl Pts',(-0.0849584620835372,1.,-2.17063357870952));
#35796=CARTESIAN_POINT('Ctrl Pts',(-0.0879381291386923,-1.,-2.16495552645014));
#35797=CARTESIAN_POINT('Ctrl Pts',(-0.0879381291386923,1.,-2.16495552645014));
#35798=CARTESIAN_POINT('Ctrl Pts',(-0.0908789888107265,-1.,-2.15926961544516));
#35799=CARTESIAN_POINT('Ctrl Pts',(-0.0908789888107265,1.,-2.15926961544516));
#35800=CARTESIAN_POINT('Ctrl Pts',(-0.0937807218867643,-1.,-2.1535759397817));
#35801=CARTESIAN_POINT('Ctrl Pts',(-0.0937807218867643,1.,-2.1535759397817));
#35802=CARTESIAN_POINT('Ctrl Pts',(-0.0966429852305459,-1.,-2.14787463531795));
#35803=CARTESIAN_POINT('Ctrl Pts',(-0.0966429852305459,1.,-2.14787463531795));
#35804=CARTESIAN_POINT('Ctrl Pts',(-0.0994654261990915,-1.,-2.14216588396025));
#35805=CARTESIAN_POINT('Ctrl Pts',(-0.0994654261990915,1.,-2.14216588396025));
#35806=CARTESIAN_POINT('Ctrl Pts',(-0.1022477005561,-1.,-2.13644992667165));
#35807=CARTESIAN_POINT('Ctrl Pts',(-0.1022477005561,1.,-2.13644992667165));
#35808=CARTESIAN_POINT('Ctrl Pts',(-0.104989479152739,-1.,-2.13072704887293));
#35809=CARTESIAN_POINT('Ctrl Pts',(-0.104989479152739,1.,-2.13072704887293));
#35810=CARTESIAN_POINT('Ctrl Pts',(-0.10769043523109,-1.,-2.12499752307));
#35811=CARTESIAN_POINT('Ctrl Pts',(-0.10769043523109,1.,-2.12499752307));
#35812=CARTESIAN_POINT('Ctrl Pts',(-0.110350236135025,-1.,-2.11926155590865));
#35813=CARTESIAN_POINT('Ctrl Pts',(-0.110350236135025,1.,-2.11926155590865));
#35814=CARTESIAN_POINT('Ctrl Pts',(-0.112968534419737,-1.,-2.11351924490306));
#35815=CARTESIAN_POINT('Ctrl Pts',(-0.112968534419737,1.,-2.11351924490306));
#35816=CARTESIAN_POINT('Ctrl Pts',(-0.115544957687926,-1.,-2.10777050261309));
#35817=CARTESIAN_POINT('Ctrl Pts',(-0.115544957687926,1.,-2.10777050261309));
#35818=CARTESIAN_POINT('Ctrl Pts',(-0.118079107988355,-1.,-2.102015121329));
#35819=CARTESIAN_POINT('Ctrl Pts',(-0.118079107988355,1.,-2.102015121329));
#35820=CARTESIAN_POINT('Ctrl Pts',(-0.120570567965122,-1.,-2.0962529286773));
#35821=CARTESIAN_POINT('Ctrl Pts',(-0.120570567965122,1.,-2.0962529286773));
#35822=CARTESIAN_POINT('Ctrl Pts',(-0.123018905621083,-1.,-2.09048392424825));
#35823=CARTESIAN_POINT('Ctrl Pts',(-0.123018905621083,1.,-2.09048392424825));
#35824=CARTESIAN_POINT('Ctrl Pts',(-0.125423679412061,-1.,-2.08470840653643));
#35825=CARTESIAN_POINT('Ctrl Pts',(-0.125423679412061,1.,-2.08470840653643));
#35826=CARTESIAN_POINT('Ctrl Pts',(-0.12778444527612,-1.,-2.07892715110987));
#35827=CARTESIAN_POINT('Ctrl Pts',(-0.12778444527612,1.,-2.07892715110987));
#35828=CARTESIAN_POINT('Ctrl Pts',(-0.130100748328403,-1.,-2.07314114713063));
#35829=CARTESIAN_POINT('Ctrl Pts',(-0.130100748328403,1.,-2.07314114713063));
#35830=CARTESIAN_POINT('Ctrl Pts',(-0.13237211154771,-1.,-2.06735123910326));
#35831=CARTESIAN_POINT('Ctrl Pts',(-0.13237211154771,1.,-2.06735123910326));
#35832=CARTESIAN_POINT('Ctrl Pts',(-0.134598026192106,-1.,-2.06155781517842));
#35833=CARTESIAN_POINT('Ctrl Pts',(-0.134598026192106,1.,-2.06155781517842));
#35834=CARTESIAN_POINT('Ctrl Pts',(-0.136777941218044,-1.,-2.05576044414264));
#35835=CARTESIAN_POINT('Ctrl Pts',(-0.136777941218044,1.,-2.05576044414264));
#35836=CARTESIAN_POINT('Ctrl Pts',(-0.138911255368966,-1.,-2.04995762001328));
#35837=CARTESIAN_POINT('Ctrl Pts',(-0.138911255368966,1.,-2.04995762001328));
#35838=CARTESIAN_POINT('Ctrl Pts',(-0.140997332152546,-1.,-2.04414757947916));
#35839=CARTESIAN_POINT('Ctrl Pts',(-0.140997332152546,1.,-2.04414757947916));
#35840=CARTESIAN_POINT('Ctrl Pts',(-0.143035515058209,-1.,-2.03832911025912));
#35841=CARTESIAN_POINT('Ctrl Pts',(-0.143035515058209,1.,-2.03832911025912));
#35842=CARTESIAN_POINT('Ctrl Pts',(-0.145025140186057,-1.,-2.03250223739942));
#35843=CARTESIAN_POINT('Ctrl Pts',(-0.145025140186057,1.,-2.03250223739942));
#35844=CARTESIAN_POINT('Ctrl Pts',(-0.146965557332583,-1.,-2.02666926182017));
#35845=CARTESIAN_POINT('Ctrl Pts',(-0.146965557332583,1.,-2.02666926182017));
#35846=CARTESIAN_POINT('Ctrl Pts',(-0.148856124775337,-1.,-2.02083464969894));
#35847=CARTESIAN_POINT('Ctrl Pts',(-0.148856124775337,1.,-2.02083464969894));
#35848=CARTESIAN_POINT('Ctrl Pts',(-0.150696157673078,-1.,-2.01500291940238));
#35849=CARTESIAN_POINT('Ctrl Pts',(-0.150696157673078,1.,-2.01500291940238));
#35850=CARTESIAN_POINT('Ctrl Pts',(-0.15248488362145,-1.,-2.00917680318424));
#35851=CARTESIAN_POINT('Ctrl Pts',(-0.15248488362145,1.,-2.00917680318424));
#35852=CARTESIAN_POINT('Ctrl Pts',(-0.154221403049722,-1.,-2.00335565310543));
#35853=CARTESIAN_POINT('Ctrl Pts',(-0.154221403049722,1.,-2.00335565310543));
#35854=CARTESIAN_POINT('Ctrl Pts',(-0.155904629548783,-1.,-1.99753284771497));
#35855=CARTESIAN_POINT('Ctrl Pts',(-0.155904629548783,1.,-1.99753284771497));
#35856=CARTESIAN_POINT('Ctrl Pts',(-0.157533331459227,-1.,-1.99169810931908));
#35857=CARTESIAN_POINT('Ctrl Pts',(-0.157533331459227,1.,-1.99169810931908));
#35858=CARTESIAN_POINT('Ctrl Pts',(-0.159106226437299,-1.,-1.98584238283292));
#35859=CARTESIAN_POINT('Ctrl Pts',(-0.159106226437299,1.,-1.98584238283292));
#35860=CARTESIAN_POINT('Ctrl Pts',(-0.160622060784611,-1.,-1.97996195437559));
#35861=CARTESIAN_POINT('Ctrl Pts',(-0.160622060784611,1.,-1.97996195437559));
#35862=CARTESIAN_POINT('Ctrl Pts',(-0.162079693556289,-1.,-1.97406280235188));
#35863=CARTESIAN_POINT('Ctrl Pts',(-0.162079693556289,1.,-1.97406280235188));
#35864=CARTESIAN_POINT('Ctrl Pts',(-0.163478185457734,-1.,-1.96816512677967));
#35865=CARTESIAN_POINT('Ctrl Pts',(-0.163478185457734,1.,-1.96816512677967));
#35866=CARTESIAN_POINT('Ctrl Pts',(-0.164816568920269,-1.,-1.96229379940136));
#35867=CARTESIAN_POINT('Ctrl Pts',(-0.164816568920269,1.,-1.96229379940136));
#35868=CARTESIAN_POINT('Ctrl Pts',(-0.166093592002812,-1.,-1.9564675971873));
#35869=CARTESIAN_POINT('Ctrl Pts',(-0.166093592002812,1.,-1.9564675971873));
#35870=CARTESIAN_POINT('Ctrl Pts',(-0.167307501784475,-1.,-1.95069027794294));
#35871=CARTESIAN_POINT('Ctrl Pts',(-0.167307501784475,1.,-1.95069027794294));
#35872=CARTESIAN_POINT('Ctrl Pts',(-0.168455741607556,-1.,-1.94493757756931));
#35873=CARTESIAN_POINT('Ctrl Pts',(-0.168455741607556,1.,-1.94493757756931));
#35874=CARTESIAN_POINT('Ctrl Pts',(-0.169534904817491,-1.,-1.93915639211581));
#35875=CARTESIAN_POINT('Ctrl Pts',(-0.169534904817491,1.,-1.93915639211581));
#35876=CARTESIAN_POINT('Ctrl Pts',(-0.170541253116202,-1.,-1.93329183155539));
#35877=CARTESIAN_POINT('Ctrl Pts',(-0.170541253116202,1.,-1.93329183155539));
#35878=CARTESIAN_POINT('Ctrl Pts',(-0.171471191532988,-1.,-1.92731093582036));
#35879=CARTESIAN_POINT('Ctrl Pts',(-0.171471191532988,1.,-1.92731093582036));
#35880=CARTESIAN_POINT('Ctrl Pts',(-0.172321621259514,-1.,-1.9212233439798));
#35881=CARTESIAN_POINT('Ctrl Pts',(-0.172321621259514,1.,-1.9212233439798));
#35882=CARTESIAN_POINT('Ctrl Pts',(-0.173090695383496,-1.,-1.91511429159527));
#35883=CARTESIAN_POINT('Ctrl Pts',(-0.173090695383496,1.,-1.91511429159527));
#35884=CARTESIAN_POINT('Ctrl Pts',(-0.173776635257817,-1.,-1.90911693975267));
#35885=CARTESIAN_POINT('Ctrl Pts',(-0.173776635257817,1.,-1.90911693975267));
#35886=CARTESIAN_POINT('Ctrl Pts',(-0.174375518661085,-1.,-1.90335253862834));
#35887=CARTESIAN_POINT('Ctrl Pts',(-0.174375518661085,1.,-1.90335253862834));
#35888=CARTESIAN_POINT('Ctrl Pts',(-0.174879405091263,-1.,-1.89788101117132));
#35889=CARTESIAN_POINT('Ctrl Pts',(-0.174879405091263,1.,-1.89788101117132));
#35890=CARTESIAN_POINT('Ctrl Pts',(-0.175274276190844,-1.,-1.892646301985));
#35891=CARTESIAN_POINT('Ctrl Pts',(-0.175274276190844,1.,-1.892646301985));
#35892=CARTESIAN_POINT('Ctrl Pts',(-0.175538155840648,-1.,-1.88742606273259));
#35893=CARTESIAN_POINT('Ctrl Pts',(-0.175538155840648,1.,-1.88742606273259));
#35894=CARTESIAN_POINT('Ctrl Pts',(-0.175644148889699,-1.,-1.88188663145367));
#35895=CARTESIAN_POINT('Ctrl Pts',(-0.175644148889699,1.,-1.88188663145367));
#35896=CARTESIAN_POINT('Ctrl Pts',(-0.175563480746485,-1.,-1.87563767773588));
#35897=CARTESIAN_POINT('Ctrl Pts',(-0.175563480746485,1.,-1.87563767773588));
#35898=CARTESIAN_POINT('Ctrl Pts',(-0.175268337590758,-1.,-1.86828349694799));
#35899=CARTESIAN_POINT('Ctrl Pts',(-0.175268337590758,1.,-1.86828349694799));
#35900=CARTESIAN_POINT('Ctrl Pts',(-0.17473525927603,-1.,-1.85948367088837));
#35901=CARTESIAN_POINT('Ctrl Pts',(-0.17473525927603,1.,-1.85948367088837));
#35902=CARTESIAN_POINT('Ctrl Pts',(-0.173946627587731,-1.,-1.8489811319852));
#35903=CARTESIAN_POINT('Ctrl Pts',(-0.173946627587731,1.,-1.8489811319852));
#35904=CARTESIAN_POINT('Ctrl Pts',(-0.1728894428919,-1.,-1.83658380527692));
#35905=CARTESIAN_POINT('Ctrl Pts',(-0.1728894428919,1.,-1.83658380527692));
#35906=CARTESIAN_POINT('Ctrl Pts',(-0.171554770204119,-1.,-1.82215766811545));
#35907=CARTESIAN_POINT('Ctrl Pts',(-0.171554770204119,1.,-1.82215766811545));
#35908=CARTESIAN_POINT('Ctrl Pts',(-0.169936923904608,-1.,-1.80561530629706));
#35909=CARTESIAN_POINT('Ctrl Pts',(-0.169936923904608,1.,-1.80561530629706));
#35910=CARTESIAN_POINT('Ctrl Pts',(-0.168032772805197,-1.,-1.7869064998507));
#35911=CARTESIAN_POINT('Ctrl Pts',(-0.168032772805197,1.,-1.7869064998507));
#35912=CARTESIAN_POINT('Ctrl Pts',(-0.1662793551464,-1.,-1.77018771684844));
#35913=CARTESIAN_POINT('Ctrl Pts',(-0.1662793551464,1.,-1.77018771684844));
#35914=CARTESIAN_POINT('Ctrl Pts',(-0.164834765707158,-1.,-1.75666056638427));
#35915=CARTESIAN_POINT('Ctrl Pts',(-0.164834765707158,1.,-1.75666056638427));
#35916=CARTESIAN_POINT('Ctrl Pts',(-0.163814161002002,-1.,-1.7472034950333));
#35917=CARTESIAN_POINT('Ctrl Pts',(-0.163814161002002,1.,-1.7472034950333));
#35918=CARTESIAN_POINT('Ctrl Pts',(-0.163289472382896,-1.,-1.74236521665491));
#35919=CARTESIAN_POINT('Ctrl Pts',(-0.163289472382896,1.,-1.74236521665491));
#35920=CARTESIAN_POINT('',(-0.0694764450219581,1.,-2.19890268624765));
#35921=CARTESIAN_POINT('Ctrl Pts',(-0.0694764450219581,1.,-2.19890268624765));
#35922=CARTESIAN_POINT('Ctrl Pts',(-0.070114353632549,1.,-2.19777582085423));
#35923=CARTESIAN_POINT('Ctrl Pts',(-0.0713863779526154,1.,-2.19552129484002));
#35924=CARTESIAN_POINT('Ctrl Pts',(-0.0732830357306725,1.,-2.19213712013662));
#35925=CARTESIAN_POINT('Ctrl Pts',(-0.0757891465836148,1.,-2.1876201139953));
#35926=CARTESIAN_POINT('Ctrl Pts',(-0.0788837727685243,1.,-2.18196589448887));
#35927=CARTESIAN_POINT('Ctrl Pts',(-0.0819402680872765,1.,-2.176303712113));
#35928=CARTESIAN_POINT('Ctrl Pts',(-0.0849584620835372,1.,-2.17063357870952));
#35929=CARTESIAN_POINT('Ctrl Pts',(-0.0879381291386923,1.,-2.16495552645014));
#35930=CARTESIAN_POINT('Ctrl Pts',(-0.0908789888107265,1.,-2.15926961544516));
#35931=CARTESIAN_POINT('Ctrl Pts',(-0.0937807218867643,1.,-2.1535759397817));
#35932=CARTESIAN_POINT('Ctrl Pts',(-0.0966429852305459,1.,-2.14787463531795));
#35933=CARTESIAN_POINT('Ctrl Pts',(-0.0994654261990915,1.,-2.14216588396025));
#35934=CARTESIAN_POINT('Ctrl Pts',(-0.1022477005561,1.,-2.13644992667165));
#35935=CARTESIAN_POINT('Ctrl Pts',(-0.104989479152739,1.,-2.13072704887293));
#35936=CARTESIAN_POINT('Ctrl Pts',(-0.10769043523109,1.,-2.12499752307));
#35937=CARTESIAN_POINT('Ctrl Pts',(-0.110350236135025,1.,-2.11926155590865));
#35938=CARTESIAN_POINT('Ctrl Pts',(-0.112968534419737,1.,-2.11351924490306));
#35939=CARTESIAN_POINT('Ctrl Pts',(-0.115544957687926,1.,-2.10777050261309));
#35940=CARTESIAN_POINT('Ctrl Pts',(-0.118079107988355,1.,-2.102015121329));
#35941=CARTESIAN_POINT('Ctrl Pts',(-0.120570567965122,1.,-2.0962529286773));
#35942=CARTESIAN_POINT('Ctrl Pts',(-0.123018905621083,1.,-2.09048392424825));
#35943=CARTESIAN_POINT('Ctrl Pts',(-0.125423679412061,1.,-2.08470840653643));
#35944=CARTESIAN_POINT('Ctrl Pts',(-0.12778444527612,1.,-2.07892715110987));
#35945=CARTESIAN_POINT('Ctrl Pts',(-0.130100748328403,1.,-2.07314114713063));
#35946=CARTESIAN_POINT('Ctrl Pts',(-0.13237211154771,1.,-2.06735123910326));
#35947=CARTESIAN_POINT('Ctrl Pts',(-0.134598026192106,1.,-2.06155781517842));
#35948=CARTESIAN_POINT('Ctrl Pts',(-0.136777941218044,1.,-2.05576044414264));
#35949=CARTESIAN_POINT('Ctrl Pts',(-0.138911255368966,1.,-2.04995762001328));
#35950=CARTESIAN_POINT('Ctrl Pts',(-0.140997332152546,1.,-2.04414757947916));
#35951=CARTESIAN_POINT('Ctrl Pts',(-0.143035515058209,1.,-2.03832911025912));
#35952=CARTESIAN_POINT('Ctrl Pts',(-0.145025140186057,1.,-2.03250223739942));
#35953=CARTESIAN_POINT('Ctrl Pts',(-0.146965557332583,1.,-2.02666926182017));
#35954=CARTESIAN_POINT('Ctrl Pts',(-0.148856124775337,1.,-2.02083464969894));
#35955=CARTESIAN_POINT('Ctrl Pts',(-0.150696157673078,1.,-2.01500291940238));
#35956=CARTESIAN_POINT('Ctrl Pts',(-0.15248488362145,1.,-2.00917680318424));
#35957=CARTESIAN_POINT('Ctrl Pts',(-0.154221403049722,1.,-2.00335565310543));
#35958=CARTESIAN_POINT('Ctrl Pts',(-0.155904629548783,1.,-1.99753284771497));
#35959=CARTESIAN_POINT('Ctrl Pts',(-0.157533331459227,1.,-1.99169810931908));
#35960=CARTESIAN_POINT('Ctrl Pts',(-0.159106226437299,1.,-1.98584238283292));
#35961=CARTESIAN_POINT('Ctrl Pts',(-0.160622060784611,1.,-1.97996195437559));
#35962=CARTESIAN_POINT('Ctrl Pts',(-0.162079693556289,1.,-1.97406280235188));
#35963=CARTESIAN_POINT('Ctrl Pts',(-0.163478185457734,1.,-1.96816512677967));
#35964=CARTESIAN_POINT('Ctrl Pts',(-0.164816568920269,1.,-1.96229379940136));
#35965=CARTESIAN_POINT('Ctrl Pts',(-0.166093592002812,1.,-1.9564675971873));
#35966=CARTESIAN_POINT('Ctrl Pts',(-0.167307501784475,1.,-1.95069027794294));
#35967=CARTESIAN_POINT('Ctrl Pts',(-0.168455741607556,1.,-1.94493757756931));
#35968=CARTESIAN_POINT('Ctrl Pts',(-0.169534904817491,1.,-1.93915639211581));
#35969=CARTESIAN_POINT('Ctrl Pts',(-0.170541253116202,1.,-1.93329183155539));
#35970=CARTESIAN_POINT('Ctrl Pts',(-0.171471191532988,1.,-1.92731093582036));
#35971=CARTESIAN_POINT('Ctrl Pts',(-0.172321621259514,1.,-1.9212233439798));
#35972=CARTESIAN_POINT('Ctrl Pts',(-0.173090695383496,1.,-1.91511429159527));
#35973=CARTESIAN_POINT('Ctrl Pts',(-0.173776635257817,1.,-1.90911693975267));
#35974=CARTESIAN_POINT('Ctrl Pts',(-0.174375518661085,1.,-1.90335253862834));
#35975=CARTESIAN_POINT('Ctrl Pts',(-0.174879405091263,1.,-1.89788101117132));
#35976=CARTESIAN_POINT('Ctrl Pts',(-0.175274276190844,1.,-1.892646301985));
#35977=CARTESIAN_POINT('Ctrl Pts',(-0.175538155840648,1.,-1.88742606273259));
#35978=CARTESIAN_POINT('Ctrl Pts',(-0.175644148889699,1.,-1.88188663145367));
#35979=CARTESIAN_POINT('Ctrl Pts',(-0.175563480746485,1.,-1.87563767773588));
#35980=CARTESIAN_POINT('Ctrl Pts',(-0.175268337590758,1.,-1.86828349694799));
#35981=CARTESIAN_POINT('Ctrl Pts',(-0.17473525927603,1.,-1.85948367088837));
#35982=CARTESIAN_POINT('Ctrl Pts',(-0.173946627587731,1.,-1.8489811319852));
#35983=CARTESIAN_POINT('Ctrl Pts',(-0.1728894428919,1.,-1.83658380527692));
#35984=CARTESIAN_POINT('Ctrl Pts',(-0.171554770204119,1.,-1.82215766811545));
#35985=CARTESIAN_POINT('Ctrl Pts',(-0.169936923904608,1.,-1.80561530629706));
#35986=CARTESIAN_POINT('Ctrl Pts',(-0.168032772805197,1.,-1.7869064998507));
#35987=CARTESIAN_POINT('Ctrl Pts',(-0.1662793551464,1.,-1.77018771684844));
#35988=CARTESIAN_POINT('Ctrl Pts',(-0.164834765707158,1.,-1.75666056638427));
#35989=CARTESIAN_POINT('Ctrl Pts',(-0.163814161002002,1.,-1.7472034950333));
#35990=CARTESIAN_POINT('Ctrl Pts',(-0.163289472382896,1.,-1.74236521665491));
#35991=CARTESIAN_POINT('',(-0.0694764450219581,0.,-2.19890268624765));
#35992=CARTESIAN_POINT('Origin',(0.0694764450219584,0.,-2.19890268624765));
#35993=CARTESIAN_POINT('',(0.0694764450219584,1.,-2.19890268624765));
#35994=CARTESIAN_POINT('',(-0.0694764450219581,1.,-2.19890268624765));
#35995=CARTESIAN_POINT('',(0.0694764450219584,0.,-2.19890268624765));
#35996=CARTESIAN_POINT('Ctrl Pts',(0.163289472382896,-1.,-1.74236521665491));
#35997=CARTESIAN_POINT('Ctrl Pts',(0.163289472382896,1.,-1.74236521665491));
#35998=CARTESIAN_POINT('Ctrl Pts',(0.163814161002474,-1.,-1.74720349503904));
#35999=CARTESIAN_POINT('Ctrl Pts',(0.163814161002474,1.,-1.74720349503904));
#36000=CARTESIAN_POINT('Ctrl Pts',(0.164834765708484,-1.,-1.75666056640041));
#36001=CARTESIAN_POINT('Ctrl Pts',(0.164834765708484,1.,-1.75666056640041));
#36002=CARTESIAN_POINT('Ctrl Pts',(0.166279355148738,-1.,-1.77018771687692));
#36003=CARTESIAN_POINT('Ctrl Pts',(0.166279355148738,1.,-1.77018771687692));
#36004=CARTESIAN_POINT('Ctrl Pts',(0.16803277280837,-1.,-1.78690649988931));
#36005=CARTESIAN_POINT('Ctrl Pts',(0.16803277280837,1.,-1.78690649988931));
#36006=CARTESIAN_POINT('Ctrl Pts',(0.169936923908078,-1.,-1.80561530633924));
#36007=CARTESIAN_POINT('Ctrl Pts',(0.169936923908078,1.,-1.80561530633924));
#36008=CARTESIAN_POINT('Ctrl Pts',(0.171554770207306,-1.,-1.82215766815414));
#36009=CARTESIAN_POINT('Ctrl Pts',(0.171554770207306,1.,-1.82215766815414));
#36010=CARTESIAN_POINT('Ctrl Pts',(0.17288944289442,-1.,-1.83658380530747));
#36011=CARTESIAN_POINT('Ctrl Pts',(0.17288944289442,1.,-1.83658380530747));
#36012=CARTESIAN_POINT('Ctrl Pts',(0.173946627589401,-1.,-1.84898113200543));
#36013=CARTESIAN_POINT('Ctrl Pts',(0.173946627589401,1.,-1.84898113200543));
#36014=CARTESIAN_POINT('Ctrl Pts',(0.174735259276856,-1.,-1.85948367089838));
#36015=CARTESIAN_POINT('Ctrl Pts',(0.174735259276856,1.,-1.85948367089838));
#36016=CARTESIAN_POINT('Ctrl Pts',(0.175268337590901,-1.,-1.86828349694972));
#36017=CARTESIAN_POINT('Ctrl Pts',(0.175268337590901,1.,-1.86828349694972));
#36018=CARTESIAN_POINT('Ctrl Pts',(0.175563480746205,-1.,-1.87563767773249));
#36019=CARTESIAN_POINT('Ctrl Pts',(0.175563480746205,1.,-1.87563767773249));
#36020=CARTESIAN_POINT('Ctrl Pts',(0.175644148889271,-1.,-1.88188663144846));
#36021=CARTESIAN_POINT('Ctrl Pts',(0.175644148889271,1.,-1.88188663144846));
#36022=CARTESIAN_POINT('Ctrl Pts',(0.175538155840286,-1.,-1.88742606272818));
#36023=CARTESIAN_POINT('Ctrl Pts',(0.175538155840286,1.,-1.88742606272818));
#36024=CARTESIAN_POINT('Ctrl Pts',(0.175274276190664,-1.,-1.89264630198279));
#36025=CARTESIAN_POINT('Ctrl Pts',(0.175274276190664,1.,-1.89264630198279));
#36026=CARTESIAN_POINT('Ctrl Pts',(0.174879405091277,-1.,-1.89788101117148));
#36027=CARTESIAN_POINT('Ctrl Pts',(0.174879405091277,1.,-1.89788101117148));
#36028=CARTESIAN_POINT('Ctrl Pts',(0.174375518661222,-1.,-1.90335253863003));
#36029=CARTESIAN_POINT('Ctrl Pts',(0.174375518661222,1.,-1.90335253863003));
#36030=CARTESIAN_POINT('Ctrl Pts',(0.173776635257984,-1.,-1.90911693975475));
#36031=CARTESIAN_POINT('Ctrl Pts',(0.173776635257984,1.,-1.90911693975475));
#36032=CARTESIAN_POINT('Ctrl Pts',(0.173090695383619,-1.,-1.91511429159681));
#36033=CARTESIAN_POINT('Ctrl Pts',(0.173090695383619,1.,-1.91511429159681));
#36034=CARTESIAN_POINT('Ctrl Pts',(0.172321621259557,-1.,-1.92122334398034));
#36035=CARTESIAN_POINT('Ctrl Pts',(0.172321621259557,1.,-1.92122334398034));
#36036=CARTESIAN_POINT('Ctrl Pts',(0.17147119153296,-1.,-1.92731093582));
#36037=CARTESIAN_POINT('Ctrl Pts',(0.17147119153296,1.,-1.92731093582));
#36038=CARTESIAN_POINT('Ctrl Pts',(0.170541253116136,-1.,-1.93329183155455));
#36039=CARTESIAN_POINT('Ctrl Pts',(0.170541253116136,1.,-1.93329183155455));
#36040=CARTESIAN_POINT('Ctrl Pts',(0.169534904817425,-1.,-1.93915639211497));
#36041=CARTESIAN_POINT('Ctrl Pts',(0.169534904817425,1.,-1.93915639211497));
#36042=CARTESIAN_POINT('Ctrl Pts',(0.168455741607516,-1.,-1.94493757756879));
#36043=CARTESIAN_POINT('Ctrl Pts',(0.168455741607516,1.,-1.94493757756879));
#36044=CARTESIAN_POINT('Ctrl Pts',(0.167307501784469,-1.,-1.95069027794286));
#36045=CARTESIAN_POINT('Ctrl Pts',(0.167307501784469,1.,-1.95069027794286));
#36046=CARTESIAN_POINT('Ctrl Pts',(0.166093592002833,-1.,-1.95646759718755));
#36047=CARTESIAN_POINT('Ctrl Pts',(0.166093592002833,1.,-1.95646759718755));
#36048=CARTESIAN_POINT('Ctrl Pts',(0.1648165689203,-1.,-1.96229379940174));
#36049=CARTESIAN_POINT('Ctrl Pts',(0.1648165689203,1.,-1.96229379940174));
#36050=CARTESIAN_POINT('Ctrl Pts',(0.16347818545776,-1.,-1.96816512678));
#36051=CARTESIAN_POINT('Ctrl Pts',(0.16347818545776,1.,-1.96816512678));
#36052=CARTESIAN_POINT('Ctrl Pts',(0.162079693556302,-1.,-1.97406280235204));
#36053=CARTESIAN_POINT('Ctrl Pts',(0.162079693556302,1.,-1.97406280235204));
#36054=CARTESIAN_POINT('Ctrl Pts',(0.16062206078461,-1.,-1.97996195437557));
#36055=CARTESIAN_POINT('Ctrl Pts',(0.16062206078461,1.,-1.97996195437557));
#36056=CARTESIAN_POINT('Ctrl Pts',(0.159106226437288,-1.,-1.98584238283279));
#36057=CARTESIAN_POINT('Ctrl Pts',(0.159106226437288,1.,-1.98584238283279));
#36058=CARTESIAN_POINT('Ctrl Pts',(0.157533331459215,-1.,-1.99169810931893));
#36059=CARTESIAN_POINT('Ctrl Pts',(0.157533331459215,1.,-1.99169810931893));
#36060=CARTESIAN_POINT('Ctrl Pts',(0.155904629548774,-1.,-1.99753284771487));
#36061=CARTESIAN_POINT('Ctrl Pts',(0.155904629548774,1.,-1.99753284771487));
#36062=CARTESIAN_POINT('Ctrl Pts',(0.154221403049719,-1.,-2.00335565310539));
#36063=CARTESIAN_POINT('Ctrl Pts',(0.154221403049719,1.,-2.00335565310539));
#36064=CARTESIAN_POINT('Ctrl Pts',(0.152484883621452,-1.,-2.00917680318426));
#36065=CARTESIAN_POINT('Ctrl Pts',(0.152484883621452,1.,-2.00917680318426));
#36066=CARTESIAN_POINT('Ctrl Pts',(0.150696157673084,-1.,-2.01500291940243));
#36067=CARTESIAN_POINT('Ctrl Pts',(0.150696157673084,1.,-2.01500291940243));
#36068=CARTESIAN_POINT('Ctrl Pts',(0.148856124775343,-1.,-2.02083464969897));
#36069=CARTESIAN_POINT('Ctrl Pts',(0.148856124775343,1.,-2.02083464969897));
#36070=CARTESIAN_POINT('Ctrl Pts',(0.146965557332586,-1.,-2.02666926182017));
#36071=CARTESIAN_POINT('Ctrl Pts',(0.146965557332586,1.,-2.02666926182017));
#36072=CARTESIAN_POINT('Ctrl Pts',(0.145025140186058,-1.,-2.03250223739941));
#36073=CARTESIAN_POINT('Ctrl Pts',(0.145025140186058,1.,-2.03250223739941));
#36074=CARTESIAN_POINT('Ctrl Pts',(0.143035515058208,-1.,-2.03832911025913));
#36075=CARTESIAN_POINT('Ctrl Pts',(0.143035515058208,1.,-2.03832911025913));
#36076=CARTESIAN_POINT('Ctrl Pts',(0.140997332152545,-1.,-2.04414757947919));
#36077=CARTESIAN_POINT('Ctrl Pts',(0.140997332152545,1.,-2.04414757947919));
#36078=CARTESIAN_POINT('Ctrl Pts',(0.138911255368966,-1.,-2.04995762001333));
#36079=CARTESIAN_POINT('Ctrl Pts',(0.138911255368966,1.,-2.04995762001333));
#36080=CARTESIAN_POINT('Ctrl Pts',(0.136777941218044,-1.,-2.0557604441427));
#36081=CARTESIAN_POINT('Ctrl Pts',(0.136777941218044,1.,-2.0557604441427));
#36082=CARTESIAN_POINT('Ctrl Pts',(0.134598026192107,-1.,-2.06155781517844));
#36083=CARTESIAN_POINT('Ctrl Pts',(0.134598026192107,1.,-2.06155781517844));
#36084=CARTESIAN_POINT('Ctrl Pts',(0.13237211154771,-1.,-2.06735123910319));
#36085=CARTESIAN_POINT('Ctrl Pts',(0.13237211154771,1.,-2.06735123910319));
#36086=CARTESIAN_POINT('Ctrl Pts',(0.1301007483284,-1.,-2.07314114713047));
#36087=CARTESIAN_POINT('Ctrl Pts',(0.1301007483284,1.,-2.07314114713047));
#36088=CARTESIAN_POINT('Ctrl Pts',(0.127784445276116,-1.,-2.07892715110967));
#36089=CARTESIAN_POINT('Ctrl Pts',(0.127784445276116,1.,-2.07892715110967));
#36090=CARTESIAN_POINT('Ctrl Pts',(0.125423679412058,-1.,-2.08470840653628));
#36091=CARTESIAN_POINT('Ctrl Pts',(0.125423679412058,1.,-2.08470840653628));
#36092=CARTESIAN_POINT('Ctrl Pts',(0.123018905621083,-1.,-2.09048392424826));
#36093=CARTESIAN_POINT('Ctrl Pts',(0.123018905621083,1.,-2.09048392424826));
#36094=CARTESIAN_POINT('Ctrl Pts',(0.120570567965129,-1.,-2.09625292867756));
#36095=CARTESIAN_POINT('Ctrl Pts',(0.120570567965129,1.,-2.09625292867756));
#36096=CARTESIAN_POINT('Ctrl Pts',(0.118079107988368,-1.,-2.10201512132945));
#36097=CARTESIAN_POINT('Ctrl Pts',(0.118079107988368,1.,-2.10201512132945));
#36098=CARTESIAN_POINT('Ctrl Pts',(0.11554495768794,-1.,-2.10777050261359));
#36099=CARTESIAN_POINT('Ctrl Pts',(0.11554495768794,1.,-2.10777050261359));
#36100=CARTESIAN_POINT('Ctrl Pts',(0.112968534419746,-1.,-2.11351924490335));
#36101=CARTESIAN_POINT('Ctrl Pts',(0.112968534419746,1.,-2.11351924490335));
#36102=CARTESIAN_POINT('Ctrl Pts',(0.11035023613502,-1.,-2.11926155590849));
#36103=CARTESIAN_POINT('Ctrl Pts',(0.11035023613502,1.,-2.11926155590849));
#36104=CARTESIAN_POINT('Ctrl Pts',(0.107690435231068,-1.,-2.12499752306927));
#36105=CARTESIAN_POINT('Ctrl Pts',(0.107690435231068,1.,-2.12499752306927));
#36106=CARTESIAN_POINT('Ctrl Pts',(0.104989479152703,-1.,-2.1307270488718));
#36107=CARTESIAN_POINT('Ctrl Pts',(0.104989479152703,1.,-2.1307270488718));
#36108=CARTESIAN_POINT('Ctrl Pts',(0.102247700556064,-1.,-2.13644992667052));
#36109=CARTESIAN_POINT('Ctrl Pts',(0.102247700556064,1.,-2.13644992667052));
#36110=CARTESIAN_POINT('Ctrl Pts',(0.0994654261990743,-1.,-2.14216588395974));
#36111=CARTESIAN_POINT('Ctrl Pts',(0.0994654261990743,1.,-2.14216588395974));
#36112=CARTESIAN_POINT('Ctrl Pts',(0.0966429852305689,-1.,-2.14787463531864));
#36113=CARTESIAN_POINT('Ctrl Pts',(0.0966429852305689,1.,-2.14787463531864));
#36114=CARTESIAN_POINT('Ctrl Pts',(0.0937807218868345,-1.,-2.15357593978377));
#36115=CARTESIAN_POINT('Ctrl Pts',(0.0937807218868345,1.,-2.15357593978377));
#36116=CARTESIAN_POINT('Ctrl Pts',(0.0908789888108266,-1.,-2.15926961544808));
#36117=CARTESIAN_POINT('Ctrl Pts',(0.0908789888108266,1.,-2.15926961544808));
#36118=CARTESIAN_POINT('Ctrl Pts',(0.0879381291387823,-1.,-2.16495552645275));
#36119=CARTESIAN_POINT('Ctrl Pts',(0.0879381291387823,1.,-2.16495552645275));
#36120=CARTESIAN_POINT('Ctrl Pts',(0.0849584620835643,-1.,-2.17063357871031));
#36121=CARTESIAN_POINT('Ctrl Pts',(0.0849584620835643,1.,-2.17063357871031));
#36122=CARTESIAN_POINT('Ctrl Pts',(0.0819402680871939,-1.,-2.1763037121106));
#36123=CARTESIAN_POINT('Ctrl Pts',(0.0819402680871939,1.,-2.1763037121106));
#36124=CARTESIAN_POINT('Ctrl Pts',(0.0788837727683228,-1.,-2.18196589448304));
#36125=CARTESIAN_POINT('Ctrl Pts',(0.0788837727683228,1.,-2.18196589448304));
#36126=CARTESIAN_POINT('Ctrl Pts',(0.0757891465833411,-1.,-2.1876201139874));
#36127=CARTESIAN_POINT('Ctrl Pts',(0.0757891465833411,1.,-2.1876201139874));
#36128=CARTESIAN_POINT('Ctrl Pts',(0.0732830357304276,-1.,-2.19213712012956));
#36129=CARTESIAN_POINT('Ctrl Pts',(0.0732830357304276,1.,-2.19213712012956));
#36130=CARTESIAN_POINT('Ctrl Pts',(0.0713863779524627,-1.,-2.19552129483562));
#36131=CARTESIAN_POINT('Ctrl Pts',(0.0713863779524627,1.,-2.19552129483562));
#36132=CARTESIAN_POINT('Ctrl Pts',(0.0701143536324926,-1.,-2.19777582085261));
#36133=CARTESIAN_POINT('Ctrl Pts',(0.0701143536324926,1.,-2.19777582085261));
#36134=CARTESIAN_POINT('Ctrl Pts',(0.0694764450219584,-1.,-2.19890268624765));
#36135=CARTESIAN_POINT('Ctrl Pts',(0.0694764450219584,1.,-2.19890268624765));
#36136=CARTESIAN_POINT('',(0.163289472382896,1.,-1.74236521665491));
#36137=CARTESIAN_POINT('Ctrl Pts',(0.163289472382896,1.,-1.74236521665491));
#36138=CARTESIAN_POINT('Ctrl Pts',(0.163814161002474,1.,-1.74720349503904));
#36139=CARTESIAN_POINT('Ctrl Pts',(0.164834765708484,1.,-1.75666056640041));
#36140=CARTESIAN_POINT('Ctrl Pts',(0.166279355148738,1.,-1.77018771687692));
#36141=CARTESIAN_POINT('Ctrl Pts',(0.16803277280837,1.,-1.78690649988931));
#36142=CARTESIAN_POINT('Ctrl Pts',(0.169936923908078,1.,-1.80561530633924));
#36143=CARTESIAN_POINT('Ctrl Pts',(0.171554770207306,1.,-1.82215766815414));
#36144=CARTESIAN_POINT('Ctrl Pts',(0.17288944289442,1.,-1.83658380530747));
#36145=CARTESIAN_POINT('Ctrl Pts',(0.173946627589401,1.,-1.84898113200543));
#36146=CARTESIAN_POINT('Ctrl Pts',(0.174735259276856,1.,-1.85948367089838));
#36147=CARTESIAN_POINT('Ctrl Pts',(0.175268337590901,1.,-1.86828349694972));
#36148=CARTESIAN_POINT('Ctrl Pts',(0.175563480746205,1.,-1.87563767773249));
#36149=CARTESIAN_POINT('Ctrl Pts',(0.175644148889271,1.,-1.88188663144846));
#36150=CARTESIAN_POINT('Ctrl Pts',(0.175538155840286,1.,-1.88742606272818));
#36151=CARTESIAN_POINT('Ctrl Pts',(0.175274276190664,1.,-1.89264630198279));
#36152=CARTESIAN_POINT('Ctrl Pts',(0.174879405091277,1.,-1.89788101117148));
#36153=CARTESIAN_POINT('Ctrl Pts',(0.174375518661222,1.,-1.90335253863003));
#36154=CARTESIAN_POINT('Ctrl Pts',(0.173776635257984,1.,-1.90911693975475));
#36155=CARTESIAN_POINT('Ctrl Pts',(0.173090695383619,1.,-1.91511429159681));
#36156=CARTESIAN_POINT('Ctrl Pts',(0.172321621259557,1.,-1.92122334398034));
#36157=CARTESIAN_POINT('Ctrl Pts',(0.17147119153296,1.,-1.92731093582));
#36158=CARTESIAN_POINT('Ctrl Pts',(0.170541253116136,1.,-1.93329183155455));
#36159=CARTESIAN_POINT('Ctrl Pts',(0.169534904817425,1.,-1.93915639211497));
#36160=CARTESIAN_POINT('Ctrl Pts',(0.168455741607516,1.,-1.94493757756879));
#36161=CARTESIAN_POINT('Ctrl Pts',(0.167307501784469,1.,-1.95069027794286));
#36162=CARTESIAN_POINT('Ctrl Pts',(0.166093592002833,1.,-1.95646759718755));
#36163=CARTESIAN_POINT('Ctrl Pts',(0.1648165689203,1.,-1.96229379940174));
#36164=CARTESIAN_POINT('Ctrl Pts',(0.16347818545776,1.,-1.96816512678));
#36165=CARTESIAN_POINT('Ctrl Pts',(0.162079693556302,1.,-1.97406280235204));
#36166=CARTESIAN_POINT('Ctrl Pts',(0.16062206078461,1.,-1.97996195437557));
#36167=CARTESIAN_POINT('Ctrl Pts',(0.159106226437288,1.,-1.98584238283279));
#36168=CARTESIAN_POINT('Ctrl Pts',(0.157533331459215,1.,-1.99169810931893));
#36169=CARTESIAN_POINT('Ctrl Pts',(0.155904629548774,1.,-1.99753284771487));
#36170=CARTESIAN_POINT('Ctrl Pts',(0.154221403049719,1.,-2.00335565310539));
#36171=CARTESIAN_POINT('Ctrl Pts',(0.152484883621452,1.,-2.00917680318426));
#36172=CARTESIAN_POINT('Ctrl Pts',(0.150696157673084,1.,-2.01500291940243));
#36173=CARTESIAN_POINT('Ctrl Pts',(0.148856124775343,1.,-2.02083464969897));
#36174=CARTESIAN_POINT('Ctrl Pts',(0.146965557332586,1.,-2.02666926182017));
#36175=CARTESIAN_POINT('Ctrl Pts',(0.145025140186058,1.,-2.03250223739941));
#36176=CARTESIAN_POINT('Ctrl Pts',(0.143035515058208,1.,-2.03832911025913));
#36177=CARTESIAN_POINT('Ctrl Pts',(0.140997332152545,1.,-2.04414757947919));
#36178=CARTESIAN_POINT('Ctrl Pts',(0.138911255368966,1.,-2.04995762001333));
#36179=CARTESIAN_POINT('Ctrl Pts',(0.136777941218044,1.,-2.0557604441427));
#36180=CARTESIAN_POINT('Ctrl Pts',(0.134598026192107,1.,-2.06155781517844));
#36181=CARTESIAN_POINT('Ctrl Pts',(0.13237211154771,1.,-2.06735123910319));
#36182=CARTESIAN_POINT('Ctrl Pts',(0.1301007483284,1.,-2.07314114713047));
#36183=CARTESIAN_POINT('Ctrl Pts',(0.127784445276116,1.,-2.07892715110967));
#36184=CARTESIAN_POINT('Ctrl Pts',(0.125423679412058,1.,-2.08470840653628));
#36185=CARTESIAN_POINT('Ctrl Pts',(0.123018905621083,1.,-2.09048392424826));
#36186=CARTESIAN_POINT('Ctrl Pts',(0.120570567965129,1.,-2.09625292867756));
#36187=CARTESIAN_POINT('Ctrl Pts',(0.118079107988368,1.,-2.10201512132945));
#36188=CARTESIAN_POINT('Ctrl Pts',(0.11554495768794,1.,-2.10777050261359));
#36189=CARTESIAN_POINT('Ctrl Pts',(0.112968534419746,1.,-2.11351924490335));
#36190=CARTESIAN_POINT('Ctrl Pts',(0.11035023613502,1.,-2.11926155590849));
#36191=CARTESIAN_POINT('Ctrl Pts',(0.107690435231068,1.,-2.12499752306927));
#36192=CARTESIAN_POINT('Ctrl Pts',(0.104989479152703,1.,-2.1307270488718));
#36193=CARTESIAN_POINT('Ctrl Pts',(0.102247700556064,1.,-2.13644992667052));
#36194=CARTESIAN_POINT('Ctrl Pts',(0.0994654261990743,1.,-2.14216588395974));
#36195=CARTESIAN_POINT('Ctrl Pts',(0.0966429852305689,1.,-2.14787463531864));
#36196=CARTESIAN_POINT('Ctrl Pts',(0.0937807218868345,1.,-2.15357593978377));
#36197=CARTESIAN_POINT('Ctrl Pts',(0.0908789888108266,1.,-2.15926961544808));
#36198=CARTESIAN_POINT('Ctrl Pts',(0.0879381291387823,1.,-2.16495552645275));
#36199=CARTESIAN_POINT('Ctrl Pts',(0.0849584620835643,1.,-2.17063357871031));
#36200=CARTESIAN_POINT('Ctrl Pts',(0.0819402680871939,1.,-2.1763037121106));
#36201=CARTESIAN_POINT('Ctrl Pts',(0.0788837727683228,1.,-2.18196589448304));
#36202=CARTESIAN_POINT('Ctrl Pts',(0.0757891465833411,1.,-2.1876201139874));
#36203=CARTESIAN_POINT('Ctrl Pts',(0.0732830357304276,1.,-2.19213712012956));
#36204=CARTESIAN_POINT('Ctrl Pts',(0.0713863779524627,1.,-2.19552129483562));
#36205=CARTESIAN_POINT('Ctrl Pts',(0.0701143536324926,1.,-2.19777582085261));
#36206=CARTESIAN_POINT('Ctrl Pts',(0.0694764450219584,1.,-2.19890268624765));
#36207=CARTESIAN_POINT('',(0.163289472382896,0.,-1.74236521665491));
#36208=CARTESIAN_POINT('Origin',(0.,0.,0.));
#36209=CARTESIAN_POINT('',(0.383122945602004,1.,-1.7075470150345));
#36210=CARTESIAN_POINT('Origin',(0.,1.,0.));
#36211=CARTESIAN_POINT('',(0.383122945602004,0.,-1.7075470150345));
#36212=CARTESIAN_POINT('Ctrl Pts',(0.61342227326009,-1.,-2.11275013067528));
#36213=CARTESIAN_POINT('Ctrl Pts',(0.61342227326009,1.,-2.11275013067528));
#36214=CARTESIAN_POINT('Ctrl Pts',(0.61246736556225,-1.,-2.11187554260142));
#36215=CARTESIAN_POINT('Ctrl Pts',(0.61246736556225,1.,-2.11187554260142));
#36216=CARTESIAN_POINT('Ctrl Pts',(0.610560911691113,-1.,-2.11012443807661));
#36217=CARTESIAN_POINT('Ctrl Pts',(0.610560911691113,1.,-2.11012443807661));
#36218=CARTESIAN_POINT('Ctrl Pts',(0.607711315456826,-1.,-2.10749199615859));
#36219=CARTESIAN_POINT('Ctrl Pts',(0.607711315456826,1.,-2.10749199615859));
#36220=CARTESIAN_POINT('Ctrl Pts',(0.603932030738212,-1.,-2.10397049887709));
#36221=CARTESIAN_POINT('Ctrl Pts',(0.603932030738212,1.,-2.10397049887709));
#36222=CARTESIAN_POINT('Ctrl Pts',(0.599241616422144,-1.,-2.09954930865331));
#36223=CARTESIAN_POINT('Ctrl Pts',(0.599241616422144,1.,-2.09954930865331));
#36224=CARTESIAN_POINT('Ctrl Pts',(0.594585006052823,-1.,-2.09510876220501));
#36225=CARTESIAN_POINT('Ctrl Pts',(0.594585006052823,1.,-2.09510876220501));
#36226=CARTESIAN_POINT('Ctrl Pts',(0.589962365403189,-1.,-2.09064881812053));
#36227=CARTESIAN_POINT('Ctrl Pts',(0.589962365403189,1.,-2.09064881812053));
#36228=CARTESIAN_POINT('Ctrl Pts',(0.585373918990895,-1.,-2.086169437277));
#36229=CARTESIAN_POINT('Ctrl Pts',(0.585373918990895,1.,-2.086169437277));
#36230=CARTESIAN_POINT('Ctrl Pts',(0.580819952107256,-1.,-2.08167059018138));
#36231=CARTESIAN_POINT('Ctrl Pts',(0.580819952107256,1.,-2.08167059018138));
#36232=CARTESIAN_POINT('Ctrl Pts',(0.576300797416274,-1.,-2.07715226767361));
#36233=CARTESIAN_POINT('Ctrl Pts',(0.576300797416274,1.,-2.07715226767361));
#36234=CARTESIAN_POINT('Ctrl Pts',(0.571816823242411,-1.,-2.07261449292758));
#36235=CARTESIAN_POINT('Ctrl Pts',(0.571816823242411,1.,-2.07261449292758));
#36236=CARTESIAN_POINT('Ctrl Pts',(0.567368421181229,-1.,-2.06805732997383));
#36237=CARTESIAN_POINT('Ctrl Pts',(0.567368421181229,1.,-2.06805732997383));
#36238=CARTESIAN_POINT('Ctrl Pts',(0.562955993082574,-1.,-2.06348090160697));
#36239=CARTESIAN_POINT('Ctrl Pts',(0.562955993082574,1.,-2.06348090160697));
#36240=CARTESIAN_POINT('Ctrl Pts',(0.558579940185467,-1.,-2.05888537756571));
#36241=CARTESIAN_POINT('Ctrl Pts',(0.558579940185467,1.,-2.05888537756571));
#36242=CARTESIAN_POINT('Ctrl Pts',(0.554240657464109,-1.,-2.05427091604482));
#36243=CARTESIAN_POINT('Ctrl Pts',(0.554240657464109,1.,-2.05427091604482));
#36244=CARTESIAN_POINT('Ctrl Pts',(0.549938525150342,-1.,-2.04963761077974));
#36245=CARTESIAN_POINT('Ctrl Pts',(0.549938525150342,1.,-2.04963761077974));
#36246=CARTESIAN_POINT('Ctrl Pts',(0.545673903817348,-1.,-2.0449854471456));
#36247=CARTESIAN_POINT('Ctrl Pts',(0.545673903817348,1.,-2.0449854471456));
#36248=CARTESIAN_POINT('Ctrl Pts',(0.54144712061552,-1.,-2.0403142269048));
#36249=CARTESIAN_POINT('Ctrl Pts',(0.54144712061552,1.,-2.0403142269048));
#36250=CARTESIAN_POINT('Ctrl Pts',(0.537258489833134,-1.,-2.03562362953993));
#36251=CARTESIAN_POINT('Ctrl Pts',(0.537258489833134,1.,-2.03562362953993));
#36252=CARTESIAN_POINT('Ctrl Pts',(0.533108355132905,-1.,-2.03091336214401));
#36253=CARTESIAN_POINT('Ctrl Pts',(0.533108355132905,1.,-2.03091336214401));
#36254=CARTESIAN_POINT('Ctrl Pts',(0.52899712724191,-1.,-2.02618329083289));
#36255=CARTESIAN_POINT('Ctrl Pts',(0.52899712724191,1.,-2.02618329083289));
#36256=CARTESIAN_POINT('Ctrl Pts',(0.524925318333518,-1.,-2.02143356304712));
#36257=CARTESIAN_POINT('Ctrl Pts',(0.524925318333518,1.,-2.02143356304712));
#36258=CARTESIAN_POINT('Ctrl Pts',(0.520893590399428,-1.,-2.01666477917306));
#36259=CARTESIAN_POINT('Ctrl Pts',(0.520893590399428,1.,-2.01666477917306));
#36260=CARTESIAN_POINT('Ctrl Pts',(0.516902681728733,-1.,-2.01187773939257));
#36261=CARTESIAN_POINT('Ctrl Pts',(0.516902681728733,1.,-2.01187773939257));
#36262=CARTESIAN_POINT('Ctrl Pts',(0.512953306961813,-1.,-2.00707309946955));
#36263=CARTESIAN_POINT('Ctrl Pts',(0.512953306961813,1.,-2.00707309946955));
#36264=CARTESIAN_POINT('Ctrl Pts',(0.509046069886152,-1.,-2.00225107134733));
#36265=CARTESIAN_POINT('Ctrl Pts',(0.509046069886152,1.,-2.00225107134733));
#36266=CARTESIAN_POINT('Ctrl Pts',(0.505181361323011,-1.,-1.99741107463567));
#36267=CARTESIAN_POINT('Ctrl Pts',(0.505181361323011,1.,-1.99741107463567));
#36268=CARTESIAN_POINT('Ctrl Pts',(0.501359287727129,-1.,-1.9925514912615));
#36269=CARTESIAN_POINT('Ctrl Pts',(0.501359287727129,1.,-1.9925514912615));
#36270=CARTESIAN_POINT('Ctrl Pts',(0.497579909545564,-1.,-1.98767044752929));
#36271=CARTESIAN_POINT('Ctrl Pts',(0.497579909545564,1.,-1.98767044752929));
#36272=CARTESIAN_POINT('Ctrl Pts',(0.493843476541492,-1.,-1.9827665876182));
#36273=CARTESIAN_POINT('Ctrl Pts',(0.493843476541492,1.,-1.9827665876182));
#36274=CARTESIAN_POINT('Ctrl Pts',(0.490150627860955,-1.,-1.97783973019229));
#36275=CARTESIAN_POINT('Ctrl Pts',(0.490150627860955,1.,-1.97783973019229));
#36276=CARTESIAN_POINT('Ctrl Pts',(0.486502692907661,-1.,-1.97289186263272));
#36277=CARTESIAN_POINT('Ctrl Pts',(0.486502692907661,1.,-1.97289186263272));
#36278=CARTESIAN_POINT('Ctrl Pts',(0.482901662120686,-1.,-1.96792703422358));
#36279=CARTESIAN_POINT('Ctrl Pts',(0.482901662120686,1.,-1.96792703422358));
#36280=CARTESIAN_POINT('Ctrl Pts',(0.479349583074846,-1.,-1.96294933055938));
#36281=CARTESIAN_POINT('Ctrl Pts',(0.479349583074846,1.,-1.96294933055938));
#36282=CARTESIAN_POINT('Ctrl Pts',(0.475848034683171,-1.,-1.95796111148175));
#36283=CARTESIAN_POINT('Ctrl Pts',(0.475848034683171,1.,-1.95796111148175));
#36284=CARTESIAN_POINT('Ctrl Pts',(0.472397672264079,-1.,-1.95296148278136));
#36285=CARTESIAN_POINT('Ctrl Pts',(0.472397672264079,1.,-1.95296148278136));
#36286=CARTESIAN_POINT('Ctrl Pts',(0.468997482913158,-1.,-1.94794381136524));
#36287=CARTESIAN_POINT('Ctrl Pts',(0.468997482913158,1.,-1.94794381136524));
#36288=CARTESIAN_POINT('Ctrl Pts',(0.465645462026064,-1.,-1.94289794196205));
#36289=CARTESIAN_POINT('Ctrl Pts',(0.465645462026064,1.,-1.94289794196205));
#36290=CARTESIAN_POINT('Ctrl Pts',(0.462340031009087,-1.,-1.93781486640834));
#36291=CARTESIAN_POINT('Ctrl Pts',(0.462340031009087,1.,-1.93781486640834));
#36292=CARTESIAN_POINT('Ctrl Pts',(0.459081234547931,-1.,-1.93269066517936));
#36293=CARTESIAN_POINT('Ctrl Pts',(0.459081234547931,1.,-1.93269066517936));
#36294=CARTESIAN_POINT('Ctrl Pts',(0.455872005174335,-1.,-1.92753067150461));
#36295=CARTESIAN_POINT('Ctrl Pts',(0.455872005174335,1.,-1.92753067150461));
#36296=CARTESIAN_POINT('Ctrl Pts',(0.452719478359356,-1.,-1.9223538064847));
#36297=CARTESIAN_POINT('Ctrl Pts',(0.452719478359356,1.,-1.9223538064847));
#36298=CARTESIAN_POINT('Ctrl Pts',(0.449632260106572,-1.,-1.91718342555717));
#36299=CARTESIAN_POINT('Ctrl Pts',(0.449632260106572,1.,-1.91718342555717));
#36300=CARTESIAN_POINT('Ctrl Pts',(0.446617343485651,-1.,-1.91203699981095));
#36301=CARTESIAN_POINT('Ctrl Pts',(0.446617343485651,1.,-1.91203699981095));
#36302=CARTESIAN_POINT('Ctrl Pts',(0.44367755684917,-1.,-1.90691756144906));
#36303=CARTESIAN_POINT('Ctrl Pts',(0.44367755684917,1.,-1.90691756144906));
#36304=CARTESIAN_POINT('Ctrl Pts',(0.44080783370416,-1.,-1.90180124389137));
#36305=CARTESIAN_POINT('Ctrl Pts',(0.44080783370416,1.,-1.90180124389137));
#36306=CARTESIAN_POINT('Ctrl Pts',(0.437995003948443,-1.,-1.89663648956549));
#36307=CARTESIAN_POINT('Ctrl Pts',(0.437995003948443,1.,-1.89663648956549));
#36308=CARTESIAN_POINT('Ctrl Pts',(0.43522566096358,-1.,-1.89136993975585));
#36309=CARTESIAN_POINT('Ctrl Pts',(0.43522566096358,1.,-1.89136993975585));
#36310=CARTESIAN_POINT('Ctrl Pts',(0.432493038548833,-1.,-1.88596913666828));
#36311=CARTESIAN_POINT('Ctrl Pts',(0.432493038548833,1.,-1.88596913666828));
#36312=CARTESIAN_POINT('Ctrl Pts',(0.429803062482217,-1.,-1.88044229001779));
#36313=CARTESIAN_POINT('Ctrl Pts',(0.429803062482217,1.,-1.88044229001779));
#36314=CARTESIAN_POINT('Ctrl Pts',(0.427183828518743,-1.,-1.87486989291334));
#36315=CARTESIAN_POINT('Ctrl Pts',(0.427183828518743,1.,-1.87486989291334));
#36316=CARTESIAN_POINT('Ctrl Pts',(0.424678177290876,-1.,-1.8693780394412));
#36317=CARTESIAN_POINT('Ctrl Pts',(0.424678177290876,1.,-1.8693780394412));
#36318=CARTESIAN_POINT('Ctrl Pts',(0.422327307417884,-1.,-1.86408083333863));
#36319=CARTESIAN_POINT('Ctrl Pts',(0.422327307417884,1.,-1.86408083333863));
#36320=CARTESIAN_POINT('Ctrl Pts',(0.420157287975583,-1.,-1.8590328109667));
#36321=CARTESIAN_POINT('Ctrl Pts',(0.420157287975583,1.,-1.8590328109667));
#36322=CARTESIAN_POINT('Ctrl Pts',(0.418164129144045,-1.,-1.8541763285645));
#36323=CARTESIAN_POINT('Ctrl Pts',(0.418164129144045,1.,-1.8541763285645));
#36324=CARTESIAN_POINT('Ctrl Pts',(0.416300022039885,-1.,-1.84929312930314));
#36325=CARTESIAN_POINT('Ctrl Pts',(0.416300022039885,1.,-1.84929312930314));
#36326=CARTESIAN_POINT('Ctrl Pts',(0.414487438255542,-1.,-1.84405757074218));
#36327=CARTESIAN_POINT('Ctrl Pts',(0.414487438255542,1.,-1.84405757074218));
#36328=CARTESIAN_POINT('Ctrl Pts',(0.412633125322945,-1.,-1.8380895347617));
#36329=CARTESIAN_POINT('Ctrl Pts',(0.412633125322945,1.,-1.8380895347617));
#36330=CARTESIAN_POINT('Ctrl Pts',(0.410641256301276,-1.,-1.83100408895047));
#36331=CARTESIAN_POINT('Ctrl Pts',(0.410641256301276,1.,-1.83100408895047));
#36332=CARTESIAN_POINT('Ctrl Pts',(0.408428948106227,-1.,-1.82247022677562));
#36333=CARTESIAN_POINT('Ctrl Pts',(0.408428948106227,1.,-1.82247022677562));
#36334=CARTESIAN_POINT('Ctrl Pts',(0.405933518407175,-1.,-1.81223801812013));
#36335=CARTESIAN_POINT('Ctrl Pts',(0.405933518407175,1.,-1.81223801812013));
#36336=CARTESIAN_POINT('Ctrl Pts',(0.403107976163396,-1.,-1.80012077173238));
#36337=CARTESIAN_POINT('Ctrl Pts',(0.403107976163396,1.,-1.80012077173238));
#36338=CARTESIAN_POINT('Ctrl Pts',(0.399919403774155,-1.,-1.78598826343754));
#36339=CARTESIAN_POINT('Ctrl Pts',(0.399919403774155,1.,-1.78598826343754));
#36340=CARTESIAN_POINT('Ctrl Pts',(0.396346196110688,-1.,-1.76975560043442));
#36341=CARTESIAN_POINT('Ctrl Pts',(0.396346196110688,1.,-1.76975560043442));
#36342=CARTESIAN_POINT('Ctrl Pts',(0.392375812285395,-1.,-1.75137405310193));
#36343=CARTESIAN_POINT('Ctrl Pts',(0.392375812285395,1.,-1.75137405310193));
#36344=CARTESIAN_POINT('Ctrl Pts',(0.388877023502615,-1.,-1.73493170972829));
#36345=CARTESIAN_POINT('Ctrl Pts',(0.388877023502615,1.,-1.73493170972829));
#36346=CARTESIAN_POINT('Ctrl Pts',(0.386070790323281,-1.,-1.72162022244582));
#36347=CARTESIAN_POINT('Ctrl Pts',(0.386070790323281,1.,-1.72162022244582));
#36348=CARTESIAN_POINT('Ctrl Pts',(0.384119047314215,-1.,-1.71231062891398));
#36349=CARTESIAN_POINT('Ctrl Pts',(0.384119047314215,1.,-1.71231062891398));
#36350=CARTESIAN_POINT('Ctrl Pts',(0.383122945602004,-1.,-1.7075470150345));
#36351=CARTESIAN_POINT('Ctrl Pts',(0.383122945602004,1.,-1.7075470150345));
#36352=CARTESIAN_POINT('',(0.61342227326009,1.,-2.11275013067528));
#36353=CARTESIAN_POINT('Ctrl Pts',(0.61342227326009,1.,-2.11275013067528));
#36354=CARTESIAN_POINT('Ctrl Pts',(0.61246736556225,1.,-2.11187554260142));
#36355=CARTESIAN_POINT('Ctrl Pts',(0.610560911691113,1.,-2.11012443807661));
#36356=CARTESIAN_POINT('Ctrl Pts',(0.607711315456826,1.,-2.10749199615859));
#36357=CARTESIAN_POINT('Ctrl Pts',(0.603932030738212,1.,-2.10397049887709));
#36358=CARTESIAN_POINT('Ctrl Pts',(0.599241616422144,1.,-2.09954930865331));
#36359=CARTESIAN_POINT('Ctrl Pts',(0.594585006052823,1.,-2.09510876220501));
#36360=CARTESIAN_POINT('Ctrl Pts',(0.589962365403189,1.,-2.09064881812053));
#36361=CARTESIAN_POINT('Ctrl Pts',(0.585373918990895,1.,-2.086169437277));
#36362=CARTESIAN_POINT('Ctrl Pts',(0.580819952107256,1.,-2.08167059018138));
#36363=CARTESIAN_POINT('Ctrl Pts',(0.576300797416274,1.,-2.07715226767361));
#36364=CARTESIAN_POINT('Ctrl Pts',(0.571816823242411,1.,-2.07261449292758));
#36365=CARTESIAN_POINT('Ctrl Pts',(0.567368421181229,1.,-2.06805732997383));
#36366=CARTESIAN_POINT('Ctrl Pts',(0.562955993082574,1.,-2.06348090160697));
#36367=CARTESIAN_POINT('Ctrl Pts',(0.558579940185467,1.,-2.05888537756571));
#36368=CARTESIAN_POINT('Ctrl Pts',(0.554240657464109,1.,-2.05427091604482));
#36369=CARTESIAN_POINT('Ctrl Pts',(0.549938525150342,1.,-2.04963761077974));
#36370=CARTESIAN_POINT('Ctrl Pts',(0.545673903817348,1.,-2.0449854471456));
#36371=CARTESIAN_POINT('Ctrl Pts',(0.54144712061552,1.,-2.0403142269048));
#36372=CARTESIAN_POINT('Ctrl Pts',(0.537258489833134,1.,-2.03562362953993));
#36373=CARTESIAN_POINT('Ctrl Pts',(0.533108355132905,1.,-2.03091336214401));
#36374=CARTESIAN_POINT('Ctrl Pts',(0.52899712724191,1.,-2.02618329083289));
#36375=CARTESIAN_POINT('Ctrl Pts',(0.524925318333518,1.,-2.02143356304712));
#36376=CARTESIAN_POINT('Ctrl Pts',(0.520893590399428,1.,-2.01666477917306));
#36377=CARTESIAN_POINT('Ctrl Pts',(0.516902681728733,1.,-2.01187773939257));
#36378=CARTESIAN_POINT('Ctrl Pts',(0.512953306961813,1.,-2.00707309946955));
#36379=CARTESIAN_POINT('Ctrl Pts',(0.509046069886152,1.,-2.00225107134733));
#36380=CARTESIAN_POINT('Ctrl Pts',(0.505181361323011,1.,-1.99741107463567));
#36381=CARTESIAN_POINT('Ctrl Pts',(0.501359287727129,1.,-1.9925514912615));
#36382=CARTESIAN_POINT('Ctrl Pts',(0.497579909545564,1.,-1.98767044752929));
#36383=CARTESIAN_POINT('Ctrl Pts',(0.493843476541492,1.,-1.9827665876182));
#36384=CARTESIAN_POINT('Ctrl Pts',(0.490150627860955,1.,-1.97783973019229));
#36385=CARTESIAN_POINT('Ctrl Pts',(0.486502692907661,1.,-1.97289186263272));
#36386=CARTESIAN_POINT('Ctrl Pts',(0.482901662120686,1.,-1.96792703422358));
#36387=CARTESIAN_POINT('Ctrl Pts',(0.479349583074846,1.,-1.96294933055938));
#36388=CARTESIAN_POINT('Ctrl Pts',(0.475848034683171,1.,-1.95796111148175));
#36389=CARTESIAN_POINT('Ctrl Pts',(0.472397672264079,1.,-1.95296148278136));
#36390=CARTESIAN_POINT('Ctrl Pts',(0.468997482913158,1.,-1.94794381136524));
#36391=CARTESIAN_POINT('Ctrl Pts',(0.465645462026064,1.,-1.94289794196205));
#36392=CARTESIAN_POINT('Ctrl Pts',(0.462340031009087,1.,-1.93781486640834));
#36393=CARTESIAN_POINT('Ctrl Pts',(0.459081234547931,1.,-1.93269066517936));
#36394=CARTESIAN_POINT('Ctrl Pts',(0.455872005174335,1.,-1.92753067150461));
#36395=CARTESIAN_POINT('Ctrl Pts',(0.452719478359356,1.,-1.9223538064847));
#36396=CARTESIAN_POINT('Ctrl Pts',(0.449632260106572,1.,-1.91718342555717));
#36397=CARTESIAN_POINT('Ctrl Pts',(0.446617343485651,1.,-1.91203699981095));
#36398=CARTESIAN_POINT('Ctrl Pts',(0.44367755684917,1.,-1.90691756144906));
#36399=CARTESIAN_POINT('Ctrl Pts',(0.44080783370416,1.,-1.90180124389137));
#36400=CARTESIAN_POINT('Ctrl Pts',(0.437995003948443,1.,-1.89663648956549));
#36401=CARTESIAN_POINT('Ctrl Pts',(0.43522566096358,1.,-1.89136993975585));
#36402=CARTESIAN_POINT('Ctrl Pts',(0.432493038548833,1.,-1.88596913666828));
#36403=CARTESIAN_POINT('Ctrl Pts',(0.429803062482217,1.,-1.88044229001779));
#36404=CARTESIAN_POINT('Ctrl Pts',(0.427183828518743,1.,-1.87486989291334));
#36405=CARTESIAN_POINT('Ctrl Pts',(0.424678177290876,1.,-1.8693780394412));
#36406=CARTESIAN_POINT('Ctrl Pts',(0.422327307417884,1.,-1.86408083333863));
#36407=CARTESIAN_POINT('Ctrl Pts',(0.420157287975583,1.,-1.8590328109667));
#36408=CARTESIAN_POINT('Ctrl Pts',(0.418164129144045,1.,-1.8541763285645));
#36409=CARTESIAN_POINT('Ctrl Pts',(0.416300022039885,1.,-1.84929312930314));
#36410=CARTESIAN_POINT('Ctrl Pts',(0.414487438255542,1.,-1.84405757074218));
#36411=CARTESIAN_POINT('Ctrl Pts',(0.412633125322945,1.,-1.8380895347617));
#36412=CARTESIAN_POINT('Ctrl Pts',(0.410641256301276,1.,-1.83100408895047));
#36413=CARTESIAN_POINT('Ctrl Pts',(0.408428948106227,1.,-1.82247022677562));
#36414=CARTESIAN_POINT('Ctrl Pts',(0.405933518407175,1.,-1.81223801812013));
#36415=CARTESIAN_POINT('Ctrl Pts',(0.403107976163396,1.,-1.80012077173238));
#36416=CARTESIAN_POINT('Ctrl Pts',(0.399919403774155,1.,-1.78598826343754));
#36417=CARTESIAN_POINT('Ctrl Pts',(0.396346196110688,1.,-1.76975560043442));
#36418=CARTESIAN_POINT('Ctrl Pts',(0.392375812285395,1.,-1.75137405310193));
#36419=CARTESIAN_POINT('Ctrl Pts',(0.388877023502615,1.,-1.73493170972829));
#36420=CARTESIAN_POINT('Ctrl Pts',(0.386070790323281,1.,-1.72162022244582));
#36421=CARTESIAN_POINT('Ctrl Pts',(0.384119047314215,1.,-1.71231062891398));
#36422=CARTESIAN_POINT('Ctrl Pts',(0.383122945602004,1.,-1.7075470150345));
#36423=CARTESIAN_POINT('',(0.61342227326009,0.,-2.11275013067528));
#36424=CARTESIAN_POINT('Origin',(0.745574324794401,0.,-2.0698113262342));
#36425=CARTESIAN_POINT('',(0.745574324794401,1.,-2.0698113262342));
#36426=CARTESIAN_POINT('',(0.61342227326009,1.,-2.11275013067528));
#36427=CARTESIAN_POINT('',(0.745574324794401,0.,-2.0698113262342));
#36428=CARTESIAN_POINT('Ctrl Pts',(0.693717979106306,-1.,-1.60662857109684));
#36429=CARTESIAN_POINT('Ctrl Pts',(0.693717979106306,1.,-1.60662857109684));
#36430=CARTESIAN_POINT('Ctrl Pts',(0.695712097881194,-1.,-1.61106790958151));
#36431=CARTESIAN_POINT('Ctrl Pts',(0.695712097881194,1.,-1.61106790958151));
#36432=CARTESIAN_POINT('Ctrl Pts',(0.699605146405088,-1.,-1.61974673472612));
#36433=CARTESIAN_POINT('Ctrl Pts',(0.699605146405088,1.,-1.61974673472612));
#36434=CARTESIAN_POINT('Ctrl Pts',(0.705159151988319,-1.,-1.63216541664676));
#36435=CARTESIAN_POINT('Ctrl Pts',(0.705159151988319,1.,-1.63216541664676));
#36436=CARTESIAN_POINT('Ctrl Pts',(0.711993139355394,-1.,-1.64752408832016));
#36437=CARTESIAN_POINT('Ctrl Pts',(0.711993139355394,1.,-1.64752408832016));
#36438=CARTESIAN_POINT('Ctrl Pts',(0.719585433804282,-1.,-1.6647288055568));
#36439=CARTESIAN_POINT('Ctrl Pts',(0.719585433804282,1.,-1.6647288055568));
#36440=CARTESIAN_POINT('Ctrl Pts',(0.726235967997433,-1.,-1.67996158455503));
#36441=CARTESIAN_POINT('Ctrl Pts',(0.726235967997433,1.,-1.67996158455503));
#36442=CARTESIAN_POINT('Ctrl Pts',(0.731963238697195,-1.,-1.69326921975743));
#36443=CARTESIAN_POINT('Ctrl Pts',(0.731963238697195,1.,-1.69326921975743));
#36444=CARTESIAN_POINT('Ctrl Pts',(0.736799665724771,-1.,-1.70473309006121));
#36445=CARTESIAN_POINT('Ctrl Pts',(0.736799665724771,1.,-1.70473309006121));
#36446=CARTESIAN_POINT('Ctrl Pts',(0.740795162032087,-1.,-1.71447789751927));
#36447=CARTESIAN_POINT('Ctrl Pts',(0.740795162032087,1.,-1.71447789751927));
#36448=CARTESIAN_POINT('Ctrl Pts',(0.744021445433764,-1.,-1.7226822991693));
#36449=CARTESIAN_POINT('Ctrl Pts',(0.744021445433764,1.,-1.7226822991693));
#36450=CARTESIAN_POINT('Ctrl Pts',(0.746574710096436,-1.,-1.72958533647399));
#36451=CARTESIAN_POINT('Ctrl Pts',(0.746574710096436,1.,-1.72958533647399));
#36452=CARTESIAN_POINT('Ctrl Pts',(0.748582462954854,-1.,-1.73550351679848));
#36453=CARTESIAN_POINT('Ctrl Pts',(0.748582462954854,1.,-1.73550351679848));
#36454=CARTESIAN_POINT('Ctrl Pts',(0.75019343597954,-1.,-1.74080458266705));
#36455=CARTESIAN_POINT('Ctrl Pts',(0.75019343597954,1.,-1.74080458266705));
#36456=CARTESIAN_POINT('Ctrl Pts',(0.751555614163629,-1.,-1.74585086852298));
#36457=CARTESIAN_POINT('Ctrl Pts',(0.751555614163629,1.,-1.74585086852298));
#36458=CARTESIAN_POINT('Ctrl Pts',(0.752797683531377,-1.,-1.75095139468809));
#36459=CARTESIAN_POINT('Ctrl Pts',(0.752797683531377,1.,-1.75095139468809));
#36460=CARTESIAN_POINT('Ctrl Pts',(0.75400925402848,-1.,-1.75631083600175));
#36461=CARTESIAN_POINT('Ctrl Pts',(0.75400925402848,1.,-1.75631083600175));
#36462=CARTESIAN_POINT('Ctrl Pts',(0.755220979975262,-1.,-1.7619781724032));
#36463=CARTESIAN_POINT('Ctrl Pts',(0.755220979975262,1.,-1.7619781724032));
#36464=CARTESIAN_POINT('Ctrl Pts',(0.756421896028403,-1.,-1.76789396003141));
#36465=CARTESIAN_POINT('Ctrl Pts',(0.756421896028403,1.,-1.76789396003141));
#36466=CARTESIAN_POINT('Ctrl Pts',(0.757578264077238,-1.,-1.77394167108342));
#36467=CARTESIAN_POINT('Ctrl Pts',(0.757578264077238,1.,-1.77394167108342));
#36468=CARTESIAN_POINT('Ctrl Pts',(0.75865062667738,-1.,-1.77999411220912));
#36469=CARTESIAN_POINT('Ctrl Pts',(0.75865062667738,1.,-1.77999411220912));
#36470=CARTESIAN_POINT('Ctrl Pts',(0.759614401109868,-1.,-1.78596964884527));
#36471=CARTESIAN_POINT('Ctrl Pts',(0.759614401109868,1.,-1.78596964884527));
#36472=CARTESIAN_POINT('Ctrl Pts',(0.760469555880425,-1.,-1.79185815610802));
#36473=CARTESIAN_POINT('Ctrl Pts',(0.760469555880425,1.,-1.79185815610802));
#36474=CARTESIAN_POINT('Ctrl Pts',(0.761229695230359,-1.,-1.79768986997735));
#36475=CARTESIAN_POINT('Ctrl Pts',(0.761229695230359,1.,-1.79768986997735));
#36476=CARTESIAN_POINT('Ctrl Pts',(0.761915336443515,-1.,-1.80351583877334));
#36477=CARTESIAN_POINT('Ctrl Pts',(0.761915336443515,1.,-1.80351583877334));
#36478=CARTESIAN_POINT('Ctrl Pts',(0.762546129464036,-1.,-1.80938551463989));
#36479=CARTESIAN_POINT('Ctrl Pts',(0.762546129464036,1.,-1.80938551463989));
#36480=CARTESIAN_POINT('Ctrl Pts',(0.763132003836783,-1.,-1.81532118405566));
#36481=CARTESIAN_POINT('Ctrl Pts',(0.763132003836783,1.,-1.81532118405566));
#36482=CARTESIAN_POINT('Ctrl Pts',(0.763673465462854,-1.,-1.82131873145297));
#36483=CARTESIAN_POINT('Ctrl Pts',(0.763673465462854,1.,-1.82131873145297));
#36484=CARTESIAN_POINT('Ctrl Pts',(0.764165902606055,-1.,-1.8273599120008));
#36485=CARTESIAN_POINT('Ctrl Pts',(0.764165902606055,1.,-1.8273599120008));
#36486=CARTESIAN_POINT('Ctrl Pts',(0.764602549687845,-1.,-1.8334207722714));
#36487=CARTESIAN_POINT('Ctrl Pts',(0.764602549687845,1.,-1.8334207722714));
#36488=CARTESIAN_POINT('Ctrl Pts',(0.764978057881687,-1.,-1.83948181064823));
#36489=CARTESIAN_POINT('Ctrl Pts',(0.764978057881687,1.,-1.83948181064823));
#36490=CARTESIAN_POINT('Ctrl Pts',(0.765291664861971,-1.,-1.84553698875911));
#36491=CARTESIAN_POINT('Ctrl Pts',(0.765291664861971,1.,-1.84553698875911));
#36492=CARTESIAN_POINT('Ctrl Pts',(0.765545710619023,-1.,-1.85158945130054));
#36493=CARTESIAN_POINT('Ctrl Pts',(0.765545710619023,1.,-1.85158945130054));
#36494=CARTESIAN_POINT('Ctrl Pts',(0.765744212909305,-1.,-1.85764741390391));
#36495=CARTESIAN_POINT('Ctrl Pts',(0.765744212909305,1.,-1.85764741390391));
#36496=CARTESIAN_POINT('Ctrl Pts',(0.765891519092557,-1.,-1.86372027063315));
#36497=CARTESIAN_POINT('Ctrl Pts',(0.765891519092557,1.,-1.86372027063315));
#36498=CARTESIAN_POINT('Ctrl Pts',(0.765990708546111,-1.,-1.86981398314345));
#36499=CARTESIAN_POINT('Ctrl Pts',(0.765990708546111,1.,-1.86981398314345));
#36500=CARTESIAN_POINT('Ctrl Pts',(0.766042837036759,-1.,-1.87592888967886));
#36501=CARTESIAN_POINT('Ctrl Pts',(0.766042837036759,1.,-1.87592888967886));
#36502=CARTESIAN_POINT('Ctrl Pts',(0.766047794851868,-1.,-1.88206215302561));
#36503=CARTESIAN_POINT('Ctrl Pts',(0.766047794851868,1.,-1.88206215302561));
#36504=CARTESIAN_POINT('Ctrl Pts',(0.76600483706209,-1.,-1.88820926433409));
#36505=CARTESIAN_POINT('Ctrl Pts',(0.76600483706209,1.,-1.88820926433409));
#36506=CARTESIAN_POINT('Ctrl Pts',(0.765913193856979,-1.,-1.89436577771389));
#36507=CARTESIAN_POINT('Ctrl Pts',(0.765913193856979,1.,-1.89436577771389));
#36508=CARTESIAN_POINT('Ctrl Pts',(0.765772772593395,-1.,-1.90052930393599));
#36509=CARTESIAN_POINT('Ctrl Pts',(0.765772772593395,1.,-1.90052930393599));
#36510=CARTESIAN_POINT('Ctrl Pts',(0.765584196937936,-1.,-1.90669961402362));
#36511=CARTESIAN_POINT('Ctrl Pts',(0.765584196937936,1.,-1.90669961402362));
#36512=CARTESIAN_POINT('Ctrl Pts',(0.765348465884739,-1.,-1.91287765805174));
#36513=CARTESIAN_POINT('Ctrl Pts',(0.765348465884739,1.,-1.91287765805174));
#36514=CARTESIAN_POINT('Ctrl Pts',(0.765066729667095,-1.,-1.91906491634197));
#36515=CARTESIAN_POINT('Ctrl Pts',(0.765066729667095,1.,-1.91906491634197));
#36516=CARTESIAN_POINT('Ctrl Pts',(0.764740025488189,-1.,-1.92526263537041));
#36517=CARTESIAN_POINT('Ctrl Pts',(0.764740025488189,1.,-1.92526263537041));
#36518=CARTESIAN_POINT('Ctrl Pts',(0.764369010673889,-1.,-1.93147105496367));
#36519=CARTESIAN_POINT('Ctrl Pts',(0.764369010673889,1.,-1.93147105496367));
#36520=CARTESIAN_POINT('Ctrl Pts',(0.763954049121393,-1.,-1.93768964875867));
#36521=CARTESIAN_POINT('Ctrl Pts',(0.763954049121393,1.,-1.93768964875867));
#36522=CARTESIAN_POINT('Ctrl Pts',(0.76349533353858,-1.,-1.94391746617626));
#36523=CARTESIAN_POINT('Ctrl Pts',(0.76349533353858,1.,-1.94391746617626));
#36524=CARTESIAN_POINT('Ctrl Pts',(0.762992990878774,-1.,-1.95015342590025));
#36525=CARTESIAN_POINT('Ctrl Pts',(0.762992990878774,1.,-1.95015342590025));
#36526=CARTESIAN_POINT('Ctrl Pts',(0.762447203806263,-1.,-1.95639665309893));
#36527=CARTESIAN_POINT('Ctrl Pts',(0.762447203806263,1.,-1.95639665309893));
#36528=CARTESIAN_POINT('Ctrl Pts',(0.761858300014575,-1.,-1.96264672744229));
#36529=CARTESIAN_POINT('Ctrl Pts',(0.761858300014575,1.,-1.96264672744229));
#36530=CARTESIAN_POINT('Ctrl Pts',(0.761226690483986,-1.,-1.96890351582545));
#36531=CARTESIAN_POINT('Ctrl Pts',(0.761226690483986,1.,-1.96890351582545));
#36532=CARTESIAN_POINT('Ctrl Pts',(0.760552825409855,-1.,-1.97516705321521));
#36533=CARTESIAN_POINT('Ctrl Pts',(0.760552825409855,1.,-1.97516705321521));
#36534=CARTESIAN_POINT('Ctrl Pts',(0.759837147452135,-1.,-1.98143741418156));
#36535=CARTESIAN_POINT('Ctrl Pts',(0.759837147452135,1.,-1.98143741418156));
#36536=CARTESIAN_POINT('Ctrl Pts',(0.759080037802242,-1.,-1.98771456680806));
#36537=CARTESIAN_POINT('Ctrl Pts',(0.759080037802242,1.,-1.98771456680806));
#36538=CARTESIAN_POINT('Ctrl Pts',(0.758281796766377,-1.,-1.9939983109871));
#36539=CARTESIAN_POINT('Ctrl Pts',(0.758281796766377,1.,-1.9939983109871));
#36540=CARTESIAN_POINT('Ctrl Pts',(0.757442676862341,-1.,-2.00028834739072));
#36541=CARTESIAN_POINT('Ctrl Pts',(0.757442676862341,1.,-2.00028834739072));
#36542=CARTESIAN_POINT('Ctrl Pts',(0.756562904646496,-1.,-2.00658431587682));
#36543=CARTESIAN_POINT('Ctrl Pts',(0.756562904646496,1.,-2.00658431587682));
#36544=CARTESIAN_POINT('Ctrl Pts',(0.7556427049581,-1.,-2.01288584328149));
#36545=CARTESIAN_POINT('Ctrl Pts',(0.7556427049581,1.,-2.01288584328149));
#36546=CARTESIAN_POINT('Ctrl Pts',(0.75468233072352,-1.,-2.01919259406003));
#36547=CARTESIAN_POINT('Ctrl Pts',(0.75468233072352,1.,-2.01919259406003));
#36548=CARTESIAN_POINT('Ctrl Pts',(0.753682061113765,-1.,-2.02550428623587));
#36549=CARTESIAN_POINT('Ctrl Pts',(0.753682061113765,1.,-2.02550428623587));
#36550=CARTESIAN_POINT('Ctrl Pts',(0.752642180488104,-1.,-2.03182068456467));
#36551=CARTESIAN_POINT('Ctrl Pts',(0.752642180488104,1.,-2.03182068456467));
#36552=CARTESIAN_POINT('Ctrl Pts',(0.751562963361383,-1.,-2.03814160092173));
#36553=CARTESIAN_POINT('Ctrl Pts',(0.751562963361383,1.,-2.03814160092173));
#36554=CARTESIAN_POINT('Ctrl Pts',(0.750444657874758,-1.,-2.04446689147754));
#36555=CARTESIAN_POINT('Ctrl Pts',(0.750444657874758,1.,-2.04446689147754));
#36556=CARTESIAN_POINT('Ctrl Pts',(0.749287468663053,-1.,-2.05079645591606));
#36557=CARTESIAN_POINT('Ctrl Pts',(0.749287468663053,1.,-2.05079645591606));
#36558=CARTESIAN_POINT('Ctrl Pts',(0.748091554181101,-1.,-2.05713023030263));
#36559=CARTESIAN_POINT('Ctrl Pts',(0.748091554181101,1.,-2.05713023030263));
#36560=CARTESIAN_POINT('Ctrl Pts',(0.747103932785504,-1.,-2.06220058927162));
#36561=CARTESIAN_POINT('Ctrl Pts',(0.747103932785504,1.,-2.06220058927162));
#36562=CARTESIAN_POINT('Ctrl Pts',(0.746345871542695,-1.,-2.06600523016401));
#36563=CARTESIAN_POINT('Ctrl Pts',(0.746345871542695,1.,-2.06600523016401));
#36564=CARTESIAN_POINT('Ctrl Pts',(0.74583279137781,-1.,-2.06854248895575));
#36565=CARTESIAN_POINT('Ctrl Pts',(0.74583279137781,1.,-2.06854248895575));
#36566=CARTESIAN_POINT('Ctrl Pts',(0.745574324794401,-1.,-2.0698113262342));
#36567=CARTESIAN_POINT('Ctrl Pts',(0.745574324794401,1.,-2.0698113262342));
#36568=CARTESIAN_POINT('',(0.693717979106306,1.,-1.60662857109684));
#36569=CARTESIAN_POINT('Ctrl Pts',(0.693717979106306,1.,-1.60662857109684));
#36570=CARTESIAN_POINT('Ctrl Pts',(0.695712097881194,1.,-1.61106790958151));
#36571=CARTESIAN_POINT('Ctrl Pts',(0.699605146405088,1.,-1.61974673472612));
#36572=CARTESIAN_POINT('Ctrl Pts',(0.705159151988319,1.,-1.63216541664676));
#36573=CARTESIAN_POINT('Ctrl Pts',(0.711993139355394,1.,-1.64752408832016));
#36574=CARTESIAN_POINT('Ctrl Pts',(0.719585433804282,1.,-1.6647288055568));
#36575=CARTESIAN_POINT('Ctrl Pts',(0.726235967997433,1.,-1.67996158455503));
#36576=CARTESIAN_POINT('Ctrl Pts',(0.731963238697195,1.,-1.69326921975743));
#36577=CARTESIAN_POINT('Ctrl Pts',(0.736799665724771,1.,-1.70473309006121));
#36578=CARTESIAN_POINT('Ctrl Pts',(0.740795162032087,1.,-1.71447789751927));
#36579=CARTESIAN_POINT('Ctrl Pts',(0.744021445433764,1.,-1.7226822991693));
#36580=CARTESIAN_POINT('Ctrl Pts',(0.746574710096436,1.,-1.72958533647399));
#36581=CARTESIAN_POINT('Ctrl Pts',(0.748582462954854,1.,-1.73550351679848));
#36582=CARTESIAN_POINT('Ctrl Pts',(0.75019343597954,1.,-1.74080458266705));
#36583=CARTESIAN_POINT('Ctrl Pts',(0.751555614163629,1.,-1.74585086852298));
#36584=CARTESIAN_POINT('Ctrl Pts',(0.752797683531377,1.,-1.75095139468809));
#36585=CARTESIAN_POINT('Ctrl Pts',(0.75400925402848,1.,-1.75631083600175));
#36586=CARTESIAN_POINT('Ctrl Pts',(0.755220979975262,1.,-1.7619781724032));
#36587=CARTESIAN_POINT('Ctrl Pts',(0.756421896028403,1.,-1.76789396003141));
#36588=CARTESIAN_POINT('Ctrl Pts',(0.757578264077238,1.,-1.77394167108342));
#36589=CARTESIAN_POINT('Ctrl Pts',(0.75865062667738,1.,-1.77999411220912));
#36590=CARTESIAN_POINT('Ctrl Pts',(0.759614401109868,1.,-1.78596964884527));
#36591=CARTESIAN_POINT('Ctrl Pts',(0.760469555880425,1.,-1.79185815610802));
#36592=CARTESIAN_POINT('Ctrl Pts',(0.761229695230359,1.,-1.79768986997735));
#36593=CARTESIAN_POINT('Ctrl Pts',(0.761915336443515,1.,-1.80351583877334));
#36594=CARTESIAN_POINT('Ctrl Pts',(0.762546129464036,1.,-1.80938551463989));
#36595=CARTESIAN_POINT('Ctrl Pts',(0.763132003836783,1.,-1.81532118405566));
#36596=CARTESIAN_POINT('Ctrl Pts',(0.763673465462854,1.,-1.82131873145297));
#36597=CARTESIAN_POINT('Ctrl Pts',(0.764165902606055,1.,-1.8273599120008));
#36598=CARTESIAN_POINT('Ctrl Pts',(0.764602549687845,1.,-1.8334207722714));
#36599=CARTESIAN_POINT('Ctrl Pts',(0.764978057881687,1.,-1.83948181064823));
#36600=CARTESIAN_POINT('Ctrl Pts',(0.765291664861971,1.,-1.84553698875911));
#36601=CARTESIAN_POINT('Ctrl Pts',(0.765545710619023,1.,-1.85158945130054));
#36602=CARTESIAN_POINT('Ctrl Pts',(0.765744212909305,1.,-1.85764741390391));
#36603=CARTESIAN_POINT('Ctrl Pts',(0.765891519092557,1.,-1.86372027063315));
#36604=CARTESIAN_POINT('Ctrl Pts',(0.765990708546111,1.,-1.86981398314345));
#36605=CARTESIAN_POINT('Ctrl Pts',(0.766042837036759,1.,-1.87592888967886));
#36606=CARTESIAN_POINT('Ctrl Pts',(0.766047794851868,1.,-1.88206215302561));
#36607=CARTESIAN_POINT('Ctrl Pts',(0.76600483706209,1.,-1.88820926433409));
#36608=CARTESIAN_POINT('Ctrl Pts',(0.765913193856979,1.,-1.89436577771389));
#36609=CARTESIAN_POINT('Ctrl Pts',(0.765772772593395,1.,-1.90052930393599));
#36610=CARTESIAN_POINT('Ctrl Pts',(0.765584196937936,1.,-1.90669961402362));
#36611=CARTESIAN_POINT('Ctrl Pts',(0.765348465884739,1.,-1.91287765805174));
#36612=CARTESIAN_POINT('Ctrl Pts',(0.765066729667095,1.,-1.91906491634197));
#36613=CARTESIAN_POINT('Ctrl Pts',(0.764740025488189,1.,-1.92526263537041));
#36614=CARTESIAN_POINT('Ctrl Pts',(0.764369010673889,1.,-1.93147105496367));
#36615=CARTESIAN_POINT('Ctrl Pts',(0.763954049121393,1.,-1.93768964875867));
#36616=CARTESIAN_POINT('Ctrl Pts',(0.76349533353858,1.,-1.94391746617626));
#36617=CARTESIAN_POINT('Ctrl Pts',(0.762992990878774,1.,-1.95015342590025));
#36618=CARTESIAN_POINT('Ctrl Pts',(0.762447203806263,1.,-1.95639665309893));
#36619=CARTESIAN_POINT('Ctrl Pts',(0.761858300014575,1.,-1.96264672744229));
#36620=CARTESIAN_POINT('Ctrl Pts',(0.761226690483986,1.,-1.96890351582545));
#36621=CARTESIAN_POINT('Ctrl Pts',(0.760552825409855,1.,-1.97516705321521));
#36622=CARTESIAN_POINT('Ctrl Pts',(0.759837147452135,1.,-1.98143741418156));
#36623=CARTESIAN_POINT('Ctrl Pts',(0.759080037802242,1.,-1.98771456680806));
#36624=CARTESIAN_POINT('Ctrl Pts',(0.758281796766377,1.,-1.9939983109871));
#36625=CARTESIAN_POINT('Ctrl Pts',(0.757442676862341,1.,-2.00028834739072));
#36626=CARTESIAN_POINT('Ctrl Pts',(0.756562904646496,1.,-2.00658431587682));
#36627=CARTESIAN_POINT('Ctrl Pts',(0.7556427049581,1.,-2.01288584328149));
#36628=CARTESIAN_POINT('Ctrl Pts',(0.75468233072352,1.,-2.01919259406003));
#36629=CARTESIAN_POINT('Ctrl Pts',(0.753682061113765,1.,-2.02550428623587));
#36630=CARTESIAN_POINT('Ctrl Pts',(0.752642180488104,1.,-2.03182068456467));
#36631=CARTESIAN_POINT('Ctrl Pts',(0.751562963361383,1.,-2.03814160092173));
#36632=CARTESIAN_POINT('Ctrl Pts',(0.750444657874758,1.,-2.04446689147754));
#36633=CARTESIAN_POINT('Ctrl Pts',(0.749287468663053,1.,-2.05079645591606));
#36634=CARTESIAN_POINT('Ctrl Pts',(0.748091554181101,1.,-2.05713023030263));
#36635=CARTESIAN_POINT('Ctrl Pts',(0.747103932785504,1.,-2.06220058927162));
#36636=CARTESIAN_POINT('Ctrl Pts',(0.746345871542695,1.,-2.06600523016401));
#36637=CARTESIAN_POINT('Ctrl Pts',(0.74583279137781,1.,-2.06854248895575));
#36638=CARTESIAN_POINT('Ctrl Pts',(0.745574324794401,1.,-2.0698113262342));
#36639=CARTESIAN_POINT('',(0.693717979106306,0.,-1.60662857109684));
#36640=CARTESIAN_POINT('Origin',(0.,0.,0.));
#36641=CARTESIAN_POINT('',(0.892032620296855,1.,-1.5055822144029));
#36642=CARTESIAN_POINT('Origin',(0.,1.,0.));
#36643=CARTESIAN_POINT('',(0.892032620296855,0.,-1.5055822144029));
#36644=CARTESIAN_POINT('Ctrl Pts',(1.23627494547115,-1.,-1.81978687191668));
#36645=CARTESIAN_POINT('Ctrl Pts',(1.23627494547115,1.,-1.81978687191668));
#36646=CARTESIAN_POINT('Ctrl Pts',(1.23509651170476,-1.,-1.81925017193666));
#36647=CARTESIAN_POINT('Ctrl Pts',(1.23509651170476,1.,-1.81925017193666));
#36648=CARTESIAN_POINT('Ctrl Pts',(1.2327422452705,-1.,-1.81817389921279));
#36649=CARTESIAN_POINT('Ctrl Pts',(1.2327422452705,1.,-1.81817389921279));
#36650=CARTESIAN_POINT('Ctrl Pts',(1.2292186489137,-1.,-1.8165508718364));
#36651=CARTESIAN_POINT('Ctrl Pts',(1.2292186489137,1.,-1.8165508718364));
#36652=CARTESIAN_POINT('Ctrl Pts',(1.2245361330495,-1.,-1.81436959210434));
#36653=CARTESIAN_POINT('Ctrl Pts',(1.2245361330495,1.,-1.81436959210434));
#36654=CARTESIAN_POINT('Ctrl Pts',(1.21870906103557,-1.,-1.81161420806656));
#36655=CARTESIAN_POINT('Ctrl Pts',(1.21870906103557,1.,-1.81161420806656));
#36656=CARTESIAN_POINT('Ctrl Pts',(1.21290815708314,-1.,-1.80882996917129));
#36657=CARTESIAN_POINT('Ctrl Pts',(1.21290815708314,1.,-1.80882996917129));
#36658=CARTESIAN_POINT('Ctrl Pts',(1.20713356605475,-1.,-1.80601678480707));
#36659=CARTESIAN_POINT('Ctrl Pts',(1.20713356605475,1.,-1.80601678480707));
#36660=CARTESIAN_POINT('Ctrl Pts',(1.20138548938974,-1.,-1.80317454838603));
#36661=CARTESIAN_POINT('Ctrl Pts',(1.20138548938974,1.,-1.80317454838603));
#36662=CARTESIAN_POINT('Ctrl Pts',(1.19566418930242,-1.,-1.80030314369879));
#36663=CARTESIAN_POINT('Ctrl Pts',(1.19566418930242,1.,-1.80030314369879));
#36664=CARTESIAN_POINT('Ctrl Pts',(1.18996997934445,-1.,-1.79740245923478));
#36665=CARTESIAN_POINT('Ctrl Pts',(1.18996997934445,1.,-1.79740245923478));
#36666=CARTESIAN_POINT('Ctrl Pts',(1.18430321697432,-1.,-1.79447240321515));
#36667=CARTESIAN_POINT('Ctrl Pts',(1.18430321697432,1.,-1.79447240321515));
#36668=CARTESIAN_POINT('Ctrl Pts',(1.17866429440809,-1.,-1.79151291552689));
#36669=CARTESIAN_POINT('Ctrl Pts',(1.17866429440809,1.,-1.79151291552689));
#36670=CARTESIAN_POINT('Ctrl Pts',(1.17305363177328,-1.,-1.78852398877617));
#36671=CARTESIAN_POINT('Ctrl Pts',(1.17305363177328,1.,-1.78852398877617));
#36672=CARTESIAN_POINT('Ctrl Pts',(1.16747166312303,-1.,-1.78550566040443));
#36673=CARTESIAN_POINT('Ctrl Pts',(1.16747166312303,1.,-1.78550566040443));
#36674=CARTESIAN_POINT('Ctrl Pts',(1.16191881298499,-1.,-1.78245795881009));
#36675=CARTESIAN_POINT('Ctrl Pts',(1.16191881298499,1.,-1.78245795881009));
#36676=CARTESIAN_POINT('Ctrl Pts',(1.15639547194698,-1.,-1.77938085564275));
#36677=CARTESIAN_POINT('Ctrl Pts',(1.15639547194698,1.,-1.77938085564275));
#36678=CARTESIAN_POINT('Ctrl Pts',(1.15090197841514,-1.,-1.7762742255701));
#36679=CARTESIAN_POINT('Ctrl Pts',(1.15090197841514,1.,-1.7762742255701));
#36680=CARTESIAN_POINT('Ctrl Pts',(1.1454385822692,-1.,-1.77313777896194));
#36681=CARTESIAN_POINT('Ctrl Pts',(1.1454385822692,1.,-1.77313777896194));
#36682=CARTESIAN_POINT('Ctrl Pts',(1.14000548336975,-1.,-1.76997111386769));
#36683=CARTESIAN_POINT('Ctrl Pts',(1.14000548336975,1.,-1.76997111386769));
#36684=CARTESIAN_POINT('Ctrl Pts',(1.1346029180462,-1.,-1.76677384551862));
#36685=CARTESIAN_POINT('Ctrl Pts',(1.1346029180462,1.,-1.76677384551862));
#36686=CARTESIAN_POINT('Ctrl Pts',(1.12923123555075,-1.,-1.7635457196617));
#36687=CARTESIAN_POINT('Ctrl Pts',(1.12923123555075,1.,-1.7635457196617));
#36688=CARTESIAN_POINT('Ctrl Pts',(1.12389096855086,-1.,-1.76028671825096));
#36689=CARTESIAN_POINT('Ctrl Pts',(1.12389096855086,1.,-1.76028671825096));
#36690=CARTESIAN_POINT('Ctrl Pts',(1.11858293216763,-1.,-1.75699720772105));
#36691=CARTESIAN_POINT('Ctrl Pts',(1.11858293216763,1.,-1.75699720772105));
#36692=CARTESIAN_POINT('Ctrl Pts',(1.11330807582551,-1.,-1.7536777209463));
#36693=CARTESIAN_POINT('Ctrl Pts',(1.11330807582551,1.,-1.7536777209463));
#36694=CARTESIAN_POINT('Ctrl Pts',(1.10806728183007,-1.,-1.7503286607592));
#36695=CARTESIAN_POINT('Ctrl Pts',(1.10806728183007,1.,-1.7503286607592));
#36696=CARTESIAN_POINT('Ctrl Pts',(1.10286118991143,-1.,-1.74695004214923));
#36697=CARTESIAN_POINT('Ctrl Pts',(1.10286118991143,1.,-1.74695004214923));
#36698=CARTESIAN_POINT('Ctrl Pts',(1.09768999241225,-1.,-1.74354119236208));
#36699=CARTESIAN_POINT('Ctrl Pts',(1.09768999241225,1.,-1.74354119236208));
#36700=CARTESIAN_POINT('Ctrl Pts',(1.09255329056493,-1.,-1.74010053962247));
#36701=CARTESIAN_POINT('Ctrl Pts',(1.09255329056493,1.,-1.74010053962247));
#36702=CARTESIAN_POINT('Ctrl Pts',(1.08745056285427,-1.,-1.73662628326091));
#36703=CARTESIAN_POINT('Ctrl Pts',(1.08745056285427,1.,-1.73662628326091));
#36704=CARTESIAN_POINT('Ctrl Pts',(1.08238162784749,-1.,-1.73311705663407));
#36705=CARTESIAN_POINT('Ctrl Pts',(1.08238162784749,1.,-1.73311705663407));
#36706=CARTESIAN_POINT('Ctrl Pts',(1.0773470373727,-1.,-1.72957248977424));
#36707=CARTESIAN_POINT('Ctrl Pts',(1.0773470373727,1.,-1.72957248977424));
#36708=CARTESIAN_POINT('Ctrl Pts',(1.07234866990252,-1.,-1.72599406198488));
#36709=CARTESIAN_POINT('Ctrl Pts',(1.07234866990252,1.,-1.72599406198488));
#36710=CARTESIAN_POINT('Ctrl Pts',(1.06738966975462,-1.,-1.72238500928453));
#36711=CARTESIAN_POINT('Ctrl Pts',(1.06738966975462,1.,-1.72238500928453));
#36712=CARTESIAN_POINT('Ctrl Pts',(1.06247324680647,-1.,-1.71874858456904));
#36713=CARTESIAN_POINT('Ctrl Pts',(1.06247324680647,1.,-1.71874858456904));
#36714=CARTESIAN_POINT('Ctrl Pts',(1.05760163192479,-1.,-1.7150865442702));
#36715=CARTESIAN_POINT('Ctrl Pts',(1.05760163192479,1.,-1.7150865442702));
#36716=CARTESIAN_POINT('Ctrl Pts',(1.05277517202855,-1.,-1.71139783543989));
#36717=CARTESIAN_POINT('Ctrl Pts',(1.05277517202855,1.,-1.71139783543989));
#36718=CARTESIAN_POINT('Ctrl Pts',(1.04799085404995,-1.,-1.70767646263649));
#36719=CARTESIAN_POINT('Ctrl Pts',(1.04799085404995,1.,-1.70767646263649));
#36720=CARTESIAN_POINT('Ctrl Pts',(1.04324363334554,-1.,-1.70391338707982));
#36721=CARTESIAN_POINT('Ctrl Pts',(1.04324363334554,1.,-1.70391338707982));
#36722=CARTESIAN_POINT('Ctrl Pts',(1.03852922490789,-1.,-1.70010052930962));
#36723=CARTESIAN_POINT('Ctrl Pts',(1.03852922490789,1.,-1.70010052930962));
#36724=CARTESIAN_POINT('Ctrl Pts',(1.03384646003588,-1.,-1.69623414782771));
#36725=CARTESIAN_POINT('Ctrl Pts',(1.03384646003588,1.,-1.69623414782771));
#36726=CARTESIAN_POINT('Ctrl Pts',(1.02919977579147,-1.,-1.69231840863458));
#36727=CARTESIAN_POINT('Ctrl Pts',(1.02919977579147,1.,-1.69231840863458));
#36728=CARTESIAN_POINT('Ctrl Pts',(1.02460180535255,-1.,-1.68836910178447));
#36729=CARTESIAN_POINT('Ctrl Pts',(1.02460180535255,1.,-1.68836910178447));
#36730=CARTESIAN_POINT('Ctrl Pts',(1.02006795074201,-1.,-1.68440578021706));
#36731=CARTESIAN_POINT('Ctrl Pts',(1.02006795074201,1.,-1.68440578021706));
#36732=CARTESIAN_POINT('Ctrl Pts',(1.01561026162773,-1.,-1.68044289894798));
#36733=CARTESIAN_POINT('Ctrl Pts',(1.01561026162773,1.,-1.68044289894798));
#36734=CARTESIAN_POINT('Ctrl Pts',(1.01123236493511,-1.,-1.67648246776464));
#36735=CARTESIAN_POINT('Ctrl Pts',(1.01123236493511,1.,-1.67648246776464));
#36736=CARTESIAN_POINT('Ctrl Pts',(1.00692206696414,-1.,-1.67250335383293));
#36737=CARTESIAN_POINT('Ctrl Pts',(1.00692206696414,1.,-1.67250335383293));
#36738=CARTESIAN_POINT('Ctrl Pts',(1.00265091003727,-1.,-1.66846059277303));
#36739=CARTESIAN_POINT('Ctrl Pts',(1.00265091003727,1.,-1.66846059277303));
#36740=CARTESIAN_POINT('Ctrl Pts',(0.998389654952757,-1.,-1.66430758030376));
#36741=CARTESIAN_POINT('Ctrl Pts',(0.998389654952757,1.,-1.66430758030376));
#36742=CARTESIAN_POINT('Ctrl Pts',(0.994121836661305,-1.,-1.66001553809947));
#36743=CARTESIAN_POINT('Ctrl Pts',(0.994121836661305,1.,-1.66001553809947));
#36744=CARTESIAN_POINT('Ctrl Pts',(0.989855627854164,-1.,-1.65559044289699));
#36745=CARTESIAN_POINT('Ctrl Pts',(0.989855627854164,1.,-1.65559044289699));
#36746=CARTESIAN_POINT('Ctrl Pts',(0.98564262292082,-1.,-1.65110016612638));
#36747=CARTESIAN_POINT('Ctrl Pts',(0.98564262292082,1.,-1.65110016612638));
#36748=CARTESIAN_POINT('Ctrl Pts',(0.981562530939489,-1.,-1.64665139190656));
#36749=CARTESIAN_POINT('Ctrl Pts',(0.981562530939489,1.,-1.64665139190656));
#36750=CARTESIAN_POINT('Ctrl Pts',(0.977689794119416,-1.,-1.64233990826687));
#36751=CARTESIAN_POINT('Ctrl Pts',(0.977689794119416,1.,-1.64233990826687));
#36752=CARTESIAN_POINT('Ctrl Pts',(0.974066058287418,-1.,-1.63820952658144));
#36753=CARTESIAN_POINT('Ctrl Pts',(0.974066058287418,1.,-1.63820952658144));
#36754=CARTESIAN_POINT('Ctrl Pts',(0.970669715997509,-1.,-1.63420665729798));
#36755=CARTESIAN_POINT('Ctrl Pts',(0.970669715997509,1.,-1.63420665729798));
#36756=CARTESIAN_POINT('Ctrl Pts',(0.967387853230345,-1.,-1.63013849959462));
#36757=CARTESIAN_POINT('Ctrl Pts',(0.967387853230345,1.,-1.63013849959462));
#36758=CARTESIAN_POINT('Ctrl Pts',(0.964046107040535,-1.,-1.62571930670187));
#36759=CARTESIAN_POINT('Ctrl Pts',(0.964046107040535,1.,-1.62571930670187));
#36760=CARTESIAN_POINT('Ctrl Pts',(0.960438326101728,-1.,-1.62061638140221));
#36761=CARTESIAN_POINT('Ctrl Pts',(0.960438326101728,1.,-1.62061638140221));
#36762=CARTESIAN_POINT('Ctrl Pts',(0.95635442292067,-1.,-1.61449324337085));
#36763=CARTESIAN_POINT('Ctrl Pts',(0.95635442292067,1.,-1.61449324337085));
#36764=CARTESIAN_POINT('Ctrl Pts',(0.951613284356035,-1.,-1.60706069896936));
#36765=CARTESIAN_POINT('Ctrl Pts',(0.951613284356035,1.,-1.60706069896936));
#36766=CARTESIAN_POINT('Ctrl Pts',(0.946078063315257,-1.,-1.59810042043673));
#36767=CARTESIAN_POINT('Ctrl Pts',(0.946078063315257,1.,-1.59810042043673));
#36768=CARTESIAN_POINT('Ctrl Pts',(0.939646377893399,-1.,-1.58744937487176));
#36769=CARTESIAN_POINT('Ctrl Pts',(0.939646377893399,1.,-1.58744937487176));
#36770=CARTESIAN_POINT('Ctrl Pts',(0.932246680108685,-1.,-1.57499388382243));
#36771=CARTESIAN_POINT('Ctrl Pts',(0.932246680108685,1.,-1.57499388382243));
#36772=CARTESIAN_POINT('Ctrl Pts',(0.923832188944341,-1.,-1.56065988578893));
#36773=CARTESIAN_POINT('Ctrl Pts',(0.923832188944341,1.,-1.56065988578893));
#36774=CARTESIAN_POINT('Ctrl Pts',(0.914375919026456,-1.,-1.54440491149498));
#36775=CARTESIAN_POINT('Ctrl Pts',(0.914375919026456,1.,-1.54440491149498));
#36776=CARTESIAN_POINT('Ctrl Pts',(0.905967409625651,-1.,-1.52984849887993));
#36777=CARTESIAN_POINT('Ctrl Pts',(0.905967409625651,1.,-1.52984849887993));
#36778=CARTESIAN_POINT('Ctrl Pts',(0.89918504748351,-1.,-1.51805569590094));
#36779=CARTESIAN_POINT('Ctrl Pts',(0.89918504748351,1.,-1.51805569590094));
#36780=CARTESIAN_POINT('Ctrl Pts',(0.894452006964543,-1.,-1.50980486806688));
#36781=CARTESIAN_POINT('Ctrl Pts',(0.894452006964543,1.,-1.50980486806688));
#36782=CARTESIAN_POINT('Ctrl Pts',(0.892032620296855,-1.,-1.5055822144029));
#36783=CARTESIAN_POINT('Ctrl Pts',(0.892032620296855,1.,-1.5055822144029));
#36784=CARTESIAN_POINT('',(1.23627494547115,1.,-1.81978687191668));
#36785=CARTESIAN_POINT('Ctrl Pts',(1.23627494547115,1.,-1.81978687191668));
#36786=CARTESIAN_POINT('Ctrl Pts',(1.23509651170476,1.,-1.81925017193666));
#36787=CARTESIAN_POINT('Ctrl Pts',(1.2327422452705,1.,-1.81817389921279));
#36788=CARTESIAN_POINT('Ctrl Pts',(1.2292186489137,1.,-1.8165508718364));
#36789=CARTESIAN_POINT('Ctrl Pts',(1.2245361330495,1.,-1.81436959210434));
#36790=CARTESIAN_POINT('Ctrl Pts',(1.21870906103557,1.,-1.81161420806656));
#36791=CARTESIAN_POINT('Ctrl Pts',(1.21290815708314,1.,-1.80882996917129));
#36792=CARTESIAN_POINT('Ctrl Pts',(1.20713356605475,1.,-1.80601678480707));
#36793=CARTESIAN_POINT('Ctrl Pts',(1.20138548938974,1.,-1.80317454838603));
#36794=CARTESIAN_POINT('Ctrl Pts',(1.19566418930242,1.,-1.80030314369879));
#36795=CARTESIAN_POINT('Ctrl Pts',(1.18996997934445,1.,-1.79740245923478));
#36796=CARTESIAN_POINT('Ctrl Pts',(1.18430321697432,1.,-1.79447240321515));
#36797=CARTESIAN_POINT('Ctrl Pts',(1.17866429440809,1.,-1.79151291552689));
#36798=CARTESIAN_POINT('Ctrl Pts',(1.17305363177328,1.,-1.78852398877617));
#36799=CARTESIAN_POINT('Ctrl Pts',(1.16747166312303,1.,-1.78550566040443));
#36800=CARTESIAN_POINT('Ctrl Pts',(1.16191881298499,1.,-1.78245795881009));
#36801=CARTESIAN_POINT('Ctrl Pts',(1.15639547194698,1.,-1.77938085564275));
#36802=CARTESIAN_POINT('Ctrl Pts',(1.15090197841514,1.,-1.7762742255701));
#36803=CARTESIAN_POINT('Ctrl Pts',(1.1454385822692,1.,-1.77313777896194));
#36804=CARTESIAN_POINT('Ctrl Pts',(1.14000548336975,1.,-1.76997111386769));
#36805=CARTESIAN_POINT('Ctrl Pts',(1.1346029180462,1.,-1.76677384551862));
#36806=CARTESIAN_POINT('Ctrl Pts',(1.12923123555075,1.,-1.7635457196617));
#36807=CARTESIAN_POINT('Ctrl Pts',(1.12389096855086,1.,-1.76028671825096));
#36808=CARTESIAN_POINT('Ctrl Pts',(1.11858293216763,1.,-1.75699720772105));
#36809=CARTESIAN_POINT('Ctrl Pts',(1.11330807582551,1.,-1.7536777209463));
#36810=CARTESIAN_POINT('Ctrl Pts',(1.10806728183007,1.,-1.7503286607592));
#36811=CARTESIAN_POINT('Ctrl Pts',(1.10286118991143,1.,-1.74695004214923));
#36812=CARTESIAN_POINT('Ctrl Pts',(1.09768999241225,1.,-1.74354119236208));
#36813=CARTESIAN_POINT('Ctrl Pts',(1.09255329056493,1.,-1.74010053962247));
#36814=CARTESIAN_POINT('Ctrl Pts',(1.08745056285427,1.,-1.73662628326091));
#36815=CARTESIAN_POINT('Ctrl Pts',(1.08238162784749,1.,-1.73311705663407));
#36816=CARTESIAN_POINT('Ctrl Pts',(1.0773470373727,1.,-1.72957248977424));
#36817=CARTESIAN_POINT('Ctrl Pts',(1.07234866990252,1.,-1.72599406198488));
#36818=CARTESIAN_POINT('Ctrl Pts',(1.06738966975462,1.,-1.72238500928453));
#36819=CARTESIAN_POINT('Ctrl Pts',(1.06247324680647,1.,-1.71874858456904));
#36820=CARTESIAN_POINT('Ctrl Pts',(1.05760163192479,1.,-1.7150865442702));
#36821=CARTESIAN_POINT('Ctrl Pts',(1.05277517202855,1.,-1.71139783543989));
#36822=CARTESIAN_POINT('Ctrl Pts',(1.04799085404995,1.,-1.70767646263649));
#36823=CARTESIAN_POINT('Ctrl Pts',(1.04324363334554,1.,-1.70391338707982));
#36824=CARTESIAN_POINT('Ctrl Pts',(1.03852922490789,1.,-1.70010052930962));
#36825=CARTESIAN_POINT('Ctrl Pts',(1.03384646003588,1.,-1.69623414782771));
#36826=CARTESIAN_POINT('Ctrl Pts',(1.02919977579147,1.,-1.69231840863458));
#36827=CARTESIAN_POINT('Ctrl Pts',(1.02460180535255,1.,-1.68836910178447));
#36828=CARTESIAN_POINT('Ctrl Pts',(1.02006795074201,1.,-1.68440578021706));
#36829=CARTESIAN_POINT('Ctrl Pts',(1.01561026162773,1.,-1.68044289894798));
#36830=CARTESIAN_POINT('Ctrl Pts',(1.01123236493511,1.,-1.67648246776464));
#36831=CARTESIAN_POINT('Ctrl Pts',(1.00692206696414,1.,-1.67250335383293));
#36832=CARTESIAN_POINT('Ctrl Pts',(1.00265091003727,1.,-1.66846059277303));
#36833=CARTESIAN_POINT('Ctrl Pts',(0.998389654952757,1.,-1.66430758030376));
#36834=CARTESIAN_POINT('Ctrl Pts',(0.994121836661305,1.,-1.66001553809947));
#36835=CARTESIAN_POINT('Ctrl Pts',(0.989855627854164,1.,-1.65559044289699));
#36836=CARTESIAN_POINT('Ctrl Pts',(0.98564262292082,1.,-1.65110016612638));
#36837=CARTESIAN_POINT('Ctrl Pts',(0.981562530939489,1.,-1.64665139190656));
#36838=CARTESIAN_POINT('Ctrl Pts',(0.977689794119416,1.,-1.64233990826687));
#36839=CARTESIAN_POINT('Ctrl Pts',(0.974066058287418,1.,-1.63820952658144));
#36840=CARTESIAN_POINT('Ctrl Pts',(0.970669715997509,1.,-1.63420665729798));
#36841=CARTESIAN_POINT('Ctrl Pts',(0.967387853230345,1.,-1.63013849959462));
#36842=CARTESIAN_POINT('Ctrl Pts',(0.964046107040535,1.,-1.62571930670187));
#36843=CARTESIAN_POINT('Ctrl Pts',(0.960438326101728,1.,-1.62061638140221));
#36844=CARTESIAN_POINT('Ctrl Pts',(0.95635442292067,1.,-1.61449324337085));
#36845=CARTESIAN_POINT('Ctrl Pts',(0.951613284356035,1.,-1.60706069896936));
#36846=CARTESIAN_POINT('Ctrl Pts',(0.946078063315257,1.,-1.59810042043673));
#36847=CARTESIAN_POINT('Ctrl Pts',(0.939646377893399,1.,-1.58744937487176));
#36848=CARTESIAN_POINT('Ctrl Pts',(0.932246680108685,1.,-1.57499388382243));
#36849=CARTESIAN_POINT('Ctrl Pts',(0.923832188944341,1.,-1.56065988578893));
#36850=CARTESIAN_POINT('Ctrl Pts',(0.914375919026456,1.,-1.54440491149498));
#36851=CARTESIAN_POINT('Ctrl Pts',(0.905967409625651,1.,-1.52984849887993));
#36852=CARTESIAN_POINT('Ctrl Pts',(0.89918504748351,1.,-1.51805569590094));
#36853=CARTESIAN_POINT('Ctrl Pts',(0.894452006964543,1.,-1.50980486806688));
#36854=CARTESIAN_POINT('Ctrl Pts',(0.892032620296855,1.,-1.5055822144029));
#36855=CARTESIAN_POINT('',(1.23627494547115,0.,-1.81978687191668));
#36856=CARTESIAN_POINT('Origin',(1.34869019493419,0.,-1.73811241238545));
#36857=CARTESIAN_POINT('',(1.34869019493419,1.,-1.73811241238545));
#36858=CARTESIAN_POINT('',(1.23627494547115,1.,-1.81978687191668));
#36859=CARTESIAN_POINT('',(1.34869019493419,0.,-1.73811241238545));
#36860=CARTESIAN_POINT('Ctrl Pts',(1.15624053661742,-1.,-1.31362392696032));
#36861=CARTESIAN_POINT('Ctrl Pts',(1.15624053661742,1.,-1.31362392696032));
#36862=CARTESIAN_POINT('Ctrl Pts',(1.15950888730809,-1.,-1.31722977216397));
#36863=CARTESIAN_POINT('Ctrl Pts',(1.15950888730809,1.,-1.31722977216397));
#36864=CARTESIAN_POINT('Ctrl Pts',(1.16589330093588,-1.,-1.32428080721772));
#36865=CARTESIAN_POINT('Ctrl Pts',(1.16589330093588,1.,-1.32428080721772));
#36866=CARTESIAN_POINT('Ctrl Pts',(1.17501305789857,-1.,-1.33437539347008));
#36867=CARTESIAN_POINT('Ctrl Pts',(1.17501305789857,1.,-1.33437539347008));
#36868=CARTESIAN_POINT('Ctrl Pts',(1.18625865667441,-1.,-1.34687054001093));
#36869=CARTESIAN_POINT('Ctrl Pts',(1.18625865667441,1.,-1.34687054001093));
#36870=CARTESIAN_POINT('Ctrl Pts',(1.1987959077932,-1.,-1.36088705043885));
#36871=CARTESIAN_POINT('Ctrl Pts',(1.1987959077932,1.,-1.36088705043885));
#36872=CARTESIAN_POINT('Ctrl Pts',(1.20982812925645,-1.,-1.37331915607905));
#36873=CARTESIAN_POINT('Ctrl Pts',(1.20982812925645,1.,-1.37331915607905));
#36874=CARTESIAN_POINT('Ctrl Pts',(1.21938737280852,-1.,-1.38420564527715));
#36875=CARTESIAN_POINT('Ctrl Pts',(1.21938737280852,1.,-1.38420564527715));
#36876=CARTESIAN_POINT('Ctrl Pts',(1.22752961899387,-1.,-1.39361389568796));
#36877=CARTESIAN_POINT('Ctrl Pts',(1.22752961899387,1.,-1.39361389568796));
#36878=CARTESIAN_POINT('Ctrl Pts',(1.23434087290423,-1.,-1.40164708206106));
#36879=CARTESIAN_POINT('Ctrl Pts',(1.23434087290423,1.,-1.40164708206106));
#36880=CARTESIAN_POINT('Ctrl Pts',(1.23994455029534,-1.,-1.40845295531283));
#36881=CARTESIAN_POINT('Ctrl Pts',(1.23994455029534,1.,-1.40845295531283));
#36882=CARTESIAN_POINT('Ctrl Pts',(1.24450600513056,-1.,-1.41422913175179));
#36883=CARTESIAN_POINT('Ctrl Pts',(1.24450600513056,1.,-1.41422913175179));
#36884=CARTESIAN_POINT('Ctrl Pts',(1.24824430986571,-1.,-1.41923722596025));
#36885=CARTESIAN_POINT('Ctrl Pts',(1.24824430986571,1.,-1.41923722596025));
#36886=CARTESIAN_POINT('Ctrl Pts',(1.2514145557001,-1.,-1.42378102115575));
#36887=CARTESIAN_POINT('Ctrl Pts',(1.2514145557001,1.,-1.42378102115575));
#36888=CARTESIAN_POINT('Ctrl Pts',(1.25426945222639,-1.,-1.42815938799387));
#36889=CARTESIAN_POINT('Ctrl Pts',(1.25426945222639,1.,-1.42815938799387));
#36890=CARTESIAN_POINT('Ctrl Pts',(1.25702687965755,-1.,-1.43262645609691));
#36891=CARTESIAN_POINT('Ctrl Pts',(1.25702687965755,1.,-1.43262645609691));
#36892=CARTESIAN_POINT('Ctrl Pts',(1.25983531012005,-1.,-1.43734919180848));
#36893=CARTESIAN_POINT('Ctrl Pts',(1.25983531012005,1.,-1.43734919180848));
#36894=CARTESIAN_POINT('Ctrl Pts',(1.26273903323858,-1.,-1.44236470511303));
#36895=CARTESIAN_POINT('Ctrl Pts',(1.26273903323858,1.,-1.44236470511303));
#36896=CARTESIAN_POINT('Ctrl Pts',(1.26570925118868,-1.,-1.44761985001662));
#36897=CARTESIAN_POINT('Ctrl Pts',(1.26570925118868,1.,-1.44761985001662));
#36898=CARTESIAN_POINT('Ctrl Pts',(1.2686778680489,-1.,-1.45301422764247));
#36899=CARTESIAN_POINT('Ctrl Pts',(1.2686778680489,1.,-1.45301422764247));
#36900=CARTESIAN_POINT('Ctrl Pts',(1.27156805265289,-1.,-1.45843906294697));
#36901=CARTESIAN_POINT('Ctrl Pts',(1.27156805265289,1.,-1.45843906294697));
#36902=CARTESIAN_POINT('Ctrl Pts',(1.27433119897822,-1.,-1.46382431332476));
#36903=CARTESIAN_POINT('Ctrl Pts',(1.27433119897822,1.,-1.46382431332476));
#36904=CARTESIAN_POINT('Ctrl Pts',(1.27696414831089,-1.,-1.46916035917133));
#36905=CARTESIAN_POINT('Ctrl Pts',(1.27696414831089,1.,-1.46916035917133));
#36906=CARTESIAN_POINT('Ctrl Pts',(1.2794891824849,-1.,-1.4744717526707));
#36907=CARTESIAN_POINT('Ctrl Pts',(1.2794891824849,1.,-1.4744717526707));
#36908=CARTESIAN_POINT('Ctrl Pts',(1.28194158939517,-1.,-1.47980070347096));
#36909=CARTESIAN_POINT('Ctrl Pts',(1.28194158939517,1.,-1.47980070347096));
#36910=CARTESIAN_POINT('Ctrl Pts',(1.28435533880201,-1.,-1.4851881711891));
#36911=CARTESIAN_POINT('Ctrl Pts',(1.28435533880201,1.,-1.4851881711891));
#36912=CARTESIAN_POINT('Ctrl Pts',(1.2867467611644,-1.,-1.4906522831278));
#36913=CARTESIAN_POINT('Ctrl Pts',(1.2867467611644,1.,-1.4906522831278));
#36914=CARTESIAN_POINT('Ctrl Pts',(1.28911506584254,-1.,-1.49618896881754));
#36915=CARTESIAN_POINT('Ctrl Pts',(1.28911506584254,1.,-1.49618896881754));
#36916=CARTESIAN_POINT('Ctrl Pts',(1.29145022885181,-1.,-1.50178230149776));
#36917=CARTESIAN_POINT('Ctrl Pts',(1.29145022885181,1.,-1.50178230149776));
#36918=CARTESIAN_POINT('Ctrl Pts',(1.29373841372842,-1.,-1.50741159078365));
#36919=CARTESIAN_POINT('Ctrl Pts',(1.29373841372842,1.,-1.50741159078365));
#36920=CARTESIAN_POINT('Ctrl Pts',(1.29596850710509,-1.,-1.51305994241402));
#36921=CARTESIAN_POINT('Ctrl Pts',(1.29596850710509,1.,-1.51305994241402));
#36922=CARTESIAN_POINT('Ctrl Pts',(1.29813791800747,-1.,-1.51872184912724));
#36923=CARTESIAN_POINT('Ctrl Pts',(1.29813791800747,1.,-1.51872184912724));
#36924=CARTESIAN_POINT('Ctrl Pts',(1.30024984366328,-1.,-1.52439957861062));
#36925=CARTESIAN_POINT('Ctrl Pts',(1.30024984366328,1.,-1.52439957861062));
#36926=CARTESIAN_POINT('Ctrl Pts',(1.30231064395568,-1.,-1.53009970283891));
#36927=CARTESIAN_POINT('Ctrl Pts',(1.30231064395568,1.,-1.53009970283891));
#36928=CARTESIAN_POINT('Ctrl Pts',(1.30432735639489,-1.,-1.53582981268977));
#36929=CARTESIAN_POINT('Ctrl Pts',(1.30432735639489,1.,-1.53582981268977));
#36930=CARTESIAN_POINT('Ctrl Pts',(1.30630475189556,-1.,-1.54159462645432));
#36931=CARTESIAN_POINT('Ctrl Pts',(1.30630475189556,1.,-1.54159462645432));
#36932=CARTESIAN_POINT('Ctrl Pts',(1.30824393907473,-1.,-1.54739413957185));
#36933=CARTESIAN_POINT('Ctrl Pts',(1.30824393907473,1.,-1.54739413957185));
#36934=CARTESIAN_POINT('Ctrl Pts',(1.31014393684222,-1.,-1.55322568759481));
#36935=CARTESIAN_POINT('Ctrl Pts',(1.31014393684222,1.,-1.55322568759481));
#36936=CARTESIAN_POINT('Ctrl Pts',(1.31200264341696,-1.,-1.55908521254821));
#36937=CARTESIAN_POINT('Ctrl Pts',(1.31200264341696,1.,-1.55908521254821));
#36938=CARTESIAN_POINT('Ctrl Pts',(1.31381795281002,-1.,-1.56496872402353));
#36939=CARTESIAN_POINT('Ctrl Pts',(1.31381795281002,1.,-1.56496872402353));
#36940=CARTESIAN_POINT('Ctrl Pts',(1.31558903860016,-1.,-1.57087397835723));
#36941=CARTESIAN_POINT('Ctrl Pts',(1.31558903860016,1.,-1.57087397835723));
#36942=CARTESIAN_POINT('Ctrl Pts',(1.31731642317187,-1.,-1.5768005650559));
#36943=CARTESIAN_POINT('Ctrl Pts',(1.31731642317187,1.,-1.5768005650559));
#36944=CARTESIAN_POINT('Ctrl Pts',(1.31900135021432,-1.,-1.58274907898834));
#36945=CARTESIAN_POINT('Ctrl Pts',(1.31900135021432,1.,-1.58274907898834));
#36946=CARTESIAN_POINT('Ctrl Pts',(1.32064537110892,-1.,-1.58872057258245));
#36947=CARTESIAN_POINT('Ctrl Pts',(1.32064537110892,1.,-1.58872057258245));
#36948=CARTESIAN_POINT('Ctrl Pts',(1.32224985747682,-1.,-1.59471591079403));
#36949=CARTESIAN_POINT('Ctrl Pts',(1.32224985747682,1.,-1.59471591079403));
#36950=CARTESIAN_POINT('Ctrl Pts',(1.32381550858256,-1.,-1.60073511858687));
#36951=CARTESIAN_POINT('Ctrl Pts',(1.32381550858256,1.,-1.60073511858687));
#36952=CARTESIAN_POINT('Ctrl Pts',(1.32534250785782,-1.,-1.60677758290954));
#36953=CARTESIAN_POINT('Ctrl Pts',(1.32534250785782,1.,-1.60677758290954));
#36954=CARTESIAN_POINT('Ctrl Pts',(1.32683074483356,-1.,-1.6128423401575));
#36955=CARTESIAN_POINT('Ctrl Pts',(1.32683074483356,1.,-1.6128423401575));
#36956=CARTESIAN_POINT('Ctrl Pts',(1.32828000610449,-1.,-1.61892832270724));
#36957=CARTESIAN_POINT('Ctrl Pts',(1.32828000610449,1.,-1.61892832270724));
#36958=CARTESIAN_POINT('Ctrl Pts',(1.3296901950568,-1.,-1.62503464209797));
#36959=CARTESIAN_POINT('Ctrl Pts',(1.3296901950568,1.,-1.62503464209797));
#36960=CARTESIAN_POINT('Ctrl Pts',(1.33106149345645,-1.,-1.63116079730923));
#36961=CARTESIAN_POINT('Ctrl Pts',(1.33106149345645,1.,-1.63116079730923));
#36962=CARTESIAN_POINT('Ctrl Pts',(1.33239425103724,-1.,-1.63730653475089));
#36963=CARTESIAN_POINT('Ctrl Pts',(1.33239425103724,1.,-1.63730653475089));
#36964=CARTESIAN_POINT('Ctrl Pts',(1.33368890676572,-1.,-1.6434717485603));
#36965=CARTESIAN_POINT('Ctrl Pts',(1.33368890676572,1.,-1.6434717485603));
#36966=CARTESIAN_POINT('Ctrl Pts',(1.33494590467993,-1.,-1.6496563728683));
#36967=CARTESIAN_POINT('Ctrl Pts',(1.33494590467993,1.,-1.6496563728683));
#36968=CARTESIAN_POINT('Ctrl Pts',(1.33616559745172,-1.,-1.65586025952593));
#36969=CARTESIAN_POINT('Ctrl Pts',(1.33616559745172,1.,-1.65586025952593));
#36970=CARTESIAN_POINT('Ctrl Pts',(1.33734820885262,-1.,-1.66208312541983));
#36971=CARTESIAN_POINT('Ctrl Pts',(1.33734820885262,1.,-1.66208312541983));
#36972=CARTESIAN_POINT('Ctrl Pts',(1.33849388654388,-1.,-1.66832460783989));
#36973=CARTESIAN_POINT('Ctrl Pts',(1.33849388654388,1.,-1.66832460783989));
#36974=CARTESIAN_POINT('Ctrl Pts',(1.3396027347034,-1.,-1.67458429426086));
#36975=CARTESIAN_POINT('Ctrl Pts',(1.3396027347034,1.,-1.67458429426086));
#36976=CARTESIAN_POINT('Ctrl Pts',(1.34067485185203,-1.,-1.68086176030362));
#36977=CARTESIAN_POINT('Ctrl Pts',(1.34067485185203,1.,-1.68086176030362));
#36978=CARTESIAN_POINT('Ctrl Pts',(1.341710374848,-1.,-1.68715660868764));
#36979=CARTESIAN_POINT('Ctrl Pts',(1.341710374848,1.,-1.68715660868764));
#36980=CARTESIAN_POINT('Ctrl Pts',(1.34270948206319,-1.,-1.6934684849687));
#36981=CARTESIAN_POINT('Ctrl Pts',(1.34270948206319,1.,-1.6934684849687));
#36982=CARTESIAN_POINT('Ctrl Pts',(1.34367237124483,-1.,-1.69979707754427));
#36983=CARTESIAN_POINT('Ctrl Pts',(1.34367237124483,1.,-1.69979707754427));
#36984=CARTESIAN_POINT('Ctrl Pts',(1.34459924533831,-1.,-1.70614212266738));
#36985=CARTESIAN_POINT('Ctrl Pts',(1.34459924533831,1.,-1.70614212266738));
#36986=CARTESIAN_POINT('Ctrl Pts',(1.34549029589416,-1.,-1.71250340686822));
#36987=CARTESIAN_POINT('Ctrl Pts',(1.34549029589416,1.,-1.71250340686822));
#36988=CARTESIAN_POINT('Ctrl Pts',(1.34634568653227,-1.,-1.7188807715049));
#36989=CARTESIAN_POINT('Ctrl Pts',(1.34634568653227,1.,-1.7188807715049));
#36990=CARTESIAN_POINT('Ctrl Pts',(1.34716554819527,-1.,-1.72527410680674));
#36991=CARTESIAN_POINT('Ctrl Pts',(1.34716554819527,1.,-1.72527410680674));
#36992=CARTESIAN_POINT('Ctrl Pts',(1.34779309152035,-1.,-1.7304014965394));
#36993=CARTESIAN_POINT('Ctrl Pts',(1.34779309152035,1.,-1.7304014965394));
#36994=CARTESIAN_POINT('Ctrl Pts',(1.34824783112887,-1.,-1.73425417885907));
#36995=CARTESIAN_POINT('Ctrl Pts',(1.34824783112887,1.,-1.73425417885907));
#36996=CARTESIAN_POINT('Ctrl Pts',(1.34854391898045,-1.,-1.73682580585691));
#36997=CARTESIAN_POINT('Ctrl Pts',(1.34854391898045,1.,-1.73682580585691));
#36998=CARTESIAN_POINT('Ctrl Pts',(1.34869019493419,-1.,-1.73811241238545));
#36999=CARTESIAN_POINT('Ctrl Pts',(1.34869019493419,1.,-1.73811241238545));
#37000=CARTESIAN_POINT('',(1.15624053661742,1.,-1.31362392696032));
#37001=CARTESIAN_POINT('Ctrl Pts',(1.15624053661742,1.,-1.31362392696032));
#37002=CARTESIAN_POINT('Ctrl Pts',(1.15950888730809,1.,-1.31722977216397));
#37003=CARTESIAN_POINT('Ctrl Pts',(1.16589330093588,1.,-1.32428080721772));
#37004=CARTESIAN_POINT('Ctrl Pts',(1.17501305789857,1.,-1.33437539347008));
#37005=CARTESIAN_POINT('Ctrl Pts',(1.18625865667441,1.,-1.34687054001093));
#37006=CARTESIAN_POINT('Ctrl Pts',(1.1987959077932,1.,-1.36088705043885));
#37007=CARTESIAN_POINT('Ctrl Pts',(1.20982812925645,1.,-1.37331915607905));
#37008=CARTESIAN_POINT('Ctrl Pts',(1.21938737280852,1.,-1.38420564527715));
#37009=CARTESIAN_POINT('Ctrl Pts',(1.22752961899387,1.,-1.39361389568796));
#37010=CARTESIAN_POINT('Ctrl Pts',(1.23434087290423,1.,-1.40164708206106));
#37011=CARTESIAN_POINT('Ctrl Pts',(1.23994455029534,1.,-1.40845295531283));
#37012=CARTESIAN_POINT('Ctrl Pts',(1.24450600513056,1.,-1.41422913175179));
#37013=CARTESIAN_POINT('Ctrl Pts',(1.24824430986571,1.,-1.41923722596025));
#37014=CARTESIAN_POINT('Ctrl Pts',(1.2514145557001,1.,-1.42378102115575));
#37015=CARTESIAN_POINT('Ctrl Pts',(1.25426945222639,1.,-1.42815938799387));
#37016=CARTESIAN_POINT('Ctrl Pts',(1.25702687965755,1.,-1.43262645609691));
#37017=CARTESIAN_POINT('Ctrl Pts',(1.25983531012005,1.,-1.43734919180848));
#37018=CARTESIAN_POINT('Ctrl Pts',(1.26273903323858,1.,-1.44236470511303));
#37019=CARTESIAN_POINT('Ctrl Pts',(1.26570925118868,1.,-1.44761985001662));
#37020=CARTESIAN_POINT('Ctrl Pts',(1.2686778680489,1.,-1.45301422764247));
#37021=CARTESIAN_POINT('Ctrl Pts',(1.27156805265289,1.,-1.45843906294697));
#37022=CARTESIAN_POINT('Ctrl Pts',(1.27433119897822,1.,-1.46382431332476));
#37023=CARTESIAN_POINT('Ctrl Pts',(1.27696414831089,1.,-1.46916035917133));
#37024=CARTESIAN_POINT('Ctrl Pts',(1.2794891824849,1.,-1.4744717526707));
#37025=CARTESIAN_POINT('Ctrl Pts',(1.28194158939517,1.,-1.47980070347096));
#37026=CARTESIAN_POINT('Ctrl Pts',(1.28435533880201,1.,-1.4851881711891));
#37027=CARTESIAN_POINT('Ctrl Pts',(1.2867467611644,1.,-1.4906522831278));
#37028=CARTESIAN_POINT('Ctrl Pts',(1.28911506584254,1.,-1.49618896881754));
#37029=CARTESIAN_POINT('Ctrl Pts',(1.29145022885181,1.,-1.50178230149776));
#37030=CARTESIAN_POINT('Ctrl Pts',(1.29373841372842,1.,-1.50741159078365));
#37031=CARTESIAN_POINT('Ctrl Pts',(1.29596850710509,1.,-1.51305994241402));
#37032=CARTESIAN_POINT('Ctrl Pts',(1.29813791800747,1.,-1.51872184912724));
#37033=CARTESIAN_POINT('Ctrl Pts',(1.30024984366328,1.,-1.52439957861062));
#37034=CARTESIAN_POINT('Ctrl Pts',(1.30231064395568,1.,-1.53009970283891));
#37035=CARTESIAN_POINT('Ctrl Pts',(1.30432735639489,1.,-1.53582981268977));
#37036=CARTESIAN_POINT('Ctrl Pts',(1.30630475189556,1.,-1.54159462645432));
#37037=CARTESIAN_POINT('Ctrl Pts',(1.30824393907473,1.,-1.54739413957185));
#37038=CARTESIAN_POINT('Ctrl Pts',(1.31014393684222,1.,-1.55322568759481));
#37039=CARTESIAN_POINT('Ctrl Pts',(1.31200264341696,1.,-1.55908521254821));
#37040=CARTESIAN_POINT('Ctrl Pts',(1.31381795281002,1.,-1.56496872402353));
#37041=CARTESIAN_POINT('Ctrl Pts',(1.31558903860016,1.,-1.57087397835723));
#37042=CARTESIAN_POINT('Ctrl Pts',(1.31731642317187,1.,-1.5768005650559));
#37043=CARTESIAN_POINT('Ctrl Pts',(1.31900135021432,1.,-1.58274907898834));
#37044=CARTESIAN_POINT('Ctrl Pts',(1.32064537110892,1.,-1.58872057258245));
#37045=CARTESIAN_POINT('Ctrl Pts',(1.32224985747682,1.,-1.59471591079403));
#37046=CARTESIAN_POINT('Ctrl Pts',(1.32381550858256,1.,-1.60073511858687));
#37047=CARTESIAN_POINT('Ctrl Pts',(1.32534250785782,1.,-1.60677758290954));
#37048=CARTESIAN_POINT('Ctrl Pts',(1.32683074483356,1.,-1.6128423401575));
#37049=CARTESIAN_POINT('Ctrl Pts',(1.32828000610449,1.,-1.61892832270724));
#37050=CARTESIAN_POINT('Ctrl Pts',(1.3296901950568,1.,-1.62503464209797));
#37051=CARTESIAN_POINT('Ctrl Pts',(1.33106149345645,1.,-1.63116079730923));
#37052=CARTESIAN_POINT('Ctrl Pts',(1.33239425103724,1.,-1.63730653475089));
#37053=CARTESIAN_POINT('Ctrl Pts',(1.33368890676572,1.,-1.6434717485603));
#37054=CARTESIAN_POINT('Ctrl Pts',(1.33494590467993,1.,-1.6496563728683));
#37055=CARTESIAN_POINT('Ctrl Pts',(1.33616559745172,1.,-1.65586025952593));
#37056=CARTESIAN_POINT('Ctrl Pts',(1.33734820885262,1.,-1.66208312541983));
#37057=CARTESIAN_POINT('Ctrl Pts',(1.33849388654388,1.,-1.66832460783989));
#37058=CARTESIAN_POINT('Ctrl Pts',(1.3396027347034,1.,-1.67458429426086));
#37059=CARTESIAN_POINT('Ctrl Pts',(1.34067485185203,1.,-1.68086176030362));
#37060=CARTESIAN_POINT('Ctrl Pts',(1.341710374848,1.,-1.68715660868764));
#37061=CARTESIAN_POINT('Ctrl Pts',(1.34270948206319,1.,-1.6934684849687));
#37062=CARTESIAN_POINT('Ctrl Pts',(1.34367237124483,1.,-1.69979707754427));
#37063=CARTESIAN_POINT('Ctrl Pts',(1.34459924533831,1.,-1.70614212266738));
#37064=CARTESIAN_POINT('Ctrl Pts',(1.34549029589416,1.,-1.71250340686822));
#37065=CARTESIAN_POINT('Ctrl Pts',(1.34634568653227,1.,-1.7188807715049));
#37066=CARTESIAN_POINT('Ctrl Pts',(1.34716554819527,1.,-1.72527410680674));
#37067=CARTESIAN_POINT('Ctrl Pts',(1.34779309152035,1.,-1.7304014965394));
#37068=CARTESIAN_POINT('Ctrl Pts',(1.34824783112887,1.,-1.73425417885907));
#37069=CARTESIAN_POINT('Ctrl Pts',(1.34854391898045,1.,-1.73682580585691));
#37070=CARTESIAN_POINT('Ctrl Pts',(1.34869019493419,1.,-1.73811241238545));
#37071=CARTESIAN_POINT('',(1.15624053661742,0.,-1.31362392696032));
#37072=CARTESIAN_POINT('Origin',(0.,0.,0.));
#37073=CARTESIAN_POINT('',(1.31362392696032,1.,-1.15624053661742));
#37074=CARTESIAN_POINT('Origin',(0.,1.,0.));
#37075=CARTESIAN_POINT('',(1.31362392696032,0.,-1.15624053661742));
#37076=CARTESIAN_POINT('Ctrl Pts',(1.73811241238545,-1.,-1.34869019493419));
#37077=CARTESIAN_POINT('Ctrl Pts',(1.73811241238545,1.,-1.34869019493419));
#37078=CARTESIAN_POINT('Ctrl Pts',(1.73682580585819,-1.,-1.34854391898145));
#37079=CARTESIAN_POINT('Ctrl Pts',(1.73682580585819,1.,-1.34854391898145));
#37080=CARTESIAN_POINT('Ctrl Pts',(1.73425417886254,-1.,-1.34824783113158));
#37081=CARTESIAN_POINT('Ctrl Pts',(1.73425417886254,1.,-1.34824783113158));
#37082=CARTESIAN_POINT('Ctrl Pts',(1.73040149654497,-1.,-1.3477930915247));
#37083=CARTESIAN_POINT('Ctrl Pts',(1.73040149654497,1.,-1.3477930915247));
#37084=CARTESIAN_POINT('Ctrl Pts',(1.72527410681298,-1.,-1.34716554820013));
#37085=CARTESIAN_POINT('Ctrl Pts',(1.72527410681298,1.,-1.34716554820013));
#37086=CARTESIAN_POINT('Ctrl Pts',(1.7188807715095,-1.,-1.34634568653586));
#37087=CARTESIAN_POINT('Ctrl Pts',(1.7188807715095,1.,-1.34634568653586));
#37088=CARTESIAN_POINT('Ctrl Pts',(1.71250340687011,-1.,-1.34549029589563));
#37089=CARTESIAN_POINT('Ctrl Pts',(1.71250340687011,1.,-1.34549029589563));
#37090=CARTESIAN_POINT('Ctrl Pts',(1.70614212266676,-1.,-1.34459924533783));
#37091=CARTESIAN_POINT('Ctrl Pts',(1.70614212266676,1.,-1.34459924533783));
#37092=CARTESIAN_POINT('Ctrl Pts',(1.69979707754221,-1.,-1.34367237124322));
#37093=CARTESIAN_POINT('Ctrl Pts',(1.69979707754221,1.,-1.34367237124322));
#37094=CARTESIAN_POINT('Ctrl Pts',(1.6934684849664,-1.,-1.34270948206139));
#37095=CARTESIAN_POINT('Ctrl Pts',(1.6934684849664,1.,-1.34270948206139));
#37096=CARTESIAN_POINT('Ctrl Pts',(1.68715660868602,-1.,-1.34171037484673));
#37097=CARTESIAN_POINT('Ctrl Pts',(1.68715660868602,1.,-1.34171037484673));
#37098=CARTESIAN_POINT('Ctrl Pts',(1.68086176030308,-1.,-1.3406748518516));
#37099=CARTESIAN_POINT('Ctrl Pts',(1.68086176030308,1.,-1.3406748518516));
#37100=CARTESIAN_POINT('Ctrl Pts',(1.67458429426126,-1.,-1.33960273470372));
#37101=CARTESIAN_POINT('Ctrl Pts',(1.67458429426126,1.,-1.33960273470372));
#37102=CARTESIAN_POINT('Ctrl Pts',(1.66832460784078,-1.,-1.33849388654458));
#37103=CARTESIAN_POINT('Ctrl Pts',(1.66832460784078,1.,-1.33849388654458));
#37104=CARTESIAN_POINT('Ctrl Pts',(1.66208312542073,-1.,-1.33734820885331));
#37105=CARTESIAN_POINT('Ctrl Pts',(1.66208312542073,1.,-1.33734820885331));
#37106=CARTESIAN_POINT('Ctrl Pts',(1.65586025952651,-1.,-1.33616559745217));
#37107=CARTESIAN_POINT('Ctrl Pts',(1.65586025952651,1.,-1.33616559745217));
#37108=CARTESIAN_POINT('Ctrl Pts',(1.64965637286843,-1.,-1.33494590468003));
#37109=CARTESIAN_POINT('Ctrl Pts',(1.64965637286843,1.,-1.33494590468003));
#37110=CARTESIAN_POINT('Ctrl Pts',(1.64347174856007,-1.,-1.33368890676554));
#37111=CARTESIAN_POINT('Ctrl Pts',(1.64347174856007,1.,-1.33368890676554));
#37112=CARTESIAN_POINT('Ctrl Pts',(1.63730653475049,-1.,-1.33239425103694));
#37113=CARTESIAN_POINT('Ctrl Pts',(1.63730653475049,1.,-1.33239425103694));
#37114=CARTESIAN_POINT('Ctrl Pts',(1.63116079730887,-1.,-1.33106149345618));
#37115=CARTESIAN_POINT('Ctrl Pts',(1.63116079730887,1.,-1.33106149345618));
#37116=CARTESIAN_POINT('Ctrl Pts',(1.62503464209777,-1.,-1.32969019505665));
#37117=CARTESIAN_POINT('Ctrl Pts',(1.62503464209777,1.,-1.32969019505665));
#37118=CARTESIAN_POINT('Ctrl Pts',(1.61892832270723,-1.,-1.32828000610448));
#37119=CARTESIAN_POINT('Ctrl Pts',(1.61892832270723,1.,-1.32828000610448));
#37120=CARTESIAN_POINT('Ctrl Pts',(1.61284234015762,-1.,-1.32683074483365));
#37121=CARTESIAN_POINT('Ctrl Pts',(1.61284234015762,1.,-1.32683074483365));
#37122=CARTESIAN_POINT('Ctrl Pts',(1.6067775829097,-1.,-1.32534250785794));
#37123=CARTESIAN_POINT('Ctrl Pts',(1.6067775829097,1.,-1.32534250785794));
#37124=CARTESIAN_POINT('Ctrl Pts',(1.600735118587,-1.,-1.32381550858266));
#37125=CARTESIAN_POINT('Ctrl Pts',(1.600735118587,1.,-1.32381550858266));
#37126=CARTESIAN_POINT('Ctrl Pts',(1.59471591079408,-1.,-1.32224985747686));
#37127=CARTESIAN_POINT('Ctrl Pts',(1.59471591079408,1.,-1.32224985747686));
#37128=CARTESIAN_POINT('Ctrl Pts',(1.58872057258244,-1.,-1.32064537110891));
#37129=CARTESIAN_POINT('Ctrl Pts',(1.58872057258244,1.,-1.32064537110891));
#37130=CARTESIAN_POINT('Ctrl Pts',(1.58274907898829,-1.,-1.31900135021428));
#37131=CARTESIAN_POINT('Ctrl Pts',(1.58274907898829,1.,-1.31900135021428));
#37132=CARTESIAN_POINT('Ctrl Pts',(1.57680056505585,-1.,-1.31731642317183));
#37133=CARTESIAN_POINT('Ctrl Pts',(1.57680056505585,1.,-1.31731642317183));
#37134=CARTESIAN_POINT('Ctrl Pts',(1.57087397835721,-1.,-1.31558903860015));
#37135=CARTESIAN_POINT('Ctrl Pts',(1.57087397835721,1.,-1.31558903860015));
#37136=CARTESIAN_POINT('Ctrl Pts',(1.56496872402352,-1.,-1.31381795281002));
#37137=CARTESIAN_POINT('Ctrl Pts',(1.56496872402352,1.,-1.31381795281002));
#37138=CARTESIAN_POINT('Ctrl Pts',(1.55908521254822,-1.,-1.31200264341696));
#37139=CARTESIAN_POINT('Ctrl Pts',(1.55908521254822,1.,-1.31200264341696));
#37140=CARTESIAN_POINT('Ctrl Pts',(1.55322568759481,-1.,-1.31014393684221));
#37141=CARTESIAN_POINT('Ctrl Pts',(1.55322568759481,1.,-1.31014393684221));
#37142=CARTESIAN_POINT('Ctrl Pts',(1.54739413957183,-1.,-1.30824393907471));
#37143=CARTESIAN_POINT('Ctrl Pts',(1.54739413957183,1.,-1.30824393907471));
#37144=CARTESIAN_POINT('Ctrl Pts',(1.54159462645428,-1.,-1.30630475189553));
#37145=CARTESIAN_POINT('Ctrl Pts',(1.54159462645428,1.,-1.30630475189553));
#37146=CARTESIAN_POINT('Ctrl Pts',(1.53582981268976,-1.,-1.30432735639487));
#37147=CARTESIAN_POINT('Ctrl Pts',(1.53582981268976,1.,-1.30432735639487));
#37148=CARTESIAN_POINT('Ctrl Pts',(1.53009970283893,-1.,-1.3023106439557));
#37149=CARTESIAN_POINT('Ctrl Pts',(1.53009970283893,1.,-1.3023106439557));
#37150=CARTESIAN_POINT('Ctrl Pts',(1.5243995786107,-1.,-1.30024984366334));
#37151=CARTESIAN_POINT('Ctrl Pts',(1.5243995786107,1.,-1.30024984366334));
#37152=CARTESIAN_POINT('Ctrl Pts',(1.51872184912735,-1.,-1.29813791800757));
#37153=CARTESIAN_POINT('Ctrl Pts',(1.51872184912735,1.,-1.29813791800757));
#37154=CARTESIAN_POINT('Ctrl Pts',(1.51305994241412,-1.,-1.29596850710518));
#37155=CARTESIAN_POINT('Ctrl Pts',(1.51305994241412,1.,-1.29596850710518));
#37156=CARTESIAN_POINT('Ctrl Pts',(1.50741159078367,-1.,-1.29373841372843));
#37157=CARTESIAN_POINT('Ctrl Pts',(1.50741159078367,1.,-1.29373841372843));
#37158=CARTESIAN_POINT('Ctrl Pts',(1.50178230149764,-1.,-1.29145022885171));
#37159=CARTESIAN_POINT('Ctrl Pts',(1.50178230149764,1.,-1.29145022885171));
#37160=CARTESIAN_POINT('Ctrl Pts',(1.49618896881729,-1.,-1.28911506584232));
#37161=CARTESIAN_POINT('Ctrl Pts',(1.49618896881729,1.,-1.28911506584232));
#37162=CARTESIAN_POINT('Ctrl Pts',(1.4906522831275,-1.,-1.28674676116415));
#37163=CARTESIAN_POINT('Ctrl Pts',(1.4906522831275,1.,-1.28674676116415));
#37164=CARTESIAN_POINT('Ctrl Pts',(1.48518817118891,-1.,-1.28435533880184));
#37165=CARTESIAN_POINT('Ctrl Pts',(1.48518817118891,1.,-1.28435533880184));
#37166=CARTESIAN_POINT('Ctrl Pts',(1.47980070347102,-1.,-1.28194158939522));
#37167=CARTESIAN_POINT('Ctrl Pts',(1.47980070347102,1.,-1.28194158939522));
#37168=CARTESIAN_POINT('Ctrl Pts',(1.4744717526711,-1.,-1.27948918248524));
#37169=CARTESIAN_POINT('Ctrl Pts',(1.4744717526711,1.,-1.27948918248524));
#37170=CARTESIAN_POINT('Ctrl Pts',(1.46916035917197,-1.,-1.27696414831144));
#37171=CARTESIAN_POINT('Ctrl Pts',(1.46916035917197,1.,-1.27696414831144));
#37172=CARTESIAN_POINT('Ctrl Pts',(1.4638243133254,-1.,-1.27433119897877));
#37173=CARTESIAN_POINT('Ctrl Pts',(1.4638243133254,1.,-1.27433119897877));
#37174=CARTESIAN_POINT('Ctrl Pts',(1.45843906294725,-1.,-1.27156805265312));
#37175=CARTESIAN_POINT('Ctrl Pts',(1.45843906294725,1.,-1.27156805265312));
#37176=CARTESIAN_POINT('Ctrl Pts',(1.45301422764205,-1.,-1.26867786804854));
#37177=CARTESIAN_POINT('Ctrl Pts',(1.45301422764205,1.,-1.26867786804854));
#37178=CARTESIAN_POINT('Ctrl Pts',(1.44761985001544,-1.,-1.26570925118767));
#37179=CARTESIAN_POINT('Ctrl Pts',(1.44761985001544,1.,-1.26570925118767));
#37180=CARTESIAN_POINT('Ctrl Pts',(1.44236470511145,-1.,-1.26273903323723));
#37181=CARTESIAN_POINT('Ctrl Pts',(1.44236470511145,1.,-1.26273903323723));
#37182=CARTESIAN_POINT('Ctrl Pts',(1.43734919180719,-1.,-1.25983531011894));
#37183=CARTESIAN_POINT('Ctrl Pts',(1.43734919180719,1.,-1.25983531011894));
#37184=CARTESIAN_POINT('Ctrl Pts',(1.43262645609679,-1.,-1.25702687965744));
#37185=CARTESIAN_POINT('Ctrl Pts',(1.43262645609679,1.,-1.25702687965744));
#37186=CARTESIAN_POINT('Ctrl Pts',(1.42815938799555,-1.,-1.25426945222783));
#37187=CARTESIAN_POINT('Ctrl Pts',(1.42815938799555,1.,-1.25426945222783));
#37188=CARTESIAN_POINT('Ctrl Pts',(1.42378102115911,-1.,-1.25141455570299));
#37189=CARTESIAN_POINT('Ctrl Pts',(1.42378102115911,1.,-1.25141455570299));
#37190=CARTESIAN_POINT('Ctrl Pts',(1.41923722596421,-1.,-1.24824430986911));
#37191=CARTESIAN_POINT('Ctrl Pts',(1.41923722596421,1.,-1.24824430986911));
#37192=CARTESIAN_POINT('Ctrl Pts',(1.41422913175437,-1.,-1.24450600513278));
#37193=CARTESIAN_POINT('Ctrl Pts',(1.41422913175437,1.,-1.24450600513278));
#37194=CARTESIAN_POINT('Ctrl Pts',(1.40845295531151,-1.,-1.23994455029421));
#37195=CARTESIAN_POINT('Ctrl Pts',(1.40845295531151,1.,-1.23994455029421));
#37196=CARTESIAN_POINT('Ctrl Pts',(1.40164708205345,-1.,-1.23434087289768));
#37197=CARTESIAN_POINT('Ctrl Pts',(1.40164708205345,1.,-1.23434087289768));
#37198=CARTESIAN_POINT('Ctrl Pts',(1.39361389567257,-1.,-1.22752961898063));
#37199=CARTESIAN_POINT('Ctrl Pts',(1.39361389567257,1.,-1.22752961898063));
#37200=CARTESIAN_POINT('Ctrl Pts',(1.38420564525391,-1.,-1.21938737278853));
#37201=CARTESIAN_POINT('Ctrl Pts',(1.38420564525391,1.,-1.21938737278853));
#37202=CARTESIAN_POINT('Ctrl Pts',(1.37331915604962,-1.,-1.20982812923113));
#37203=CARTESIAN_POINT('Ctrl Pts',(1.37331915604962,1.,-1.20982812923113));
#37204=CARTESIAN_POINT('Ctrl Pts',(1.36088705040677,-1.,-1.1987959077656));
#37205=CARTESIAN_POINT('Ctrl Pts',(1.36088705040677,1.,-1.1987959077656));
#37206=CARTESIAN_POINT('Ctrl Pts',(1.34687053998157,-1.,-1.18625865664915));
#37207=CARTESIAN_POINT('Ctrl Pts',(1.34687053998157,1.,-1.18625865664915));
#37208=CARTESIAN_POINT('Ctrl Pts',(1.33437539344842,-1.,-1.17501305787994));
#37209=CARTESIAN_POINT('Ctrl Pts',(1.33437539344842,1.,-1.17501305787994));
#37210=CARTESIAN_POINT('Ctrl Pts',(1.32428080720544,-1.,-1.16589330092532));
#37211=CARTESIAN_POINT('Ctrl Pts',(1.32428080720544,1.,-1.16589330092532));
#37212=CARTESIAN_POINT('Ctrl Pts',(1.3172297721596,-1.,-1.15950888730433));
#37213=CARTESIAN_POINT('Ctrl Pts',(1.3172297721596,1.,-1.15950888730433));
#37214=CARTESIAN_POINT('Ctrl Pts',(1.31362392696032,-1.,-1.15624053661742));
#37215=CARTESIAN_POINT('Ctrl Pts',(1.31362392696032,1.,-1.15624053661742));
#37216=CARTESIAN_POINT('',(1.73811241238545,1.,-1.34869019493419));
#37217=CARTESIAN_POINT('Ctrl Pts',(1.73811241238545,1.,-1.34869019493419));
#37218=CARTESIAN_POINT('Ctrl Pts',(1.73682580585819,1.,-1.34854391898145));
#37219=CARTESIAN_POINT('Ctrl Pts',(1.73425417886254,1.,-1.34824783113158));
#37220=CARTESIAN_POINT('Ctrl Pts',(1.73040149654497,1.,-1.3477930915247));
#37221=CARTESIAN_POINT('Ctrl Pts',(1.72527410681298,1.,-1.34716554820013));
#37222=CARTESIAN_POINT('Ctrl Pts',(1.7188807715095,1.,-1.34634568653586));
#37223=CARTESIAN_POINT('Ctrl Pts',(1.71250340687011,1.,-1.34549029589563));
#37224=CARTESIAN_POINT('Ctrl Pts',(1.70614212266676,1.,-1.34459924533783));
#37225=CARTESIAN_POINT('Ctrl Pts',(1.69979707754221,1.,-1.34367237124322));
#37226=CARTESIAN_POINT('Ctrl Pts',(1.6934684849664,1.,-1.34270948206139));
#37227=CARTESIAN_POINT('Ctrl Pts',(1.68715660868602,1.,-1.34171037484673));
#37228=CARTESIAN_POINT('Ctrl Pts',(1.68086176030308,1.,-1.3406748518516));
#37229=CARTESIAN_POINT('Ctrl Pts',(1.67458429426126,1.,-1.33960273470372));
#37230=CARTESIAN_POINT('Ctrl Pts',(1.66832460784078,1.,-1.33849388654458));
#37231=CARTESIAN_POINT('Ctrl Pts',(1.66208312542073,1.,-1.33734820885331));
#37232=CARTESIAN_POINT('Ctrl Pts',(1.65586025952651,1.,-1.33616559745217));
#37233=CARTESIAN_POINT('Ctrl Pts',(1.64965637286843,1.,-1.33494590468003));
#37234=CARTESIAN_POINT('Ctrl Pts',(1.64347174856007,1.,-1.33368890676554));
#37235=CARTESIAN_POINT('Ctrl Pts',(1.63730653475049,1.,-1.33239425103694));
#37236=CARTESIAN_POINT('Ctrl Pts',(1.63116079730887,1.,-1.33106149345618));
#37237=CARTESIAN_POINT('Ctrl Pts',(1.62503464209777,1.,-1.32969019505665));
#37238=CARTESIAN_POINT('Ctrl Pts',(1.61892832270723,1.,-1.32828000610448));
#37239=CARTESIAN_POINT('Ctrl Pts',(1.61284234015762,1.,-1.32683074483365));
#37240=CARTESIAN_POINT('Ctrl Pts',(1.6067775829097,1.,-1.32534250785794));
#37241=CARTESIAN_POINT('Ctrl Pts',(1.600735118587,1.,-1.32381550858266));
#37242=CARTESIAN_POINT('Ctrl Pts',(1.59471591079408,1.,-1.32224985747686));
#37243=CARTESIAN_POINT('Ctrl Pts',(1.58872057258244,1.,-1.32064537110891));
#37244=CARTESIAN_POINT('Ctrl Pts',(1.58274907898829,1.,-1.31900135021428));
#37245=CARTESIAN_POINT('Ctrl Pts',(1.57680056505585,1.,-1.31731642317183));
#37246=CARTESIAN_POINT('Ctrl Pts',(1.57087397835721,1.,-1.31558903860015));
#37247=CARTESIAN_POINT('Ctrl Pts',(1.56496872402352,1.,-1.31381795281002));
#37248=CARTESIAN_POINT('Ctrl Pts',(1.55908521254822,1.,-1.31200264341696));
#37249=CARTESIAN_POINT('Ctrl Pts',(1.55322568759481,1.,-1.31014393684221));
#37250=CARTESIAN_POINT('Ctrl Pts',(1.54739413957183,1.,-1.30824393907471));
#37251=CARTESIAN_POINT('Ctrl Pts',(1.54159462645428,1.,-1.30630475189553));
#37252=CARTESIAN_POINT('Ctrl Pts',(1.53582981268976,1.,-1.30432735639487));
#37253=CARTESIAN_POINT('Ctrl Pts',(1.53009970283893,1.,-1.3023106439557));
#37254=CARTESIAN_POINT('Ctrl Pts',(1.5243995786107,1.,-1.30024984366334));
#37255=CARTESIAN_POINT('Ctrl Pts',(1.51872184912735,1.,-1.29813791800757));
#37256=CARTESIAN_POINT('Ctrl Pts',(1.51305994241412,1.,-1.29596850710518));
#37257=CARTESIAN_POINT('Ctrl Pts',(1.50741159078367,1.,-1.29373841372843));
#37258=CARTESIAN_POINT('Ctrl Pts',(1.50178230149764,1.,-1.29145022885171));
#37259=CARTESIAN_POINT('Ctrl Pts',(1.49618896881729,1.,-1.28911506584232));
#37260=CARTESIAN_POINT('Ctrl Pts',(1.4906522831275,1.,-1.28674676116415));
#37261=CARTESIAN_POINT('Ctrl Pts',(1.48518817118891,1.,-1.28435533880184));
#37262=CARTESIAN_POINT('Ctrl Pts',(1.47980070347102,1.,-1.28194158939522));
#37263=CARTESIAN_POINT('Ctrl Pts',(1.4744717526711,1.,-1.27948918248524));
#37264=CARTESIAN_POINT('Ctrl Pts',(1.46916035917197,1.,-1.27696414831144));
#37265=CARTESIAN_POINT('Ctrl Pts',(1.4638243133254,1.,-1.27433119897877));
#37266=CARTESIAN_POINT('Ctrl Pts',(1.45843906294725,1.,-1.27156805265312));
#37267=CARTESIAN_POINT('Ctrl Pts',(1.45301422764205,1.,-1.26867786804854));
#37268=CARTESIAN_POINT('Ctrl Pts',(1.44761985001544,1.,-1.26570925118767));
#37269=CARTESIAN_POINT('Ctrl Pts',(1.44236470511145,1.,-1.26273903323723));
#37270=CARTESIAN_POINT('Ctrl Pts',(1.43734919180719,1.,-1.25983531011894));
#37271=CARTESIAN_POINT('Ctrl Pts',(1.43262645609679,1.,-1.25702687965744));
#37272=CARTESIAN_POINT('Ctrl Pts',(1.42815938799555,1.,-1.25426945222783));
#37273=CARTESIAN_POINT('Ctrl Pts',(1.42378102115911,1.,-1.25141455570299));
#37274=CARTESIAN_POINT('Ctrl Pts',(1.41923722596421,1.,-1.24824430986911));
#37275=CARTESIAN_POINT('Ctrl Pts',(1.41422913175437,1.,-1.24450600513278));
#37276=CARTESIAN_POINT('Ctrl Pts',(1.40845295531151,1.,-1.23994455029421));
#37277=CARTESIAN_POINT('Ctrl Pts',(1.40164708205345,1.,-1.23434087289768));
#37278=CARTESIAN_POINT('Ctrl Pts',(1.39361389567257,1.,-1.22752961898063));
#37279=CARTESIAN_POINT('Ctrl Pts',(1.38420564525391,1.,-1.21938737278853));
#37280=CARTESIAN_POINT('Ctrl Pts',(1.37331915604962,1.,-1.20982812923113));
#37281=CARTESIAN_POINT('Ctrl Pts',(1.36088705040677,1.,-1.1987959077656));
#37282=CARTESIAN_POINT('Ctrl Pts',(1.34687053998157,1.,-1.18625865664915));
#37283=CARTESIAN_POINT('Ctrl Pts',(1.33437539344842,1.,-1.17501305787994));
#37284=CARTESIAN_POINT('Ctrl Pts',(1.32428080720544,1.,-1.16589330092532));
#37285=CARTESIAN_POINT('Ctrl Pts',(1.3172297721596,1.,-1.15950888730433));
#37286=CARTESIAN_POINT('Ctrl Pts',(1.31362392696032,1.,-1.15624053661742));
#37287=CARTESIAN_POINT('',(1.73811241238545,0.,-1.34869019493419));
#37288=CARTESIAN_POINT('Origin',(1.81978687191668,0.,-1.23627494547115));
#37289=CARTESIAN_POINT('',(1.81978687191668,1.,-1.23627494547115));
#37290=CARTESIAN_POINT('',(1.73811241238545,1.,-1.34869019493419));
#37291=CARTESIAN_POINT('',(1.81978687191668,0.,-1.23627494547115));
#37292=CARTESIAN_POINT('Ctrl Pts',(1.5055822144029,-1.,-0.892032620296855));
#37293=CARTESIAN_POINT('Ctrl Pts',(1.5055822144029,1.,-0.892032620296855));
#37294=CARTESIAN_POINT('Ctrl Pts',(1.50980486807181,-1.,-0.894452006967538));
#37295=CARTESIAN_POINT('Ctrl Pts',(1.50980486807181,1.,-0.894452006967538));
#37296=CARTESIAN_POINT('Ctrl Pts',(1.51805569591479,-1.,-0.89918504749193));
#37297=CARTESIAN_POINT('Ctrl Pts',(1.51805569591479,1.,-0.89918504749193));
#37298=CARTESIAN_POINT('Ctrl Pts',(1.52984849890434,-1.,-0.905967409640499));
#37299=CARTESIAN_POINT('Ctrl Pts',(1.52984849890434,1.,-0.905967409640499));
#37300=CARTESIAN_POINT('Ctrl Pts',(1.54440491152807,-1.,-0.91437591904658));
#37301=CARTESIAN_POINT('Ctrl Pts',(1.54440491152807,1.,-0.91437591904658));
#37302=CARTESIAN_POINT('Ctrl Pts',(1.56065988582509,-1.,-0.923832188966322));
#37303=CARTESIAN_POINT('Ctrl Pts',(1.56065988582509,1.,-0.923832188966322));
#37304=CARTESIAN_POINT('Ctrl Pts',(1.57499388385561,-1.,-0.932246680128849));
#37305=CARTESIAN_POINT('Ctrl Pts',(1.57499388385561,1.,-0.932246680128849));
#37306=CARTESIAN_POINT('Ctrl Pts',(1.58744937489796,-1.,-0.939646377909319));
#37307=CARTESIAN_POINT('Ctrl Pts',(1.58744937489796,1.,-0.939646377909319));
#37308=CARTESIAN_POINT('Ctrl Pts',(1.59810042045408,-1.,-0.946078063325796));
#37309=CARTESIAN_POINT('Ctrl Pts',(1.59810042045408,1.,-0.946078063325796));
#37310=CARTESIAN_POINT('Ctrl Pts',(1.60706069897794,-1.,-0.951613284361248));
#37311=CARTESIAN_POINT('Ctrl Pts',(1.60706069897794,1.,-0.951613284361248));
#37312=CARTESIAN_POINT('Ctrl Pts',(1.61449324337233,-1.,-0.956354422921573));
#37313=CARTESIAN_POINT('Ctrl Pts',(1.61449324337233,1.,-0.956354422921573));
#37314=CARTESIAN_POINT('Ctrl Pts',(1.62061638139929,-1.,-0.960438326099958));
#37315=CARTESIAN_POINT('Ctrl Pts',(1.62061638139929,1.,-0.960438326099958));
#37316=CARTESIAN_POINT('Ctrl Pts',(1.6257193066974,-1.,-0.964046107037821));
#37317=CARTESIAN_POINT('Ctrl Pts',(1.6257193066974,1.,-0.964046107037821));
#37318=CARTESIAN_POINT('Ctrl Pts',(1.63013849959083,-1.,-0.967387853228041));
#37319=CARTESIAN_POINT('Ctrl Pts',(1.63013849959083,1.,-0.967387853228041));
#37320=CARTESIAN_POINT('Ctrl Pts',(1.63420665729609,-1.,-0.970669715996356));
#37321=CARTESIAN_POINT('Ctrl Pts',(1.63420665729609,1.,-0.970669715996356));
#37322=CARTESIAN_POINT('Ctrl Pts',(1.63820952658157,-1.,-0.974066058287501));
#37323=CARTESIAN_POINT('Ctrl Pts',(1.63820952658157,1.,-0.974066058287501));
#37324=CARTESIAN_POINT('Ctrl Pts',(1.64233990826831,-1.,-0.977689794120297));
#37325=CARTESIAN_POINT('Ctrl Pts',(1.64233990826831,1.,-0.977689794120297));
#37326=CARTESIAN_POINT('Ctrl Pts',(1.64665139190834,-1.,-0.981562530940574));
#37327=CARTESIAN_POINT('Ctrl Pts',(1.64665139190834,1.,-0.981562530940574));
#37328=CARTESIAN_POINT('Ctrl Pts',(1.6511001661277,-1.,-0.985642622921626));
#37329=CARTESIAN_POINT('Ctrl Pts',(1.6511001661277,1.,-0.985642622921626));
#37330=CARTESIAN_POINT('Ctrl Pts',(1.65559044289746,-1.,-0.98985562785445));
#37331=CARTESIAN_POINT('Ctrl Pts',(1.65559044289746,1.,-0.98985562785445));
#37332=CARTESIAN_POINT('Ctrl Pts',(1.66001553809916,-1.,-0.994121836661116));
#37333=CARTESIAN_POINT('Ctrl Pts',(1.66001553809916,1.,-0.994121836661116));
#37334=CARTESIAN_POINT('Ctrl Pts',(1.66430758030304,-1.,-0.998389654952317));
#37335=CARTESIAN_POINT('Ctrl Pts',(1.66430758030304,1.,-0.998389654952317));
#37336=CARTESIAN_POINT('Ctrl Pts',(1.66846059277231,-1.,-1.00265091003682));
#37337=CARTESIAN_POINT('Ctrl Pts',(1.66846059277231,1.,-1.00265091003682));
#37338=CARTESIAN_POINT('Ctrl Pts',(1.67250335383248,-1.,-1.00692206696387));
#37339=CARTESIAN_POINT('Ctrl Pts',(1.67250335383248,1.,-1.00692206696387));
#37340=CARTESIAN_POINT('Ctrl Pts',(1.67648246776457,-1.,-1.01123236493507));
#37341=CARTESIAN_POINT('Ctrl Pts',(1.67648246776457,1.,-1.01123236493507));
#37342=CARTESIAN_POINT('Ctrl Pts',(1.6804428989482,-1.,-1.01561026162787));
#37343=CARTESIAN_POINT('Ctrl Pts',(1.6804428989482,1.,-1.01561026162787));
#37344=CARTESIAN_POINT('Ctrl Pts',(1.68440578021739,-1.,-1.02006795074222));
#37345=CARTESIAN_POINT('Ctrl Pts',(1.68440578021739,1.,-1.02006795074222));
#37346=CARTESIAN_POINT('Ctrl Pts',(1.68836910178475,-1.,-1.02460180535272));
#37347=CARTESIAN_POINT('Ctrl Pts',(1.68836910178475,1.,-1.02460180535272));
#37348=CARTESIAN_POINT('Ctrl Pts',(1.69231840863471,-1.,-1.02919977579155));
#37349=CARTESIAN_POINT('Ctrl Pts',(1.69231840863471,1.,-1.02919977579155));
#37350=CARTESIAN_POINT('Ctrl Pts',(1.69623414782769,-1.,-1.03384646003587));
#37351=CARTESIAN_POINT('Ctrl Pts',(1.69623414782769,1.,-1.03384646003587));
#37352=CARTESIAN_POINT('Ctrl Pts',(1.70010052930951,-1.,-1.03852922490782));
#37353=CARTESIAN_POINT('Ctrl Pts',(1.70010052930951,1.,-1.03852922490782));
#37354=CARTESIAN_POINT('Ctrl Pts',(1.70391338707969,-1.,-1.04324363334546));
#37355=CARTESIAN_POINT('Ctrl Pts',(1.70391338707969,1.,-1.04324363334546));
#37356=CARTESIAN_POINT('Ctrl Pts',(1.70767646263641,-1.,-1.0479908540499));
#37357=CARTESIAN_POINT('Ctrl Pts',(1.70767646263641,1.,-1.0479908540499));
#37358=CARTESIAN_POINT('Ctrl Pts',(1.71139783543986,-1.,-1.05277517202854));
#37359=CARTESIAN_POINT('Ctrl Pts',(1.71139783543986,1.,-1.05277517202854));
#37360=CARTESIAN_POINT('Ctrl Pts',(1.71508654427022,-1.,-1.05760163192481));
#37361=CARTESIAN_POINT('Ctrl Pts',(1.71508654427022,1.,-1.05760163192481));
#37362=CARTESIAN_POINT('Ctrl Pts',(1.71874858456908,-1.,-1.0624732468065));
#37363=CARTESIAN_POINT('Ctrl Pts',(1.71874858456908,1.,-1.0624732468065));
#37364=CARTESIAN_POINT('Ctrl Pts',(1.72238500928456,-1.,-1.06738966975463));
#37365=CARTESIAN_POINT('Ctrl Pts',(1.72238500928456,1.,-1.06738966975463));
#37366=CARTESIAN_POINT('Ctrl Pts',(1.72599406198489,-1.,-1.07234866990252));
#37367=CARTESIAN_POINT('Ctrl Pts',(1.72599406198489,1.,-1.07234866990252));
#37368=CARTESIAN_POINT('Ctrl Pts',(1.72957248977424,-1.,-1.0773470373727));
#37369=CARTESIAN_POINT('Ctrl Pts',(1.72957248977424,1.,-1.0773470373727));
#37370=CARTESIAN_POINT('Ctrl Pts',(1.73311705663407,-1.,-1.08238162784749));
#37371=CARTESIAN_POINT('Ctrl Pts',(1.73311705663407,1.,-1.08238162784749));
#37372=CARTESIAN_POINT('Ctrl Pts',(1.73662628326093,-1.,-1.08745056285429));
#37373=CARTESIAN_POINT('Ctrl Pts',(1.73662628326093,1.,-1.08745056285429));
#37374=CARTESIAN_POINT('Ctrl Pts',(1.74010053962252,-1.,-1.09255329056496));
#37375=CARTESIAN_POINT('Ctrl Pts',(1.74010053962252,1.,-1.09255329056496));
#37376=CARTESIAN_POINT('Ctrl Pts',(1.74354119236212,-1.,-1.09768999241229));
#37377=CARTESIAN_POINT('Ctrl Pts',(1.74354119236212,1.,-1.09768999241229));
#37378=CARTESIAN_POINT('Ctrl Pts',(1.74695004214924,-1.,-1.10286118991144));
#37379=CARTESIAN_POINT('Ctrl Pts',(1.74695004214924,1.,-1.10286118991144));
#37380=CARTESIAN_POINT('Ctrl Pts',(1.75032866075914,-1.,-1.10806728183003));
#37381=CARTESIAN_POINT('Ctrl Pts',(1.75032866075914,1.,-1.10806728183003));
#37382=CARTESIAN_POINT('Ctrl Pts',(1.75367772094617,-1.,-1.11330807582542));
#37383=CARTESIAN_POINT('Ctrl Pts',(1.75367772094617,1.,-1.11330807582542));
#37384=CARTESIAN_POINT('Ctrl Pts',(1.75699720772089,-1.,-1.11858293216752));
#37385=CARTESIAN_POINT('Ctrl Pts',(1.75699720772089,1.,-1.11858293216752));
#37386=CARTESIAN_POINT('Ctrl Pts',(1.76028671825084,-1.,-1.12389096855078));
#37387=CARTESIAN_POINT('Ctrl Pts',(1.76028671825084,1.,-1.12389096855078));
#37388=CARTESIAN_POINT('Ctrl Pts',(1.76354571966171,-1.,-1.12923123555076));
#37389=CARTESIAN_POINT('Ctrl Pts',(1.76354571966171,1.,-1.12923123555076));
#37390=CARTESIAN_POINT('Ctrl Pts',(1.76677384551883,-1.,-1.13460291804635));
#37391=CARTESIAN_POINT('Ctrl Pts',(1.76677384551883,1.,-1.13460291804635));
#37392=CARTESIAN_POINT('Ctrl Pts',(1.76997111386806,-1.,-1.14000548337));
#37393=CARTESIAN_POINT('Ctrl Pts',(1.76997111386806,1.,-1.14000548337));
#37394=CARTESIAN_POINT('Ctrl Pts',(1.77313777896234,-1.,-1.14543858226948));
#37395=CARTESIAN_POINT('Ctrl Pts',(1.77313777896234,1.,-1.14543858226948));
#37396=CARTESIAN_POINT('Ctrl Pts',(1.77627422557034,-1.,-1.15090197841531));
#37397=CARTESIAN_POINT('Ctrl Pts',(1.77627422557034,1.,-1.15090197841531));
#37398=CARTESIAN_POINT('Ctrl Pts',(1.77938085564261,-1.,-1.15639547194689));
#37399=CARTESIAN_POINT('Ctrl Pts',(1.77938085564261,1.,-1.15639547194689));
#37400=CARTESIAN_POINT('Ctrl Pts',(1.78245795880949,-1.,-1.16191881298458));
#37401=CARTESIAN_POINT('Ctrl Pts',(1.78245795880949,1.,-1.16191881298458));
#37402=CARTESIAN_POINT('Ctrl Pts',(1.78550566040349,-1.,-1.16747166312239));
#37403=CARTESIAN_POINT('Ctrl Pts',(1.78550566040349,1.,-1.16747166312239));
#37404=CARTESIAN_POINT('Ctrl Pts',(1.78852398877523,-1.,-1.17305363177265));
#37405=CARTESIAN_POINT('Ctrl Pts',(1.78852398877523,1.,-1.17305363177265));
#37406=CARTESIAN_POINT('Ctrl Pts',(1.79151291552646,-1.,-1.17866429440781));
#37407=CARTESIAN_POINT('Ctrl Pts',(1.79151291552646,1.,-1.17866429440781));
#37408=CARTESIAN_POINT('Ctrl Pts',(1.79447240321572,-1.,-1.18430321697471));
#37409=CARTESIAN_POINT('Ctrl Pts',(1.79447240321572,1.,-1.18430321697471));
#37410=CARTESIAN_POINT('Ctrl Pts',(1.79740245923649,-1.,-1.1899699793456));
#37411=CARTESIAN_POINT('Ctrl Pts',(1.79740245923649,1.,-1.1899699793456));
#37412=CARTESIAN_POINT('Ctrl Pts',(1.80030314370121,-1.,-1.19566418930405));
#37413=CARTESIAN_POINT('Ctrl Pts',(1.80030314370121,1.,-1.19566418930405));
#37414=CARTESIAN_POINT('Ctrl Pts',(1.8031745483882,-1.,-1.2013854893912));
#37415=CARTESIAN_POINT('Ctrl Pts',(1.8031745483882,1.,-1.2013854893912));
#37416=CARTESIAN_POINT('Ctrl Pts',(1.80601678480772,-1.,-1.20713356605519));
#37417=CARTESIAN_POINT('Ctrl Pts',(1.80601678480772,1.,-1.20713356605519));
#37418=CARTESIAN_POINT('Ctrl Pts',(1.80882996916931,-1.,-1.2129081570818));
#37419=CARTESIAN_POINT('Ctrl Pts',(1.80882996916931,1.,-1.2129081570818));
#37420=CARTESIAN_POINT('Ctrl Pts',(1.81161420806172,-1.,-1.2187090610323));
#37421=CARTESIAN_POINT('Ctrl Pts',(1.81161420806172,1.,-1.2187090610323));
#37422=CARTESIAN_POINT('Ctrl Pts',(1.81436959209778,-1.,-1.22453613304507));
#37423=CARTESIAN_POINT('Ctrl Pts',(1.81436959209778,1.,-1.22453613304507));
#37424=CARTESIAN_POINT('Ctrl Pts',(1.81655087183054,-1.,-1.22921864890975));
#37425=CARTESIAN_POINT('Ctrl Pts',(1.81655087183054,1.,-1.22921864890975));
#37426=CARTESIAN_POINT('Ctrl Pts',(1.81817389920914,-1.,-1.23274224526804));
#37427=CARTESIAN_POINT('Ctrl Pts',(1.81817389920914,1.,-1.23274224526804));
#37428=CARTESIAN_POINT('Ctrl Pts',(1.81925017193531,-1.,-1.23509651170384));
#37429=CARTESIAN_POINT('Ctrl Pts',(1.81925017193531,1.,-1.23509651170384));
#37430=CARTESIAN_POINT('Ctrl Pts',(1.81978687191668,-1.,-1.23627494547115));
#37431=CARTESIAN_POINT('Ctrl Pts',(1.81978687191668,1.,-1.23627494547115));
#37432=CARTESIAN_POINT('',(1.5055822144029,1.,-0.892032620296855));
#37433=CARTESIAN_POINT('Ctrl Pts',(1.5055822144029,1.,-0.892032620296855));
#37434=CARTESIAN_POINT('Ctrl Pts',(1.50980486807181,1.,-0.894452006967538));
#37435=CARTESIAN_POINT('Ctrl Pts',(1.51805569591479,1.,-0.89918504749193));
#37436=CARTESIAN_POINT('Ctrl Pts',(1.52984849890434,1.,-0.905967409640499));
#37437=CARTESIAN_POINT('Ctrl Pts',(1.54440491152807,1.,-0.91437591904658));
#37438=CARTESIAN_POINT('Ctrl Pts',(1.56065988582509,1.,-0.923832188966322));
#37439=CARTESIAN_POINT('Ctrl Pts',(1.57499388385561,1.,-0.932246680128849));
#37440=CARTESIAN_POINT('Ctrl Pts',(1.58744937489796,1.,-0.939646377909319));
#37441=CARTESIAN_POINT('Ctrl Pts',(1.59810042045408,1.,-0.946078063325796));
#37442=CARTESIAN_POINT('Ctrl Pts',(1.60706069897794,1.,-0.951613284361248));
#37443=CARTESIAN_POINT('Ctrl Pts',(1.61449324337233,1.,-0.956354422921573));
#37444=CARTESIAN_POINT('Ctrl Pts',(1.62061638139929,1.,-0.960438326099958));
#37445=CARTESIAN_POINT('Ctrl Pts',(1.6257193066974,1.,-0.964046107037821));
#37446=CARTESIAN_POINT('Ctrl Pts',(1.63013849959083,1.,-0.967387853228041));
#37447=CARTESIAN_POINT('Ctrl Pts',(1.63420665729609,1.,-0.970669715996356));
#37448=CARTESIAN_POINT('Ctrl Pts',(1.63820952658157,1.,-0.974066058287501));
#37449=CARTESIAN_POINT('Ctrl Pts',(1.64233990826831,1.,-0.977689794120297));
#37450=CARTESIAN_POINT('Ctrl Pts',(1.64665139190834,1.,-0.981562530940574));
#37451=CARTESIAN_POINT('Ctrl Pts',(1.6511001661277,1.,-0.985642622921626));
#37452=CARTESIAN_POINT('Ctrl Pts',(1.65559044289746,1.,-0.98985562785445));
#37453=CARTESIAN_POINT('Ctrl Pts',(1.66001553809916,1.,-0.994121836661116));
#37454=CARTESIAN_POINT('Ctrl Pts',(1.66430758030304,1.,-0.998389654952317));
#37455=CARTESIAN_POINT('Ctrl Pts',(1.66846059277231,1.,-1.00265091003682));
#37456=CARTESIAN_POINT('Ctrl Pts',(1.67250335383248,1.,-1.00692206696387));
#37457=CARTESIAN_POINT('Ctrl Pts',(1.67648246776457,1.,-1.01123236493507));
#37458=CARTESIAN_POINT('Ctrl Pts',(1.6804428989482,1.,-1.01561026162787));
#37459=CARTESIAN_POINT('Ctrl Pts',(1.68440578021739,1.,-1.02006795074222));
#37460=CARTESIAN_POINT('Ctrl Pts',(1.68836910178475,1.,-1.02460180535272));
#37461=CARTESIAN_POINT('Ctrl Pts',(1.69231840863471,1.,-1.02919977579155));
#37462=CARTESIAN_POINT('Ctrl Pts',(1.69623414782769,1.,-1.03384646003587));
#37463=CARTESIAN_POINT('Ctrl Pts',(1.70010052930951,1.,-1.03852922490782));
#37464=CARTESIAN_POINT('Ctrl Pts',(1.70391338707969,1.,-1.04324363334546));
#37465=CARTESIAN_POINT('Ctrl Pts',(1.70767646263641,1.,-1.0479908540499));
#37466=CARTESIAN_POINT('Ctrl Pts',(1.71139783543986,1.,-1.05277517202854));
#37467=CARTESIAN_POINT('Ctrl Pts',(1.71508654427022,1.,-1.05760163192481));
#37468=CARTESIAN_POINT('Ctrl Pts',(1.71874858456908,1.,-1.0624732468065));
#37469=CARTESIAN_POINT('Ctrl Pts',(1.72238500928456,1.,-1.06738966975463));
#37470=CARTESIAN_POINT('Ctrl Pts',(1.72599406198489,1.,-1.07234866990252));
#37471=CARTESIAN_POINT('Ctrl Pts',(1.72957248977424,1.,-1.0773470373727));
#37472=CARTESIAN_POINT('Ctrl Pts',(1.73311705663407,1.,-1.08238162784749));
#37473=CARTESIAN_POINT('Ctrl Pts',(1.73662628326093,1.,-1.08745056285429));
#37474=CARTESIAN_POINT('Ctrl Pts',(1.74010053962252,1.,-1.09255329056496));
#37475=CARTESIAN_POINT('Ctrl Pts',(1.74354119236212,1.,-1.09768999241229));
#37476=CARTESIAN_POINT('Ctrl Pts',(1.74695004214924,1.,-1.10286118991144));
#37477=CARTESIAN_POINT('Ctrl Pts',(1.75032866075914,1.,-1.10806728183003));
#37478=CARTESIAN_POINT('Ctrl Pts',(1.75367772094617,1.,-1.11330807582542));
#37479=CARTESIAN_POINT('Ctrl Pts',(1.75699720772089,1.,-1.11858293216752));
#37480=CARTESIAN_POINT('Ctrl Pts',(1.76028671825084,1.,-1.12389096855078));
#37481=CARTESIAN_POINT('Ctrl Pts',(1.76354571966171,1.,-1.12923123555076));
#37482=CARTESIAN_POINT('Ctrl Pts',(1.76677384551883,1.,-1.13460291804635));
#37483=CARTESIAN_POINT('Ctrl Pts',(1.76997111386806,1.,-1.14000548337));
#37484=CARTESIAN_POINT('Ctrl Pts',(1.77313777896234,1.,-1.14543858226948));
#37485=CARTESIAN_POINT('Ctrl Pts',(1.77627422557034,1.,-1.15090197841531));
#37486=CARTESIAN_POINT('Ctrl Pts',(1.77938085564261,1.,-1.15639547194689));
#37487=CARTESIAN_POINT('Ctrl Pts',(1.78245795880949,1.,-1.16191881298458));
#37488=CARTESIAN_POINT('Ctrl Pts',(1.78550566040349,1.,-1.16747166312239));
#37489=CARTESIAN_POINT('Ctrl Pts',(1.78852398877523,1.,-1.17305363177265));
#37490=CARTESIAN_POINT('Ctrl Pts',(1.79151291552646,1.,-1.17866429440781));
#37491=CARTESIAN_POINT('Ctrl Pts',(1.79447240321572,1.,-1.18430321697471));
#37492=CARTESIAN_POINT('Ctrl Pts',(1.79740245923649,1.,-1.1899699793456));
#37493=CARTESIAN_POINT('Ctrl Pts',(1.80030314370121,1.,-1.19566418930405));
#37494=CARTESIAN_POINT('Ctrl Pts',(1.8031745483882,1.,-1.2013854893912));
#37495=CARTESIAN_POINT('Ctrl Pts',(1.80601678480772,1.,-1.20713356605519));
#37496=CARTESIAN_POINT('Ctrl Pts',(1.80882996916931,1.,-1.2129081570818));
#37497=CARTESIAN_POINT('Ctrl Pts',(1.81161420806172,1.,-1.2187090610323));
#37498=CARTESIAN_POINT('Ctrl Pts',(1.81436959209778,1.,-1.22453613304507));
#37499=CARTESIAN_POINT('Ctrl Pts',(1.81655087183054,1.,-1.22921864890975));
#37500=CARTESIAN_POINT('Ctrl Pts',(1.81817389920914,1.,-1.23274224526804));
#37501=CARTESIAN_POINT('Ctrl Pts',(1.81925017193531,1.,-1.23509651170384));
#37502=CARTESIAN_POINT('Ctrl Pts',(1.81978687191668,1.,-1.23627494547115));
#37503=CARTESIAN_POINT('',(1.5055822144029,0.,-0.892032620296855));
#37504=CARTESIAN_POINT('Origin',(0.,0.,0.));
#37505=CARTESIAN_POINT('',(1.60662857109684,1.,-0.693717979106306));
#37506=CARTESIAN_POINT('Origin',(0.,1.,0.));
#37507=CARTESIAN_POINT('',(1.60662857109684,0.,-0.693717979106308));
#37508=CARTESIAN_POINT('Ctrl Pts',(2.0698113262342,-1.,-0.745574324794401));
#37509=CARTESIAN_POINT('Ctrl Pts',(2.0698113262342,1.,-0.745574324794401));
#37510=CARTESIAN_POINT('Ctrl Pts',(2.06854248895728,-1.,-0.745832791378367));
#37511=CARTESIAN_POINT('Ctrl Pts',(2.06854248895728,1.,-0.745832791378367));
#37512=CARTESIAN_POINT('Ctrl Pts',(2.06600523016815,-1.,-0.746345871544201));
#37513=CARTESIAN_POINT('Ctrl Pts',(2.06600523016815,1.,-0.746345871544201));
#37514=CARTESIAN_POINT('Ctrl Pts',(2.06220058927826,-1.,-0.74710393278792));
#37515=CARTESIAN_POINT('Ctrl Pts',(2.06220058927826,1.,-0.74710393278792));
#37516=CARTESIAN_POINT('Ctrl Pts',(2.05713023031006,-1.,-0.748091554183803));
#37517=CARTESIAN_POINT('Ctrl Pts',(2.05713023031006,1.,-0.748091554183803));
#37518=CARTESIAN_POINT('Ctrl Pts',(2.05079645592154,-1.,-0.749287468665046));
#37519=CARTESIAN_POINT('Ctrl Pts',(2.05079645592154,1.,-0.749287468665046));
#37520=CARTESIAN_POINT('Ctrl Pts',(2.04446689147979,-1.,-0.750444657875576));
#37521=CARTESIAN_POINT('Ctrl Pts',(2.04446689147979,1.,-0.750444657875576));
#37522=CARTESIAN_POINT('Ctrl Pts',(2.03814160092099,-1.,-0.751562963361115));
#37523=CARTESIAN_POINT('Ctrl Pts',(2.03814160092099,1.,-0.751562963361115));
#37524=CARTESIAN_POINT('Ctrl Pts',(2.03182068456221,-1.,-0.752642180487211));
#37525=CARTESIAN_POINT('Ctrl Pts',(2.03182068456221,1.,-0.752642180487211));
#37526=CARTESIAN_POINT('Ctrl Pts',(2.02550428623313,-1.,-0.753682061112768));
#37527=CARTESIAN_POINT('Ctrl Pts',(2.02550428623313,1.,-0.753682061112768));
#37528=CARTESIAN_POINT('Ctrl Pts',(2.01919259405809,-1.,-0.754682330722816));
#37529=CARTESIAN_POINT('Ctrl Pts',(2.01919259405809,1.,-0.754682330722816));
#37530=CARTESIAN_POINT('Ctrl Pts',(2.01288584328084,-1.,-0.755642704957865));
#37531=CARTESIAN_POINT('Ctrl Pts',(2.01288584328084,1.,-0.755642704957865));
#37532=CARTESIAN_POINT('Ctrl Pts',(2.0065843158773,-1.,-0.756562904646671));
#37533=CARTESIAN_POINT('Ctrl Pts',(2.0065843158773,1.,-0.756562904646671));
#37534=CARTESIAN_POINT('Ctrl Pts',(2.00028834739178,-1.,-0.757442676862724));
#37535=CARTESIAN_POINT('Ctrl Pts',(2.00028834739178,1.,-0.757442676862724));
#37536=CARTESIAN_POINT('Ctrl Pts',(1.99399831098817,-1.,-0.758281796766761));
#37537=CARTESIAN_POINT('Ctrl Pts',(1.99399831098817,1.,-0.758281796766761));
#37538=CARTESIAN_POINT('Ctrl Pts',(1.98771456680874,-1.,-0.759080037802488));
#37539=CARTESIAN_POINT('Ctrl Pts',(1.98771456680874,1.,-0.759080037802488));
#37540=CARTESIAN_POINT('Ctrl Pts',(1.98143741418172,-1.,-0.75983714745219));
#37541=CARTESIAN_POINT('Ctrl Pts',(1.98143741418172,1.,-0.75983714745219));
#37542=CARTESIAN_POINT('Ctrl Pts',(1.97516705321494,-1.,-0.760552825409757));
#37543=CARTESIAN_POINT('Ctrl Pts',(1.97516705321494,1.,-0.760552825409757));
#37544=CARTESIAN_POINT('Ctrl Pts',(1.96890351582499,-1.,-0.761226690483821));
#37545=CARTESIAN_POINT('Ctrl Pts',(1.96890351582499,1.,-0.761226690483821));
#37546=CARTESIAN_POINT('Ctrl Pts',(1.96264672744186,-1.,-0.761858300014424));
#37547=CARTESIAN_POINT('Ctrl Pts',(1.96264672744186,1.,-0.761858300014424));
#37548=CARTESIAN_POINT('Ctrl Pts',(1.95639665309869,-1.,-0.762447203806179));
#37549=CARTESIAN_POINT('Ctrl Pts',(1.95639665309869,1.,-0.762447203806179));
#37550=CARTESIAN_POINT('Ctrl Pts',(1.95015342590024,-1.,-0.762992990878769));
#37551=CARTESIAN_POINT('Ctrl Pts',(1.95015342590024,1.,-0.762992990878769));
#37552=CARTESIAN_POINT('Ctrl Pts',(1.9439174661764,-1.,-0.763495333538629));
#37553=CARTESIAN_POINT('Ctrl Pts',(1.9439174661764,1.,-0.763495333538629));
#37554=CARTESIAN_POINT('Ctrl Pts',(1.93768964875886,-1.,-0.763954049121459));
#37555=CARTESIAN_POINT('Ctrl Pts',(1.93768964875886,1.,-0.763954049121459));
#37556=CARTESIAN_POINT('Ctrl Pts',(1.93147105496382,-1.,-0.764369010673941));
#37557=CARTESIAN_POINT('Ctrl Pts',(1.93147105496382,1.,-0.764369010673941));
#37558=CARTESIAN_POINT('Ctrl Pts',(1.92526263537048,-1.,-0.764740025488212));
#37559=CARTESIAN_POINT('Ctrl Pts',(1.92526263537048,1.,-0.764740025488212));
#37560=CARTESIAN_POINT('Ctrl Pts',(1.91906491634196,-1.,-0.765066729667089));
#37561=CARTESIAN_POINT('Ctrl Pts',(1.91906491634196,1.,-0.765066729667089));
#37562=CARTESIAN_POINT('Ctrl Pts',(1.91287765805169,-1.,-0.765348465884722));
#37563=CARTESIAN_POINT('Ctrl Pts',(1.91287765805169,1.,-0.765348465884722));
#37564=CARTESIAN_POINT('Ctrl Pts',(1.90669961402356,-1.,-0.765584196937919));
#37565=CARTESIAN_POINT('Ctrl Pts',(1.90669961402356,1.,-0.765584196937919));
#37566=CARTESIAN_POINT('Ctrl Pts',(1.90052930393596,-1.,-0.765772772593386));
#37567=CARTESIAN_POINT('Ctrl Pts',(1.90052930393596,1.,-0.765772772593386));
#37568=CARTESIAN_POINT('Ctrl Pts',(1.89436577771388,-1.,-0.765913193856978));
#37569=CARTESIAN_POINT('Ctrl Pts',(1.89436577771388,1.,-0.765913193856978));
#37570=CARTESIAN_POINT('Ctrl Pts',(1.88820926433409,-1.,-0.766004837062091));
#37571=CARTESIAN_POINT('Ctrl Pts',(1.88820926433409,1.,-0.766004837062091));
#37572=CARTESIAN_POINT('Ctrl Pts',(1.88206215302561,-1.,-0.766047794851865));
#37573=CARTESIAN_POINT('Ctrl Pts',(1.88206215302561,1.,-0.766047794851865));
#37574=CARTESIAN_POINT('Ctrl Pts',(1.87592888967883,-1.,-0.766042837036744));
#37575=CARTESIAN_POINT('Ctrl Pts',(1.87592888967883,1.,-0.766042837036744));
#37576=CARTESIAN_POINT('Ctrl Pts',(1.86981398314341,-1.,-0.765990708546091));
#37577=CARTESIAN_POINT('Ctrl Pts',(1.86981398314341,1.,-0.765990708546091));
#37578=CARTESIAN_POINT('Ctrl Pts',(1.86372027063312,-1.,-0.765891519092547));
#37579=CARTESIAN_POINT('Ctrl Pts',(1.86372027063312,1.,-0.765891519092547));
#37580=CARTESIAN_POINT('Ctrl Pts',(1.85764741390394,-1.,-0.765744212909319));
#37581=CARTESIAN_POINT('Ctrl Pts',(1.85764741390394,1.,-0.765744212909319));
#37582=CARTESIAN_POINT('Ctrl Pts',(1.85158945130063,-1.,-0.765545710619063));
#37583=CARTESIAN_POINT('Ctrl Pts',(1.85158945130063,1.,-0.765545710619063));
#37584=CARTESIAN_POINT('Ctrl Pts',(1.84553698875924,-1.,-0.765291664862029));
#37585=CARTESIAN_POINT('Ctrl Pts',(1.84553698875924,1.,-0.765291664862029));
#37586=CARTESIAN_POINT('Ctrl Pts',(1.83948181064835,-1.,-0.764978057881738));
#37587=CARTESIAN_POINT('Ctrl Pts',(1.83948181064835,1.,-0.764978057881738));
#37588=CARTESIAN_POINT('Ctrl Pts',(1.83342077227142,-1.,-0.764602549687853));
#37589=CARTESIAN_POINT('Ctrl Pts',(1.83342077227142,1.,-0.764602549687853));
#37590=CARTESIAN_POINT('Ctrl Pts',(1.82735991200065,-1.,-0.764165902605995));
#37591=CARTESIAN_POINT('Ctrl Pts',(1.82735991200065,1.,-0.764165902605995));
#37592=CARTESIAN_POINT('Ctrl Pts',(1.82131873145266,-1.,-0.763673465462727));
#37593=CARTESIAN_POINT('Ctrl Pts',(1.82131873145266,1.,-0.763673465462727));
#37594=CARTESIAN_POINT('Ctrl Pts',(1.8153211840553,-1.,-0.763132003836634));
#37595=CARTESIAN_POINT('Ctrl Pts',(1.8153211840553,1.,-0.763132003836634));
#37596=CARTESIAN_POINT('Ctrl Pts',(1.80938551463965,-1.,-0.762546129463938));
#37597=CARTESIAN_POINT('Ctrl Pts',(1.80938551463965,1.,-0.762546129463938));
#37598=CARTESIAN_POINT('Ctrl Pts',(1.80351583877342,-1.,-0.761915336443547));
#37599=CARTESIAN_POINT('Ctrl Pts',(1.80351583877342,1.,-0.761915336443547));
#37600=CARTESIAN_POINT('Ctrl Pts',(1.79768986997783,-1.,-0.761229695230558));
#37601=CARTESIAN_POINT('Ctrl Pts',(1.79768986997783,1.,-0.761229695230558));
#37602=CARTESIAN_POINT('Ctrl Pts',(1.7918581561088,-1.,-0.760469555880749));
#37603=CARTESIAN_POINT('Ctrl Pts',(1.7918581561088,1.,-0.760469555880749));
#37604=CARTESIAN_POINT('Ctrl Pts',(1.78596964884604,-1.,-0.75961440111019));
#37605=CARTESIAN_POINT('Ctrl Pts',(1.78596964884604,1.,-0.75961440111019));
#37606=CARTESIAN_POINT('Ctrl Pts',(1.77999411220945,-1.,-0.758650626677519));
#37607=CARTESIAN_POINT('Ctrl Pts',(1.77999411220945,1.,-0.758650626677519));
#37608=CARTESIAN_POINT('Ctrl Pts',(1.77394167108292,-1.,-0.757578264077029));
#37609=CARTESIAN_POINT('Ctrl Pts',(1.77394167108292,1.,-0.757578264077029));
#37610=CARTESIAN_POINT('Ctrl Pts',(1.76789396002998,-1.,-0.75642189602781));
#37611=CARTESIAN_POINT('Ctrl Pts',(1.76789396002998,1.,-0.75642189602781));
#37612=CARTESIAN_POINT('Ctrl Pts',(1.76197817240128,-1.,-0.755220979974462));
#37613=CARTESIAN_POINT('Ctrl Pts',(1.76197817240128,1.,-0.755220979974462));
#37614=CARTESIAN_POINT('Ctrl Pts',(1.75631083600019,-1.,-0.754009254027829));
#37615=CARTESIAN_POINT('Ctrl Pts',(1.75631083600019,1.,-0.754009254027829));
#37616=CARTESIAN_POINT('Ctrl Pts',(1.75095139468794,-1.,-0.752797683531314));
#37617=CARTESIAN_POINT('Ctrl Pts',(1.75095139468794,1.,-0.752797683531314));
#37618=CARTESIAN_POINT('Ctrl Pts',(1.74585086852502,-1.,-0.751555614164483));
#37619=CARTESIAN_POINT('Ctrl Pts',(1.74585086852502,1.,-0.751555614164483));
#37620=CARTESIAN_POINT('Ctrl Pts',(1.74080458267114,-1.,-0.75019343598125));
#37621=CARTESIAN_POINT('Ctrl Pts',(1.74080458267114,1.,-0.75019343598125));
#37622=CARTESIAN_POINT('Ctrl Pts',(1.7355035168033,-1.,-0.74858246295687));
#37623=CARTESIAN_POINT('Ctrl Pts',(1.7355035168033,1.,-0.74858246295687));
#37624=CARTESIAN_POINT('Ctrl Pts',(1.72958533647714,-1.,-0.746574710097752));
#37625=CARTESIAN_POINT('Ctrl Pts',(1.72958533647714,1.,-0.746574710097752));
#37626=CARTESIAN_POINT('Ctrl Pts',(1.72268229916769,-1.,-0.744021445433094));
#37627=CARTESIAN_POINT('Ctrl Pts',(1.72268229916769,1.,-0.744021445433094));
#37628=CARTESIAN_POINT('Ctrl Pts',(1.71447789751001,-1.,-0.74079516202821));
#37629=CARTESIAN_POINT('Ctrl Pts',(1.71447789751001,1.,-0.74079516202821));
#37630=CARTESIAN_POINT('Ctrl Pts',(1.70473309004249,-1.,-0.736799665716932));
#37631=CARTESIAN_POINT('Ctrl Pts',(1.70473309004249,1.,-0.736799665716932));
#37632=CARTESIAN_POINT('Ctrl Pts',(1.69326921972915,-1.,-0.731963238685357));
#37633=CARTESIAN_POINT('Ctrl Pts',(1.69326921972915,1.,-0.731963238685357));
#37634=CARTESIAN_POINT('Ctrl Pts',(1.67996158451922,-1.,-0.726235967982445));
#37635=CARTESIAN_POINT('Ctrl Pts',(1.67996158451922,1.,-0.726235967982445));
#37636=CARTESIAN_POINT('Ctrl Pts',(1.66472880551777,-1.,-0.71958543378795));
#37637=CARTESIAN_POINT('Ctrl Pts',(1.66472880551777,1.,-0.71958543378795));
#37638=CARTESIAN_POINT('Ctrl Pts',(1.64752408828442,-1.,-0.711993139340448));
#37639=CARTESIAN_POINT('Ctrl Pts',(1.64752408828442,1.,-0.711993139340448));
#37640=CARTESIAN_POINT('Ctrl Pts',(1.6321654166204,-1.,-0.705159151977294));
#37641=CARTESIAN_POINT('Ctrl Pts',(1.6321654166204,1.,-0.705159151977294));
#37642=CARTESIAN_POINT('Ctrl Pts',(1.61974673471117,-1.,-0.699605146398837));
#37643=CARTESIAN_POINT('Ctrl Pts',(1.61974673471117,1.,-0.699605146398837));
#37644=CARTESIAN_POINT('Ctrl Pts',(1.61106790957619,-1.,-0.69571209787897));
#37645=CARTESIAN_POINT('Ctrl Pts',(1.61106790957619,1.,-0.69571209787897));
#37646=CARTESIAN_POINT('Ctrl Pts',(1.60662857109684,-1.,-0.693717979106306));
#37647=CARTESIAN_POINT('Ctrl Pts',(1.60662857109684,1.,-0.693717979106306));
#37648=CARTESIAN_POINT('',(2.0698113262342,1.,-0.745574324794401));
#37649=CARTESIAN_POINT('Ctrl Pts',(2.0698113262342,1.,-0.745574324794401));
#37650=CARTESIAN_POINT('Ctrl Pts',(2.06854248895728,1.,-0.745832791378367));
#37651=CARTESIAN_POINT('Ctrl Pts',(2.06600523016815,1.,-0.746345871544201));
#37652=CARTESIAN_POINT('Ctrl Pts',(2.06220058927826,1.,-0.74710393278792));
#37653=CARTESIAN_POINT('Ctrl Pts',(2.05713023031006,1.,-0.748091554183803));
#37654=CARTESIAN_POINT('Ctrl Pts',(2.05079645592154,1.,-0.749287468665046));
#37655=CARTESIAN_POINT('Ctrl Pts',(2.04446689147979,1.,-0.750444657875576));
#37656=CARTESIAN_POINT('Ctrl Pts',(2.03814160092099,1.,-0.751562963361115));
#37657=CARTESIAN_POINT('Ctrl Pts',(2.03182068456221,1.,-0.752642180487211));
#37658=CARTESIAN_POINT('Ctrl Pts',(2.02550428623313,1.,-0.753682061112768));
#37659=CARTESIAN_POINT('Ctrl Pts',(2.01919259405809,1.,-0.754682330722816));
#37660=CARTESIAN_POINT('Ctrl Pts',(2.01288584328084,1.,-0.755642704957865));
#37661=CARTESIAN_POINT('Ctrl Pts',(2.0065843158773,1.,-0.756562904646671));
#37662=CARTESIAN_POINT('Ctrl Pts',(2.00028834739178,1.,-0.757442676862724));
#37663=CARTESIAN_POINT('Ctrl Pts',(1.99399831098817,1.,-0.758281796766761));
#37664=CARTESIAN_POINT('Ctrl Pts',(1.98771456680874,1.,-0.759080037802488));
#37665=CARTESIAN_POINT('Ctrl Pts',(1.98143741418172,1.,-0.75983714745219));
#37666=CARTESIAN_POINT('Ctrl Pts',(1.97516705321494,1.,-0.760552825409757));
#37667=CARTESIAN_POINT('Ctrl Pts',(1.96890351582499,1.,-0.761226690483821));
#37668=CARTESIAN_POINT('Ctrl Pts',(1.96264672744186,1.,-0.761858300014424));
#37669=CARTESIAN_POINT('Ctrl Pts',(1.95639665309869,1.,-0.762447203806179));
#37670=CARTESIAN_POINT('Ctrl Pts',(1.95015342590024,1.,-0.762992990878769));
#37671=CARTESIAN_POINT('Ctrl Pts',(1.9439174661764,1.,-0.763495333538629));
#37672=CARTESIAN_POINT('Ctrl Pts',(1.93768964875886,1.,-0.763954049121459));
#37673=CARTESIAN_POINT('Ctrl Pts',(1.93147105496382,1.,-0.764369010673941));
#37674=CARTESIAN_POINT('Ctrl Pts',(1.92526263537048,1.,-0.764740025488212));
#37675=CARTESIAN_POINT('Ctrl Pts',(1.91906491634196,1.,-0.765066729667089));
#37676=CARTESIAN_POINT('Ctrl Pts',(1.91287765805169,1.,-0.765348465884722));
#37677=CARTESIAN_POINT('Ctrl Pts',(1.90669961402356,1.,-0.765584196937919));
#37678=CARTESIAN_POINT('Ctrl Pts',(1.90052930393596,1.,-0.765772772593386));
#37679=CARTESIAN_POINT('Ctrl Pts',(1.89436577771388,1.,-0.765913193856978));
#37680=CARTESIAN_POINT('Ctrl Pts',(1.88820926433409,1.,-0.766004837062091));
#37681=CARTESIAN_POINT('Ctrl Pts',(1.88206215302561,1.,-0.766047794851865));
#37682=CARTESIAN_POINT('Ctrl Pts',(1.87592888967883,1.,-0.766042837036744));
#37683=CARTESIAN_POINT('Ctrl Pts',(1.86981398314341,1.,-0.765990708546091));
#37684=CARTESIAN_POINT('Ctrl Pts',(1.86372027063312,1.,-0.765891519092547));
#37685=CARTESIAN_POINT('Ctrl Pts',(1.85764741390394,1.,-0.765744212909319));
#37686=CARTESIAN_POINT('Ctrl Pts',(1.85158945130063,1.,-0.765545710619063));
#37687=CARTESIAN_POINT('Ctrl Pts',(1.84553698875924,1.,-0.765291664862029));
#37688=CARTESIAN_POINT('Ctrl Pts',(1.83948181064835,1.,-0.764978057881738));
#37689=CARTESIAN_POINT('Ctrl Pts',(1.83342077227142,1.,-0.764602549687853));
#37690=CARTESIAN_POINT('Ctrl Pts',(1.82735991200065,1.,-0.764165902605995));
#37691=CARTESIAN_POINT('Ctrl Pts',(1.82131873145266,1.,-0.763673465462727));
#37692=CARTESIAN_POINT('Ctrl Pts',(1.8153211840553,1.,-0.763132003836634));
#37693=CARTESIAN_POINT('Ctrl Pts',(1.80938551463965,1.,-0.762546129463938));
#37694=CARTESIAN_POINT('Ctrl Pts',(1.80351583877342,1.,-0.761915336443547));
#37695=CARTESIAN_POINT('Ctrl Pts',(1.79768986997783,1.,-0.761229695230558));
#37696=CARTESIAN_POINT('Ctrl Pts',(1.7918581561088,1.,-0.760469555880749));
#37697=CARTESIAN_POINT('Ctrl Pts',(1.78596964884604,1.,-0.75961440111019));
#37698=CARTESIAN_POINT('Ctrl Pts',(1.77999411220945,1.,-0.758650626677519));
#37699=CARTESIAN_POINT('Ctrl Pts',(1.77394167108292,1.,-0.757578264077029));
#37700=CARTESIAN_POINT('Ctrl Pts',(1.76789396002998,1.,-0.75642189602781));
#37701=CARTESIAN_POINT('Ctrl Pts',(1.76197817240128,1.,-0.755220979974462));
#37702=CARTESIAN_POINT('Ctrl Pts',(1.75631083600019,1.,-0.754009254027829));
#37703=CARTESIAN_POINT('Ctrl Pts',(1.75095139468794,1.,-0.752797683531314));
#37704=CARTESIAN_POINT('Ctrl Pts',(1.74585086852502,1.,-0.751555614164483));
#37705=CARTESIAN_POINT('Ctrl Pts',(1.74080458267114,1.,-0.75019343598125));
#37706=CARTESIAN_POINT('Ctrl Pts',(1.7355035168033,1.,-0.74858246295687));
#37707=CARTESIAN_POINT('Ctrl Pts',(1.72958533647714,1.,-0.746574710097752));
#37708=CARTESIAN_POINT('Ctrl Pts',(1.72268229916769,1.,-0.744021445433094));
#37709=CARTESIAN_POINT('Ctrl Pts',(1.71447789751001,1.,-0.74079516202821));
#37710=CARTESIAN_POINT('Ctrl Pts',(1.70473309004249,1.,-0.736799665716932));
#37711=CARTESIAN_POINT('Ctrl Pts',(1.69326921972915,1.,-0.731963238685357));
#37712=CARTESIAN_POINT('Ctrl Pts',(1.67996158451922,1.,-0.726235967982445));
#37713=CARTESIAN_POINT('Ctrl Pts',(1.66472880551777,1.,-0.71958543378795));
#37714=CARTESIAN_POINT('Ctrl Pts',(1.64752408828442,1.,-0.711993139340448));
#37715=CARTESIAN_POINT('Ctrl Pts',(1.6321654166204,1.,-0.705159151977294));
#37716=CARTESIAN_POINT('Ctrl Pts',(1.61974673471117,1.,-0.699605146398837));
#37717=CARTESIAN_POINT('Ctrl Pts',(1.61106790957619,1.,-0.69571209787897));
#37718=CARTESIAN_POINT('Ctrl Pts',(1.60662857109684,1.,-0.693717979106306));
#37719=CARTESIAN_POINT('',(2.0698113262342,0.,-0.745574324794401));
#37720=CARTESIAN_POINT('Origin',(2.11275013067528,0.,-0.61342227326009));
#37721=CARTESIAN_POINT('',(2.11275013067528,1.,-0.61342227326009));
#37722=CARTESIAN_POINT('',(2.0698113262342,1.,-0.745574324794401));
#37723=CARTESIAN_POINT('',(2.11275013067528,0.,-0.61342227326009));
#37724=CARTESIAN_POINT('Ctrl Pts',(1.7075470150345,-1.,-0.383122945602004));
#37725=CARTESIAN_POINT('Ctrl Pts',(1.7075470150345,1.,-0.383122945602004));
#37726=CARTESIAN_POINT('Ctrl Pts',(1.71231062891958,-1.,-0.384119047315542));
#37727=CARTESIAN_POINT('Ctrl Pts',(1.71231062891958,1.,-0.384119047315542));
#37728=CARTESIAN_POINT('Ctrl Pts',(1.72162022246158,-1.,-0.38607079032701));
#37729=CARTESIAN_POINT('Ctrl Pts',(1.72162022246158,1.,-0.38607079032701));
#37730=CARTESIAN_POINT('Ctrl Pts',(1.7349317097561,-1.,-0.388877023509192));
#37731=CARTESIAN_POINT('Ctrl Pts',(1.7349317097561,1.,-0.388877023509192));
#37732=CARTESIAN_POINT('Ctrl Pts',(1.75137405313962,-1.,-0.392375812294307));
#37733=CARTESIAN_POINT('Ctrl Pts',(1.75137405313962,1.,-0.392375812294307));
#37734=CARTESIAN_POINT('Ctrl Pts',(1.7697556004756,-1.,-0.39634619612042));
#37735=CARTESIAN_POINT('Ctrl Pts',(1.7697556004756,1.,-0.39634619612042));
#37736=CARTESIAN_POINT('Ctrl Pts',(1.78598826347533,-1.,-0.399919403783081));
#37737=CARTESIAN_POINT('Ctrl Pts',(1.78598826347533,1.,-0.399919403783081));
#37738=CARTESIAN_POINT('Ctrl Pts',(1.80012077176221,-1.,-0.403107976170441));
#37739=CARTESIAN_POINT('Ctrl Pts',(1.80012077176221,1.,-0.403107976170441));
#37740=CARTESIAN_POINT('Ctrl Pts',(1.81223801813988,-1.,-0.405933518411838));
#37741=CARTESIAN_POINT('Ctrl Pts',(1.81223801813988,1.,-0.405933518411838));
#37742=CARTESIAN_POINT('Ctrl Pts',(1.8224702267854,-1.,-0.408428948108534));
#37743=CARTESIAN_POINT('Ctrl Pts',(1.8224702267854,1.,-0.408428948108534));
#37744=CARTESIAN_POINT('Ctrl Pts',(1.83100408895216,-1.,-0.410641256301675));
#37745=CARTESIAN_POINT('Ctrl Pts',(1.83100408895216,1.,-0.410641256301675));
#37746=CARTESIAN_POINT('Ctrl Pts',(1.83808953475839,-1.,-0.412633125322162));
#37747=CARTESIAN_POINT('Ctrl Pts',(1.83808953475839,1.,-0.412633125322162));
#37748=CARTESIAN_POINT('Ctrl Pts',(1.8440575707371,-1.,-0.41448743825434));
#37749=CARTESIAN_POINT('Ctrl Pts',(1.8440575707371,1.,-0.41448743825434));
#37750=CARTESIAN_POINT('Ctrl Pts',(1.84929312929882,-1.,-0.416300022038864));
#37751=CARTESIAN_POINT('Ctrl Pts',(1.84929312929882,1.,-0.416300022038864));
#37752=CARTESIAN_POINT('Ctrl Pts',(1.85417632856234,-1.,-0.418164129143534));
#37753=CARTESIAN_POINT('Ctrl Pts',(1.85417632856234,1.,-0.418164129143534));
#37754=CARTESIAN_POINT('Ctrl Pts',(1.85903281096686,-1.,-0.42015728797562));
#37755=CARTESIAN_POINT('Ctrl Pts',(1.85903281096686,1.,-0.42015728797562));
#37756=CARTESIAN_POINT('Ctrl Pts',(1.86408083334028,-1.,-0.422327307418275));
#37757=CARTESIAN_POINT('Ctrl Pts',(1.86408083334028,1.,-0.422327307418275));
#37758=CARTESIAN_POINT('Ctrl Pts',(1.86937803944323,-1.,-0.424678177291359));
#37759=CARTESIAN_POINT('Ctrl Pts',(1.86937803944323,1.,-0.424678177291359));
#37760=CARTESIAN_POINT('Ctrl Pts',(1.87486989291484,-1.,-0.427183828519102));
#37761=CARTESIAN_POINT('Ctrl Pts',(1.87486989291484,1.,-0.427183828519102));
#37762=CARTESIAN_POINT('Ctrl Pts',(1.88044229001832,-1.,-0.429803062482345));
#37763=CARTESIAN_POINT('Ctrl Pts',(1.88044229001832,1.,-0.429803062482345));
#37764=CARTESIAN_POINT('Ctrl Pts',(1.88596913666793,-1.,-0.432493038548748));
#37765=CARTESIAN_POINT('Ctrl Pts',(1.88596913666793,1.,-0.432493038548748));
#37766=CARTESIAN_POINT('Ctrl Pts',(1.89136993975504,-1.,-0.435225660963383));
#37767=CARTESIAN_POINT('Ctrl Pts',(1.89136993975504,1.,-0.435225660963383));
#37768=CARTESIAN_POINT('Ctrl Pts',(1.89663648956466,-1.,-0.437995003948244));
#37769=CARTESIAN_POINT('Ctrl Pts',(1.89663648956466,1.,-0.437995003948244));
#37770=CARTESIAN_POINT('Ctrl Pts',(1.90180124389086,-1.,-0.440807833704038));
#37771=CARTESIAN_POINT('Ctrl Pts',(1.90180124389086,1.,-0.440807833704038));
#37772=CARTESIAN_POINT('Ctrl Pts',(1.90691756144898,-1.,-0.443677556849151));
#37773=CARTESIAN_POINT('Ctrl Pts',(1.90691756144898,1.,-0.443677556849151));
#37774=CARTESIAN_POINT('Ctrl Pts',(1.9120369998112,-1.,-0.446617343485711));
#37775=CARTESIAN_POINT('Ctrl Pts',(1.9120369998112,1.,-0.446617343485711));
#37776=CARTESIAN_POINT('Ctrl Pts',(1.91718342555755,-1.,-0.449632260106662));
#37777=CARTESIAN_POINT('Ctrl Pts',(1.91718342555755,1.,-0.449632260106662));
#37778=CARTESIAN_POINT('Ctrl Pts',(1.92235380648502,-1.,-0.452719478359433));
#37779=CARTESIAN_POINT('Ctrl Pts',(1.92235380648502,1.,-0.452719478359433));
#37780=CARTESIAN_POINT('Ctrl Pts',(1.92753067150476,-1.,-0.455872005174371));
#37781=CARTESIAN_POINT('Ctrl Pts',(1.92753067150476,1.,-0.455872005174371));
#37782=CARTESIAN_POINT('Ctrl Pts',(1.93269066517934,-1.,-0.459081234547926));
#37783=CARTESIAN_POINT('Ctrl Pts',(1.93269066517934,1.,-0.459081234547926));
#37784=CARTESIAN_POINT('Ctrl Pts',(1.93781486640821,-1.,-0.462340031009057));
#37785=CARTESIAN_POINT('Ctrl Pts',(1.93781486640821,1.,-0.462340031009057));
#37786=CARTESIAN_POINT('Ctrl Pts',(1.9428979419619,-1.,-0.46564546202603));
#37787=CARTESIAN_POINT('Ctrl Pts',(1.9428979419619,1.,-0.46564546202603));
#37788=CARTESIAN_POINT('Ctrl Pts',(1.94794381136514,-1.,-0.468997482913135));
#37789=CARTESIAN_POINT('Ctrl Pts',(1.94794381136514,1.,-0.468997482913135));
#37790=CARTESIAN_POINT('Ctrl Pts',(1.95296148278133,-1.,-0.472397672264072));
#37791=CARTESIAN_POINT('Ctrl Pts',(1.95296148278133,1.,-0.472397672264072));
#37792=CARTESIAN_POINT('Ctrl Pts',(1.95796111148177,-1.,-0.475848034683176));
#37793=CARTESIAN_POINT('Ctrl Pts',(1.95796111148177,1.,-0.475848034683176));
#37794=CARTESIAN_POINT('Ctrl Pts',(1.96294933055943,-1.,-0.479349583074855));
#37795=CARTESIAN_POINT('Ctrl Pts',(1.96294933055943,1.,-0.479349583074855));
#37796=CARTESIAN_POINT('Ctrl Pts',(1.96792703422362,-1.,-0.482901662120691));
#37797=CARTESIAN_POINT('Ctrl Pts',(1.96792703422362,1.,-0.482901662120691));
#37798=CARTESIAN_POINT('Ctrl Pts',(1.97289186263272,-1.,-0.486502692907659));
#37799=CARTESIAN_POINT('Ctrl Pts',(1.97289186263272,1.,-0.486502692907659));
#37800=CARTESIAN_POINT('Ctrl Pts',(1.97783973019229,-1.,-0.490150627860953));
#37801=CARTESIAN_POINT('Ctrl Pts',(1.97783973019229,1.,-0.490150627860953));
#37802=CARTESIAN_POINT('Ctrl Pts',(1.98276658761821,-1.,-0.493843476541495));
#37803=CARTESIAN_POINT('Ctrl Pts',(1.98276658761821,1.,-0.493843476541495));
#37804=CARTESIAN_POINT('Ctrl Pts',(1.98767044752932,-1.,-0.497579909545574));
#37805=CARTESIAN_POINT('Ctrl Pts',(1.98767044752932,1.,-0.497579909545574));
#37806=CARTESIAN_POINT('Ctrl Pts',(1.99255149126155,-1.,-0.501359287727146));
#37807=CARTESIAN_POINT('Ctrl Pts',(1.99255149126155,1.,-0.501359287727146));
#37808=CARTESIAN_POINT('Ctrl Pts',(1.99741107463572,-1.,-0.505181361323026));
#37809=CARTESIAN_POINT('Ctrl Pts',(1.99741107463572,1.,-0.505181361323026));
#37810=CARTESIAN_POINT('Ctrl Pts',(2.00225107134734,-1.,-0.509046069886157));
#37811=CARTESIAN_POINT('Ctrl Pts',(2.00225107134734,1.,-0.509046069886157));
#37812=CARTESIAN_POINT('Ctrl Pts',(2.00707309946949,-1.,-0.512953306961793));
#37813=CARTESIAN_POINT('Ctrl Pts',(2.00707309946949,1.,-0.512953306961793));
#37814=CARTESIAN_POINT('Ctrl Pts',(2.01187773939242,-1.,-0.516902681728687));
#37815=CARTESIAN_POINT('Ctrl Pts',(2.01187773939242,1.,-0.516902681728687));
#37816=CARTESIAN_POINT('Ctrl Pts',(2.01666477917286,-1.,-0.520893590399371));
#37817=CARTESIAN_POINT('Ctrl Pts',(2.01666477917286,1.,-0.520893590399371));
#37818=CARTESIAN_POINT('Ctrl Pts',(2.02143356304698,-1.,-0.524925318333476));
#37819=CARTESIAN_POINT('Ctrl Pts',(2.02143356304698,1.,-0.524925318333476));
#37820=CARTESIAN_POINT('Ctrl Pts',(2.0261832908329,-1.,-0.528997127241914));
#37821=CARTESIAN_POINT('Ctrl Pts',(2.0261832908329,1.,-0.528997127241914));
#37822=CARTESIAN_POINT('Ctrl Pts',(2.03091336214426,-1.,-0.533108355132977));
#37823=CARTESIAN_POINT('Ctrl Pts',(2.03091336214426,1.,-0.533108355132977));
#37824=CARTESIAN_POINT('Ctrl Pts',(2.03562362954037,-1.,-0.537258489833262));
#37825=CARTESIAN_POINT('Ctrl Pts',(2.03562362954037,1.,-0.537258489833262));
#37826=CARTESIAN_POINT('Ctrl Pts',(2.04031422690527,-1.,-0.541447120615659));
#37827=CARTESIAN_POINT('Ctrl Pts',(2.04031422690527,1.,-0.541447120615659));
#37828=CARTESIAN_POINT('Ctrl Pts',(2.04498544714588,-1.,-0.54567390381743));
#37829=CARTESIAN_POINT('Ctrl Pts',(2.04498544714588,1.,-0.54567390381743));
#37830=CARTESIAN_POINT('Ctrl Pts',(2.04963761077958,-1.,-0.549938525150295));
#37831=CARTESIAN_POINT('Ctrl Pts',(2.04963761077958,1.,-0.549938525150295));
#37832=CARTESIAN_POINT('Ctrl Pts',(2.05427091604413,-1.,-0.554240657463906));
#37833=CARTESIAN_POINT('Ctrl Pts',(2.05427091604413,1.,-0.554240657463906));
#37834=CARTESIAN_POINT('Ctrl Pts',(2.05888537756462,-1.,-0.558579940185152));
#37835=CARTESIAN_POINT('Ctrl Pts',(2.05888537756462,1.,-0.558579940185152));
#37836=CARTESIAN_POINT('Ctrl Pts',(2.06348090160589,-1.,-0.562955993082262));
#37837=CARTESIAN_POINT('Ctrl Pts',(2.06348090160589,1.,-0.562955993082262));
#37838=CARTESIAN_POINT('Ctrl Pts',(2.06805732997334,-1.,-0.567368421181087));
#37839=CARTESIAN_POINT('Ctrl Pts',(2.06805732997334,1.,-0.567368421181087));
#37840=CARTESIAN_POINT('Ctrl Pts',(2.07261449292824,-1.,-0.571816823242603));
#37841=CARTESIAN_POINT('Ctrl Pts',(2.07261449292824,1.,-0.571816823242603));
#37842=CARTESIAN_POINT('Ctrl Pts',(2.07715226767559,-1.,-0.576300797416845));
#37843=CARTESIAN_POINT('Ctrl Pts',(2.07715226767559,1.,-0.576300797416845));
#37844=CARTESIAN_POINT('Ctrl Pts',(2.08167059018418,-1.,-0.580819952108064));
#37845=CARTESIAN_POINT('Ctrl Pts',(2.08167059018418,1.,-0.580819952108064));
#37846=CARTESIAN_POINT('Ctrl Pts',(2.08616943727951,-1.,-0.585373918991617));
#37847=CARTESIAN_POINT('Ctrl Pts',(2.08616943727951,1.,-0.585373918991617));
#37848=CARTESIAN_POINT('Ctrl Pts',(2.09064881812129,-1.,-0.589962365403406));
#37849=CARTESIAN_POINT('Ctrl Pts',(2.09064881812129,1.,-0.589962365403406));
#37850=CARTESIAN_POINT('Ctrl Pts',(2.0951087622027,-1.,-0.594585006052162));
#37851=CARTESIAN_POINT('Ctrl Pts',(2.0951087622027,1.,-0.594585006052162));
#37852=CARTESIAN_POINT('Ctrl Pts',(2.0995493086477,-1.,-0.599241616420534));
#37853=CARTESIAN_POINT('Ctrl Pts',(2.0995493086477,1.,-0.599241616420534));
#37854=CARTESIAN_POINT('Ctrl Pts',(2.10397049886949,-1.,-0.60393203073603));
#37855=CARTESIAN_POINT('Ctrl Pts',(2.10397049886949,1.,-0.60393203073603));
#37856=CARTESIAN_POINT('Ctrl Pts',(2.1074919961518,-1.,-0.607711315454876));
#37857=CARTESIAN_POINT('Ctrl Pts',(2.1074919961518,1.,-0.607711315454876));
#37858=CARTESIAN_POINT('Ctrl Pts',(2.11012443807238,-1.,-0.610560911689899));
#37859=CARTESIAN_POINT('Ctrl Pts',(2.11012443807238,1.,-0.610560911689899));
#37860=CARTESIAN_POINT('Ctrl Pts',(2.11187554259986,-1.,-0.6124673655618));
#37861=CARTESIAN_POINT('Ctrl Pts',(2.11187554259986,1.,-0.6124673655618));
#37862=CARTESIAN_POINT('Ctrl Pts',(2.11275013067528,-1.,-0.61342227326009));
#37863=CARTESIAN_POINT('Ctrl Pts',(2.11275013067528,1.,-0.61342227326009));
#37864=CARTESIAN_POINT('',(1.7075470150345,1.,-0.383122945602004));
#37865=CARTESIAN_POINT('Ctrl Pts',(1.7075470150345,1.,-0.383122945602004));
#37866=CARTESIAN_POINT('Ctrl Pts',(1.71231062891958,1.,-0.384119047315542));
#37867=CARTESIAN_POINT('Ctrl Pts',(1.72162022246158,1.,-0.38607079032701));
#37868=CARTESIAN_POINT('Ctrl Pts',(1.7349317097561,1.,-0.388877023509192));
#37869=CARTESIAN_POINT('Ctrl Pts',(1.75137405313962,1.,-0.392375812294307));
#37870=CARTESIAN_POINT('Ctrl Pts',(1.7697556004756,1.,-0.39634619612042));
#37871=CARTESIAN_POINT('Ctrl Pts',(1.78598826347533,1.,-0.399919403783081));
#37872=CARTESIAN_POINT('Ctrl Pts',(1.80012077176221,1.,-0.403107976170441));
#37873=CARTESIAN_POINT('Ctrl Pts',(1.81223801813988,1.,-0.405933518411838));
#37874=CARTESIAN_POINT('Ctrl Pts',(1.8224702267854,1.,-0.408428948108534));
#37875=CARTESIAN_POINT('Ctrl Pts',(1.83100408895216,1.,-0.410641256301675));
#37876=CARTESIAN_POINT('Ctrl Pts',(1.83808953475839,1.,-0.412633125322162));
#37877=CARTESIAN_POINT('Ctrl Pts',(1.8440575707371,1.,-0.41448743825434));
#37878=CARTESIAN_POINT('Ctrl Pts',(1.84929312929882,1.,-0.416300022038864));
#37879=CARTESIAN_POINT('Ctrl Pts',(1.85417632856234,1.,-0.418164129143534));
#37880=CARTESIAN_POINT('Ctrl Pts',(1.85903281096686,1.,-0.42015728797562));
#37881=CARTESIAN_POINT('Ctrl Pts',(1.86408083334028,1.,-0.422327307418275));
#37882=CARTESIAN_POINT('Ctrl Pts',(1.86937803944323,1.,-0.424678177291359));
#37883=CARTESIAN_POINT('Ctrl Pts',(1.87486989291484,1.,-0.427183828519102));
#37884=CARTESIAN_POINT('Ctrl Pts',(1.88044229001832,1.,-0.429803062482345));
#37885=CARTESIAN_POINT('Ctrl Pts',(1.88596913666793,1.,-0.432493038548748));
#37886=CARTESIAN_POINT('Ctrl Pts',(1.89136993975504,1.,-0.435225660963383));
#37887=CARTESIAN_POINT('Ctrl Pts',(1.89663648956466,1.,-0.437995003948244));
#37888=CARTESIAN_POINT('Ctrl Pts',(1.90180124389086,1.,-0.440807833704038));
#37889=CARTESIAN_POINT('Ctrl Pts',(1.90691756144898,1.,-0.443677556849151));
#37890=CARTESIAN_POINT('Ctrl Pts',(1.9120369998112,1.,-0.446617343485711));
#37891=CARTESIAN_POINT('Ctrl Pts',(1.91718342555755,1.,-0.449632260106662));
#37892=CARTESIAN_POINT('Ctrl Pts',(1.92235380648502,1.,-0.452719478359433));
#37893=CARTESIAN_POINT('Ctrl Pts',(1.92753067150476,1.,-0.455872005174371));
#37894=CARTESIAN_POINT('Ctrl Pts',(1.93269066517934,1.,-0.459081234547926));
#37895=CARTESIAN_POINT('Ctrl Pts',(1.93781486640821,1.,-0.462340031009057));
#37896=CARTESIAN_POINT('Ctrl Pts',(1.9428979419619,1.,-0.46564546202603));
#37897=CARTESIAN_POINT('Ctrl Pts',(1.94794381136514,1.,-0.468997482913135));
#37898=CARTESIAN_POINT('Ctrl Pts',(1.95296148278133,1.,-0.472397672264072));
#37899=CARTESIAN_POINT('Ctrl Pts',(1.95796111148177,1.,-0.475848034683176));
#37900=CARTESIAN_POINT('Ctrl Pts',(1.96294933055943,1.,-0.479349583074855));
#37901=CARTESIAN_POINT('Ctrl Pts',(1.96792703422362,1.,-0.482901662120691));
#37902=CARTESIAN_POINT('Ctrl Pts',(1.97289186263272,1.,-0.486502692907659));
#37903=CARTESIAN_POINT('Ctrl Pts',(1.97783973019229,1.,-0.490150627860953));
#37904=CARTESIAN_POINT('Ctrl Pts',(1.98276658761821,1.,-0.493843476541495));
#37905=CARTESIAN_POINT('Ctrl Pts',(1.98767044752932,1.,-0.497579909545574));
#37906=CARTESIAN_POINT('Ctrl Pts',(1.99255149126155,1.,-0.501359287727146));
#37907=CARTESIAN_POINT('Ctrl Pts',(1.99741107463572,1.,-0.505181361323026));
#37908=CARTESIAN_POINT('Ctrl Pts',(2.00225107134734,1.,-0.509046069886157));
#37909=CARTESIAN_POINT('Ctrl Pts',(2.00707309946949,1.,-0.512953306961793));
#37910=CARTESIAN_POINT('Ctrl Pts',(2.01187773939242,1.,-0.516902681728687));
#37911=CARTESIAN_POINT('Ctrl Pts',(2.01666477917286,1.,-0.520893590399371));
#37912=CARTESIAN_POINT('Ctrl Pts',(2.02143356304698,1.,-0.524925318333476));
#37913=CARTESIAN_POINT('Ctrl Pts',(2.0261832908329,1.,-0.528997127241914));
#37914=CARTESIAN_POINT('Ctrl Pts',(2.03091336214426,1.,-0.533108355132977));
#37915=CARTESIAN_POINT('Ctrl Pts',(2.03562362954037,1.,-0.537258489833262));
#37916=CARTESIAN_POINT('Ctrl Pts',(2.04031422690527,1.,-0.541447120615659));
#37917=CARTESIAN_POINT('Ctrl Pts',(2.04498544714588,1.,-0.54567390381743));
#37918=CARTESIAN_POINT('Ctrl Pts',(2.04963761077958,1.,-0.549938525150295));
#37919=CARTESIAN_POINT('Ctrl Pts',(2.05427091604413,1.,-0.554240657463906));
#37920=CARTESIAN_POINT('Ctrl Pts',(2.05888537756462,1.,-0.558579940185152));
#37921=CARTESIAN_POINT('Ctrl Pts',(2.06348090160589,1.,-0.562955993082262));
#37922=CARTESIAN_POINT('Ctrl Pts',(2.06805732997334,1.,-0.567368421181087));
#37923=CARTESIAN_POINT('Ctrl Pts',(2.07261449292824,1.,-0.571816823242603));
#37924=CARTESIAN_POINT('Ctrl Pts',(2.07715226767559,1.,-0.576300797416845));
#37925=CARTESIAN_POINT('Ctrl Pts',(2.08167059018418,1.,-0.580819952108064));
#37926=CARTESIAN_POINT('Ctrl Pts',(2.08616943727951,1.,-0.585373918991617));
#37927=CARTESIAN_POINT('Ctrl Pts',(2.09064881812129,1.,-0.589962365403406));
#37928=CARTESIAN_POINT('Ctrl Pts',(2.0951087622027,1.,-0.594585006052162));
#37929=CARTESIAN_POINT('Ctrl Pts',(2.0995493086477,1.,-0.599241616420534));
#37930=CARTESIAN_POINT('Ctrl Pts',(2.10397049886949,1.,-0.60393203073603));
#37931=CARTESIAN_POINT('Ctrl Pts',(2.1074919961518,1.,-0.607711315454876));
#37932=CARTESIAN_POINT('Ctrl Pts',(2.11012443807238,1.,-0.610560911689899));
#37933=CARTESIAN_POINT('Ctrl Pts',(2.11187554259986,1.,-0.6124673655618));
#37934=CARTESIAN_POINT('Ctrl Pts',(2.11275013067528,1.,-0.61342227326009));
#37935=CARTESIAN_POINT('',(1.7075470150345,0.,-0.383122945602001));
#37936=CARTESIAN_POINT('Origin',(0.,0.,0.));
#37937=CARTESIAN_POINT('',(1.74236521665491,1.,-0.163289472382896));
#37938=CARTESIAN_POINT('Origin',(0.,1.,0.));
#37939=CARTESIAN_POINT('',(1.74236521665491,0.,-0.163289472382896));
#37940=CARTESIAN_POINT('Ctrl Pts',(2.19890268624765,-1.,-0.0694764450219582));
#37941=CARTESIAN_POINT('Ctrl Pts',(2.19890268624765,1.,-0.0694764450219582));
#37942=CARTESIAN_POINT('Ctrl Pts',(2.19777582085423,-1.,-0.0701143536325491));
#37943=CARTESIAN_POINT('Ctrl Pts',(2.19777582085423,1.,-0.0701143536325491));
#37944=CARTESIAN_POINT('Ctrl Pts',(2.19552129484002,-1.,-0.0713863779526155));
#37945=CARTESIAN_POINT('Ctrl Pts',(2.19552129484002,1.,-0.0713863779526155));
#37946=CARTESIAN_POINT('Ctrl Pts',(2.19213712013662,-1.,-0.0732830357306726));
#37947=CARTESIAN_POINT('Ctrl Pts',(2.19213712013662,1.,-0.0732830357306726));
#37948=CARTESIAN_POINT('Ctrl Pts',(2.1876201139953,-1.,-0.0757891465836149));
#37949=CARTESIAN_POINT('Ctrl Pts',(2.1876201139953,1.,-0.0757891465836149));
#37950=CARTESIAN_POINT('Ctrl Pts',(2.18196589448887,-1.,-0.0788837727685244));
#37951=CARTESIAN_POINT('Ctrl Pts',(2.18196589448887,1.,-0.0788837727685244));
#37952=CARTESIAN_POINT('Ctrl Pts',(2.176303712113,-1.,-0.0819402680872767));
#37953=CARTESIAN_POINT('Ctrl Pts',(2.176303712113,1.,-0.0819402680872767));
#37954=CARTESIAN_POINT('Ctrl Pts',(2.17063357870952,-1.,-0.0849584620835374));
#37955=CARTESIAN_POINT('Ctrl Pts',(2.17063357870952,1.,-0.0849584620835374));
#37956=CARTESIAN_POINT('Ctrl Pts',(2.16495552645014,-1.,-0.0879381291386924));
#37957=CARTESIAN_POINT('Ctrl Pts',(2.16495552645014,1.,-0.0879381291386924));
#37958=CARTESIAN_POINT('Ctrl Pts',(2.15926961544516,-1.,-0.0908789888107267));
#37959=CARTESIAN_POINT('Ctrl Pts',(2.15926961544516,1.,-0.0908789888107267));
#37960=CARTESIAN_POINT('Ctrl Pts',(2.1535759397817,-1.,-0.0937807218867645));
#37961=CARTESIAN_POINT('Ctrl Pts',(2.1535759397817,1.,-0.0937807218867645));
#37962=CARTESIAN_POINT('Ctrl Pts',(2.14787463531795,-1.,-0.096642985230546));
#37963=CARTESIAN_POINT('Ctrl Pts',(2.14787463531795,1.,-0.096642985230546));
#37964=CARTESIAN_POINT('Ctrl Pts',(2.14216588396025,-1.,-0.0994654261990917));
#37965=CARTESIAN_POINT('Ctrl Pts',(2.14216588396025,1.,-0.0994654261990917));
#37966=CARTESIAN_POINT('Ctrl Pts',(2.13644992667165,-1.,-0.102247700556101));
#37967=CARTESIAN_POINT('Ctrl Pts',(2.13644992667165,1.,-0.102247700556101));
#37968=CARTESIAN_POINT('Ctrl Pts',(2.13072704887293,-1.,-0.10498947915274));
#37969=CARTESIAN_POINT('Ctrl Pts',(2.13072704887293,1.,-0.10498947915274));
#37970=CARTESIAN_POINT('Ctrl Pts',(2.12499752307,-1.,-0.10769043523109));
#37971=CARTESIAN_POINT('Ctrl Pts',(2.12499752307,1.,-0.10769043523109));
#37972=CARTESIAN_POINT('Ctrl Pts',(2.11926155590865,-1.,-0.110350236135025));
#37973=CARTESIAN_POINT('Ctrl Pts',(2.11926155590865,1.,-0.110350236135025));
#37974=CARTESIAN_POINT('Ctrl Pts',(2.11351924490306,-1.,-0.112968534419737));
#37975=CARTESIAN_POINT('Ctrl Pts',(2.11351924490306,1.,-0.112968534419737));
#37976=CARTESIAN_POINT('Ctrl Pts',(2.10777050261309,-1.,-0.115544957687927));
#37977=CARTESIAN_POINT('Ctrl Pts',(2.10777050261309,1.,-0.115544957687927));
#37978=CARTESIAN_POINT('Ctrl Pts',(2.102015121329,-1.,-0.118079107988356));
#37979=CARTESIAN_POINT('Ctrl Pts',(2.102015121329,1.,-0.118079107988356));
#37980=CARTESIAN_POINT('Ctrl Pts',(2.0962529286773,-1.,-0.120570567965122));
#37981=CARTESIAN_POINT('Ctrl Pts',(2.0962529286773,1.,-0.120570567965122));
#37982=CARTESIAN_POINT('Ctrl Pts',(2.09048392424825,-1.,-0.123018905621083));
#37983=CARTESIAN_POINT('Ctrl Pts',(2.09048392424825,1.,-0.123018905621083));
#37984=CARTESIAN_POINT('Ctrl Pts',(2.08470840653643,-1.,-0.125423679412062));
#37985=CARTESIAN_POINT('Ctrl Pts',(2.08470840653643,1.,-0.125423679412062));
#37986=CARTESIAN_POINT('Ctrl Pts',(2.07892715110987,-1.,-0.12778444527612));
#37987=CARTESIAN_POINT('Ctrl Pts',(2.07892715110987,1.,-0.12778444527612));
#37988=CARTESIAN_POINT('Ctrl Pts',(2.07314114713063,-1.,-0.130100748328404));
#37989=CARTESIAN_POINT('Ctrl Pts',(2.07314114713063,1.,-0.130100748328404));
#37990=CARTESIAN_POINT('Ctrl Pts',(2.06735123910326,-1.,-0.132372111547711));
#37991=CARTESIAN_POINT('Ctrl Pts',(2.06735123910326,1.,-0.132372111547711));
#37992=CARTESIAN_POINT('Ctrl Pts',(2.06155781517842,-1.,-0.134598026192106));
#37993=CARTESIAN_POINT('Ctrl Pts',(2.06155781517842,1.,-0.134598026192106));
#37994=CARTESIAN_POINT('Ctrl Pts',(2.05576044414264,-1.,-0.136777941218044));
#37995=CARTESIAN_POINT('Ctrl Pts',(2.05576044414264,1.,-0.136777941218044));
#37996=CARTESIAN_POINT('Ctrl Pts',(2.04995762001328,-1.,-0.138911255368966));
#37997=CARTESIAN_POINT('Ctrl Pts',(2.04995762001328,1.,-0.138911255368966));
#37998=CARTESIAN_POINT('Ctrl Pts',(2.04414757947916,-1.,-0.140997332152546));
#37999=CARTESIAN_POINT('Ctrl Pts',(2.04414757947916,1.,-0.140997332152546));
#38000=CARTESIAN_POINT('Ctrl Pts',(2.03832911025912,-1.,-0.143035515058209));
#38001=CARTESIAN_POINT('Ctrl Pts',(2.03832911025912,1.,-0.143035515058209));
#38002=CARTESIAN_POINT('Ctrl Pts',(2.03250223739942,-1.,-0.145025140186058));
#38003=CARTESIAN_POINT('Ctrl Pts',(2.03250223739942,1.,-0.145025140186058));
#38004=CARTESIAN_POINT('Ctrl Pts',(2.02666926182017,-1.,-0.146965557332583));
#38005=CARTESIAN_POINT('Ctrl Pts',(2.02666926182017,1.,-0.146965557332583));
#38006=CARTESIAN_POINT('Ctrl Pts',(2.02083464969894,-1.,-0.148856124775337));
#38007=CARTESIAN_POINT('Ctrl Pts',(2.02083464969894,1.,-0.148856124775337));
#38008=CARTESIAN_POINT('Ctrl Pts',(2.01500291940238,-1.,-0.150696157673078));
#38009=CARTESIAN_POINT('Ctrl Pts',(2.01500291940238,1.,-0.150696157673078));
#38010=CARTESIAN_POINT('Ctrl Pts',(2.00917680318424,-1.,-0.15248488362145));
#38011=CARTESIAN_POINT('Ctrl Pts',(2.00917680318424,1.,-0.15248488362145));
#38012=CARTESIAN_POINT('Ctrl Pts',(2.00335565310543,-1.,-0.154221403049722));
#38013=CARTESIAN_POINT('Ctrl Pts',(2.00335565310543,1.,-0.154221403049722));
#38014=CARTESIAN_POINT('Ctrl Pts',(1.99753284771497,-1.,-0.155904629548784));
#38015=CARTESIAN_POINT('Ctrl Pts',(1.99753284771497,1.,-0.155904629548784));
#38016=CARTESIAN_POINT('Ctrl Pts',(1.99169810931908,-1.,-0.157533331459227));
#38017=CARTESIAN_POINT('Ctrl Pts',(1.99169810931908,1.,-0.157533331459227));
#38018=CARTESIAN_POINT('Ctrl Pts',(1.98584238283292,-1.,-0.159106226437299));
#38019=CARTESIAN_POINT('Ctrl Pts',(1.98584238283292,1.,-0.159106226437299));
#38020=CARTESIAN_POINT('Ctrl Pts',(1.97996195437559,-1.,-0.160622060784611));
#38021=CARTESIAN_POINT('Ctrl Pts',(1.97996195437559,1.,-0.160622060784611));
#38022=CARTESIAN_POINT('Ctrl Pts',(1.97406280235188,-1.,-0.162079693556289));
#38023=CARTESIAN_POINT('Ctrl Pts',(1.97406280235188,1.,-0.162079693556289));
#38024=CARTESIAN_POINT('Ctrl Pts',(1.96816512677967,-1.,-0.163478185457734));
#38025=CARTESIAN_POINT('Ctrl Pts',(1.96816512677967,1.,-0.163478185457734));
#38026=CARTESIAN_POINT('Ctrl Pts',(1.96229379940136,-1.,-0.164816568920269));
#38027=CARTESIAN_POINT('Ctrl Pts',(1.96229379940136,1.,-0.164816568920269));
#38028=CARTESIAN_POINT('Ctrl Pts',(1.9564675971873,-1.,-0.166093592002813));
#38029=CARTESIAN_POINT('Ctrl Pts',(1.9564675971873,1.,-0.166093592002813));
#38030=CARTESIAN_POINT('Ctrl Pts',(1.95069027794294,-1.,-0.167307501784476));
#38031=CARTESIAN_POINT('Ctrl Pts',(1.95069027794294,1.,-0.167307501784476));
#38032=CARTESIAN_POINT('Ctrl Pts',(1.94493757756931,-1.,-0.168455741607556));
#38033=CARTESIAN_POINT('Ctrl Pts',(1.94493757756931,1.,-0.168455741607556));
#38034=CARTESIAN_POINT('Ctrl Pts',(1.93915639211581,-1.,-0.169534904817491));
#38035=CARTESIAN_POINT('Ctrl Pts',(1.93915639211581,1.,-0.169534904817491));
#38036=CARTESIAN_POINT('Ctrl Pts',(1.93329183155539,-1.,-0.170541253116202));
#38037=CARTESIAN_POINT('Ctrl Pts',(1.93329183155539,1.,-0.170541253116202));
#38038=CARTESIAN_POINT('Ctrl Pts',(1.92731093582036,-1.,-0.171471191532988));
#38039=CARTESIAN_POINT('Ctrl Pts',(1.92731093582036,1.,-0.171471191532988));
#38040=CARTESIAN_POINT('Ctrl Pts',(1.9212233439798,-1.,-0.172321621259514));
#38041=CARTESIAN_POINT('Ctrl Pts',(1.9212233439798,1.,-0.172321621259514));
#38042=CARTESIAN_POINT('Ctrl Pts',(1.91511429159527,-1.,-0.173090695383496));
#38043=CARTESIAN_POINT('Ctrl Pts',(1.91511429159527,1.,-0.173090695383496));
#38044=CARTESIAN_POINT('Ctrl Pts',(1.90911693975267,-1.,-0.173776635257817));
#38045=CARTESIAN_POINT('Ctrl Pts',(1.90911693975267,1.,-0.173776635257817));
#38046=CARTESIAN_POINT('Ctrl Pts',(1.90335253862834,-1.,-0.174375518661085));
#38047=CARTESIAN_POINT('Ctrl Pts',(1.90335253862834,1.,-0.174375518661085));
#38048=CARTESIAN_POINT('Ctrl Pts',(1.89788101117132,-1.,-0.174879405091263));
#38049=CARTESIAN_POINT('Ctrl Pts',(1.89788101117132,1.,-0.174879405091263));
#38050=CARTESIAN_POINT('Ctrl Pts',(1.892646301985,-1.,-0.175274276190844));
#38051=CARTESIAN_POINT('Ctrl Pts',(1.892646301985,1.,-0.175274276190844));
#38052=CARTESIAN_POINT('Ctrl Pts',(1.88742606273259,-1.,-0.175538155840648));
#38053=CARTESIAN_POINT('Ctrl Pts',(1.88742606273259,1.,-0.175538155840648));
#38054=CARTESIAN_POINT('Ctrl Pts',(1.88188663145367,-1.,-0.175644148889699));
#38055=CARTESIAN_POINT('Ctrl Pts',(1.88188663145367,1.,-0.175644148889699));
#38056=CARTESIAN_POINT('Ctrl Pts',(1.87563767773588,-1.,-0.175563480746485));
#38057=CARTESIAN_POINT('Ctrl Pts',(1.87563767773588,1.,-0.175563480746485));
#38058=CARTESIAN_POINT('Ctrl Pts',(1.86828349694799,-1.,-0.175268337590758));
#38059=CARTESIAN_POINT('Ctrl Pts',(1.86828349694799,1.,-0.175268337590758));
#38060=CARTESIAN_POINT('Ctrl Pts',(1.85948367088837,-1.,-0.17473525927603));
#38061=CARTESIAN_POINT('Ctrl Pts',(1.85948367088837,1.,-0.17473525927603));
#38062=CARTESIAN_POINT('Ctrl Pts',(1.8489811319852,-1.,-0.173946627587732));
#38063=CARTESIAN_POINT('Ctrl Pts',(1.8489811319852,1.,-0.173946627587732));
#38064=CARTESIAN_POINT('Ctrl Pts',(1.83658380527692,-1.,-0.1728894428919));
#38065=CARTESIAN_POINT('Ctrl Pts',(1.83658380527692,1.,-0.1728894428919));
#38066=CARTESIAN_POINT('Ctrl Pts',(1.82215766811545,-1.,-0.171554770204119));
#38067=CARTESIAN_POINT('Ctrl Pts',(1.82215766811545,1.,-0.171554770204119));
#38068=CARTESIAN_POINT('Ctrl Pts',(1.80561530629706,-1.,-0.169936923904608));
#38069=CARTESIAN_POINT('Ctrl Pts',(1.80561530629706,1.,-0.169936923904608));
#38070=CARTESIAN_POINT('Ctrl Pts',(1.7869064998507,-1.,-0.168032772805197));
#38071=CARTESIAN_POINT('Ctrl Pts',(1.7869064998507,1.,-0.168032772805197));
#38072=CARTESIAN_POINT('Ctrl Pts',(1.77018771684844,-1.,-0.1662793551464));
#38073=CARTESIAN_POINT('Ctrl Pts',(1.77018771684844,1.,-0.1662793551464));
#38074=CARTESIAN_POINT('Ctrl Pts',(1.75666056638427,-1.,-0.164834765707159));
#38075=CARTESIAN_POINT('Ctrl Pts',(1.75666056638427,1.,-0.164834765707159));
#38076=CARTESIAN_POINT('Ctrl Pts',(1.7472034950333,-1.,-0.163814161002002));
#38077=CARTESIAN_POINT('Ctrl Pts',(1.7472034950333,1.,-0.163814161002002));
#38078=CARTESIAN_POINT('Ctrl Pts',(1.74236521665491,-1.,-0.163289472382896));
#38079=CARTESIAN_POINT('Ctrl Pts',(1.74236521665491,1.,-0.163289472382896));
#38080=CARTESIAN_POINT('',(2.19890268624765,1.,-0.0694764450219582));
#38081=CARTESIAN_POINT('Ctrl Pts',(2.19890268624765,1.,-0.0694764450219582));
#38082=CARTESIAN_POINT('Ctrl Pts',(2.19777582085423,1.,-0.0701143536325491));
#38083=CARTESIAN_POINT('Ctrl Pts',(2.19552129484002,1.,-0.0713863779526155));
#38084=CARTESIAN_POINT('Ctrl Pts',(2.19213712013662,1.,-0.0732830357306726));
#38085=CARTESIAN_POINT('Ctrl Pts',(2.1876201139953,1.,-0.0757891465836149));
#38086=CARTESIAN_POINT('Ctrl Pts',(2.18196589448887,1.,-0.0788837727685244));
#38087=CARTESIAN_POINT('Ctrl Pts',(2.176303712113,1.,-0.0819402680872767));
#38088=CARTESIAN_POINT('Ctrl Pts',(2.17063357870952,1.,-0.0849584620835374));
#38089=CARTESIAN_POINT('Ctrl Pts',(2.16495552645014,1.,-0.0879381291386924));
#38090=CARTESIAN_POINT('Ctrl Pts',(2.15926961544516,1.,-0.0908789888107267));
#38091=CARTESIAN_POINT('Ctrl Pts',(2.1535759397817,1.,-0.0937807218867645));
#38092=CARTESIAN_POINT('Ctrl Pts',(2.14787463531795,1.,-0.096642985230546));
#38093=CARTESIAN_POINT('Ctrl Pts',(2.14216588396025,1.,-0.0994654261990917));
#38094=CARTESIAN_POINT('Ctrl Pts',(2.13644992667165,1.,-0.102247700556101));
#38095=CARTESIAN_POINT('Ctrl Pts',(2.13072704887293,1.,-0.10498947915274));
#38096=CARTESIAN_POINT('Ctrl Pts',(2.12499752307,1.,-0.10769043523109));
#38097=CARTESIAN_POINT('Ctrl Pts',(2.11926155590865,1.,-0.110350236135025));
#38098=CARTESIAN_POINT('Ctrl Pts',(2.11351924490306,1.,-0.112968534419737));
#38099=CARTESIAN_POINT('Ctrl Pts',(2.10777050261309,1.,-0.115544957687927));
#38100=CARTESIAN_POINT('Ctrl Pts',(2.102015121329,1.,-0.118079107988356));
#38101=CARTESIAN_POINT('Ctrl Pts',(2.0962529286773,1.,-0.120570567965122));
#38102=CARTESIAN_POINT('Ctrl Pts',(2.09048392424825,1.,-0.123018905621083));
#38103=CARTESIAN_POINT('Ctrl Pts',(2.08470840653643,1.,-0.125423679412062));
#38104=CARTESIAN_POINT('Ctrl Pts',(2.07892715110987,1.,-0.12778444527612));
#38105=CARTESIAN_POINT('Ctrl Pts',(2.07314114713063,1.,-0.130100748328404));
#38106=CARTESIAN_POINT('Ctrl Pts',(2.06735123910326,1.,-0.132372111547711));
#38107=CARTESIAN_POINT('Ctrl Pts',(2.06155781517842,1.,-0.134598026192106));
#38108=CARTESIAN_POINT('Ctrl Pts',(2.05576044414264,1.,-0.136777941218044));
#38109=CARTESIAN_POINT('Ctrl Pts',(2.04995762001328,1.,-0.138911255368966));
#38110=CARTESIAN_POINT('Ctrl Pts',(2.04414757947916,1.,-0.140997332152546));
#38111=CARTESIAN_POINT('Ctrl Pts',(2.03832911025912,1.,-0.143035515058209));
#38112=CARTESIAN_POINT('Ctrl Pts',(2.03250223739942,1.,-0.145025140186058));
#38113=CARTESIAN_POINT('Ctrl Pts',(2.02666926182017,1.,-0.146965557332583));
#38114=CARTESIAN_POINT('Ctrl Pts',(2.02083464969894,1.,-0.148856124775337));
#38115=CARTESIAN_POINT('Ctrl Pts',(2.01500291940238,1.,-0.150696157673078));
#38116=CARTESIAN_POINT('Ctrl Pts',(2.00917680318424,1.,-0.15248488362145));
#38117=CARTESIAN_POINT('Ctrl Pts',(2.00335565310543,1.,-0.154221403049722));
#38118=CARTESIAN_POINT('Ctrl Pts',(1.99753284771497,1.,-0.155904629548784));
#38119=CARTESIAN_POINT('Ctrl Pts',(1.99169810931908,1.,-0.157533331459227));
#38120=CARTESIAN_POINT('Ctrl Pts',(1.98584238283292,1.,-0.159106226437299));
#38121=CARTESIAN_POINT('Ctrl Pts',(1.97996195437559,1.,-0.160622060784611));
#38122=CARTESIAN_POINT('Ctrl Pts',(1.97406280235188,1.,-0.162079693556289));
#38123=CARTESIAN_POINT('Ctrl Pts',(1.96816512677967,1.,-0.163478185457734));
#38124=CARTESIAN_POINT('Ctrl Pts',(1.96229379940136,1.,-0.164816568920269));
#38125=CARTESIAN_POINT('Ctrl Pts',(1.9564675971873,1.,-0.166093592002813));
#38126=CARTESIAN_POINT('Ctrl Pts',(1.95069027794294,1.,-0.167307501784476));
#38127=CARTESIAN_POINT('Ctrl Pts',(1.94493757756931,1.,-0.168455741607556));
#38128=CARTESIAN_POINT('Ctrl Pts',(1.93915639211581,1.,-0.169534904817491));
#38129=CARTESIAN_POINT('Ctrl Pts',(1.93329183155539,1.,-0.170541253116202));
#38130=CARTESIAN_POINT('Ctrl Pts',(1.92731093582036,1.,-0.171471191532988));
#38131=CARTESIAN_POINT('Ctrl Pts',(1.9212233439798,1.,-0.172321621259514));
#38132=CARTESIAN_POINT('Ctrl Pts',(1.91511429159527,1.,-0.173090695383496));
#38133=CARTESIAN_POINT('Ctrl Pts',(1.90911693975267,1.,-0.173776635257817));
#38134=CARTESIAN_POINT('Ctrl Pts',(1.90335253862834,1.,-0.174375518661085));
#38135=CARTESIAN_POINT('Ctrl Pts',(1.89788101117132,1.,-0.174879405091263));
#38136=CARTESIAN_POINT('Ctrl Pts',(1.892646301985,1.,-0.175274276190844));
#38137=CARTESIAN_POINT('Ctrl Pts',(1.88742606273259,1.,-0.175538155840648));
#38138=CARTESIAN_POINT('Ctrl Pts',(1.88188663145367,1.,-0.175644148889699));
#38139=CARTESIAN_POINT('Ctrl Pts',(1.87563767773588,1.,-0.175563480746485));
#38140=CARTESIAN_POINT('Ctrl Pts',(1.86828349694799,1.,-0.175268337590758));
#38141=CARTESIAN_POINT('Ctrl Pts',(1.85948367088837,1.,-0.17473525927603));
#38142=CARTESIAN_POINT('Ctrl Pts',(1.8489811319852,1.,-0.173946627587732));
#38143=CARTESIAN_POINT('Ctrl Pts',(1.83658380527692,1.,-0.1728894428919));
#38144=CARTESIAN_POINT('Ctrl Pts',(1.82215766811545,1.,-0.171554770204119));
#38145=CARTESIAN_POINT('Ctrl Pts',(1.80561530629706,1.,-0.169936923904608));
#38146=CARTESIAN_POINT('Ctrl Pts',(1.7869064998507,1.,-0.168032772805197));
#38147=CARTESIAN_POINT('Ctrl Pts',(1.77018771684844,1.,-0.1662793551464));
#38148=CARTESIAN_POINT('Ctrl Pts',(1.75666056638427,1.,-0.164834765707159));
#38149=CARTESIAN_POINT('Ctrl Pts',(1.7472034950333,1.,-0.163814161002002));
#38150=CARTESIAN_POINT('Ctrl Pts',(1.74236521665491,1.,-0.163289472382896));
#38151=CARTESIAN_POINT('',(2.19890268624765,0.,-0.0694764450219582));
#38152=CARTESIAN_POINT('Origin',(2.19890268624765,0.,0.0694764450219582));
#38153=CARTESIAN_POINT('',(2.19890268624765,1.,0.0694764450219582));
#38154=CARTESIAN_POINT('',(2.19890268624765,1.,-0.0694764450219582));
#38155=CARTESIAN_POINT('',(2.19890268624765,0.,0.0694764450219582));
#38156=CARTESIAN_POINT('Ctrl Pts',(1.74236521665491,-1.,0.163289472382896));
#38157=CARTESIAN_POINT('Ctrl Pts',(1.74236521665491,1.,0.163289472382896));
#38158=CARTESIAN_POINT('Ctrl Pts',(1.74720349503904,-1.,0.163814161002474));
#38159=CARTESIAN_POINT('Ctrl Pts',(1.74720349503904,1.,0.163814161002474));
#38160=CARTESIAN_POINT('Ctrl Pts',(1.75666056640041,-1.,0.164834765708484));
#38161=CARTESIAN_POINT('Ctrl Pts',(1.75666056640041,1.,0.164834765708484));
#38162=CARTESIAN_POINT('Ctrl Pts',(1.77018771687692,-1.,0.166279355148738));
#38163=CARTESIAN_POINT('Ctrl Pts',(1.77018771687692,1.,0.166279355148738));
#38164=CARTESIAN_POINT('Ctrl Pts',(1.78690649988931,-1.,0.16803277280837));
#38165=CARTESIAN_POINT('Ctrl Pts',(1.78690649988931,1.,0.16803277280837));
#38166=CARTESIAN_POINT('Ctrl Pts',(1.80561530633924,-1.,0.169936923908078));
#38167=CARTESIAN_POINT('Ctrl Pts',(1.80561530633924,1.,0.169936923908078));
#38168=CARTESIAN_POINT('Ctrl Pts',(1.82215766815414,-1.,0.171554770207306));
#38169=CARTESIAN_POINT('Ctrl Pts',(1.82215766815414,1.,0.171554770207306));
#38170=CARTESIAN_POINT('Ctrl Pts',(1.83658380530747,-1.,0.17288944289442));
#38171=CARTESIAN_POINT('Ctrl Pts',(1.83658380530747,1.,0.17288944289442));
#38172=CARTESIAN_POINT('Ctrl Pts',(1.84898113200543,-1.,0.173946627589401));
#38173=CARTESIAN_POINT('Ctrl Pts',(1.84898113200543,1.,0.173946627589401));
#38174=CARTESIAN_POINT('Ctrl Pts',(1.85948367089838,-1.,0.174735259276856));
#38175=CARTESIAN_POINT('Ctrl Pts',(1.85948367089838,1.,0.174735259276856));
#38176=CARTESIAN_POINT('Ctrl Pts',(1.86828349694972,-1.,0.1752683375909));
#38177=CARTESIAN_POINT('Ctrl Pts',(1.86828349694972,1.,0.1752683375909));
#38178=CARTESIAN_POINT('Ctrl Pts',(1.87563767773249,-1.,0.175563480746205));
#38179=CARTESIAN_POINT('Ctrl Pts',(1.87563767773249,1.,0.175563480746205));
#38180=CARTESIAN_POINT('Ctrl Pts',(1.88188663144846,-1.,0.175644148889271));
#38181=CARTESIAN_POINT('Ctrl Pts',(1.88188663144846,1.,0.175644148889271));
#38182=CARTESIAN_POINT('Ctrl Pts',(1.88742606272818,-1.,0.175538155840286));
#38183=CARTESIAN_POINT('Ctrl Pts',(1.88742606272818,1.,0.175538155840286));
#38184=CARTESIAN_POINT('Ctrl Pts',(1.89264630198279,-1.,0.175274276190664));
#38185=CARTESIAN_POINT('Ctrl Pts',(1.89264630198279,1.,0.175274276190664));
#38186=CARTESIAN_POINT('Ctrl Pts',(1.89788101117148,-1.,0.174879405091277));
#38187=CARTESIAN_POINT('Ctrl Pts',(1.89788101117148,1.,0.174879405091277));
#38188=CARTESIAN_POINT('Ctrl Pts',(1.90335253863003,-1.,0.174375518661222));
#38189=CARTESIAN_POINT('Ctrl Pts',(1.90335253863003,1.,0.174375518661222));
#38190=CARTESIAN_POINT('Ctrl Pts',(1.90911693975475,-1.,0.173776635257983));
#38191=CARTESIAN_POINT('Ctrl Pts',(1.90911693975475,1.,0.173776635257983));
#38192=CARTESIAN_POINT('Ctrl Pts',(1.91511429159681,-1.,0.173090695383619));
#38193=CARTESIAN_POINT('Ctrl Pts',(1.91511429159681,1.,0.173090695383619));
#38194=CARTESIAN_POINT('Ctrl Pts',(1.92122334398034,-1.,0.172321621259556));
#38195=CARTESIAN_POINT('Ctrl Pts',(1.92122334398034,1.,0.172321621259556));
#38196=CARTESIAN_POINT('Ctrl Pts',(1.92731093582,-1.,0.17147119153296));
#38197=CARTESIAN_POINT('Ctrl Pts',(1.92731093582,1.,0.17147119153296));
#38198=CARTESIAN_POINT('Ctrl Pts',(1.93329183155455,-1.,0.170541253116136));
#38199=CARTESIAN_POINT('Ctrl Pts',(1.93329183155455,1.,0.170541253116136));
#38200=CARTESIAN_POINT('Ctrl Pts',(1.93915639211497,-1.,0.169534904817425));
#38201=CARTESIAN_POINT('Ctrl Pts',(1.93915639211497,1.,0.169534904817425));
#38202=CARTESIAN_POINT('Ctrl Pts',(1.94493757756879,-1.,0.168455741607515));
#38203=CARTESIAN_POINT('Ctrl Pts',(1.94493757756879,1.,0.168455741607515));
#38204=CARTESIAN_POINT('Ctrl Pts',(1.95069027794286,-1.,0.167307501784469));
#38205=CARTESIAN_POINT('Ctrl Pts',(1.95069027794286,1.,0.167307501784469));
#38206=CARTESIAN_POINT('Ctrl Pts',(1.95646759718755,-1.,0.166093592002832));
#38207=CARTESIAN_POINT('Ctrl Pts',(1.95646759718755,1.,0.166093592002832));
#38208=CARTESIAN_POINT('Ctrl Pts',(1.96229379940174,-1.,0.1648165689203));
#38209=CARTESIAN_POINT('Ctrl Pts',(1.96229379940174,1.,0.1648165689203));
#38210=CARTESIAN_POINT('Ctrl Pts',(1.96816512678,-1.,0.16347818545776));
#38211=CARTESIAN_POINT('Ctrl Pts',(1.96816512678,1.,0.16347818545776));
#38212=CARTESIAN_POINT('Ctrl Pts',(1.97406280235204,-1.,0.162079693556302));
#38213=CARTESIAN_POINT('Ctrl Pts',(1.97406280235204,1.,0.162079693556302));
#38214=CARTESIAN_POINT('Ctrl Pts',(1.97996195437557,-1.,0.16062206078461));
#38215=CARTESIAN_POINT('Ctrl Pts',(1.97996195437557,1.,0.16062206078461));
#38216=CARTESIAN_POINT('Ctrl Pts',(1.98584238283279,-1.,0.159106226437288));
#38217=CARTESIAN_POINT('Ctrl Pts',(1.98584238283279,1.,0.159106226437288));
#38218=CARTESIAN_POINT('Ctrl Pts',(1.99169810931893,-1.,0.157533331459215));
#38219=CARTESIAN_POINT('Ctrl Pts',(1.99169810931893,1.,0.157533331459215));
#38220=CARTESIAN_POINT('Ctrl Pts',(1.99753284771487,-1.,0.155904629548774));
#38221=CARTESIAN_POINT('Ctrl Pts',(1.99753284771487,1.,0.155904629548774));
#38222=CARTESIAN_POINT('Ctrl Pts',(2.00335565310539,-1.,0.154221403049719));
#38223=CARTESIAN_POINT('Ctrl Pts',(2.00335565310539,1.,0.154221403049719));
#38224=CARTESIAN_POINT('Ctrl Pts',(2.00917680318426,-1.,0.152484883621452));
#38225=CARTESIAN_POINT('Ctrl Pts',(2.00917680318426,1.,0.152484883621452));
#38226=CARTESIAN_POINT('Ctrl Pts',(2.01500291940243,-1.,0.150696157673084));
#38227=CARTESIAN_POINT('Ctrl Pts',(2.01500291940243,1.,0.150696157673084));
#38228=CARTESIAN_POINT('Ctrl Pts',(2.02083464969897,-1.,0.148856124775342));
#38229=CARTESIAN_POINT('Ctrl Pts',(2.02083464969897,1.,0.148856124775342));
#38230=CARTESIAN_POINT('Ctrl Pts',(2.02666926182017,-1.,0.146965557332586));
#38231=CARTESIAN_POINT('Ctrl Pts',(2.02666926182017,1.,0.146965557332586));
#38232=CARTESIAN_POINT('Ctrl Pts',(2.03250223739941,-1.,0.145025140186058));
#38233=CARTESIAN_POINT('Ctrl Pts',(2.03250223739941,1.,0.145025140186058));
#38234=CARTESIAN_POINT('Ctrl Pts',(2.03832911025913,-1.,0.143035515058208));
#38235=CARTESIAN_POINT('Ctrl Pts',(2.03832911025913,1.,0.143035515058208));
#38236=CARTESIAN_POINT('Ctrl Pts',(2.04414757947919,-1.,0.140997332152545));
#38237=CARTESIAN_POINT('Ctrl Pts',(2.04414757947919,1.,0.140997332152545));
#38238=CARTESIAN_POINT('Ctrl Pts',(2.04995762001333,-1.,0.138911255368966));
#38239=CARTESIAN_POINT('Ctrl Pts',(2.04995762001333,1.,0.138911255368966));
#38240=CARTESIAN_POINT('Ctrl Pts',(2.0557604441427,-1.,0.136777941218044));
#38241=CARTESIAN_POINT('Ctrl Pts',(2.0557604441427,1.,0.136777941218044));
#38242=CARTESIAN_POINT('Ctrl Pts',(2.06155781517844,-1.,0.134598026192107));
#38243=CARTESIAN_POINT('Ctrl Pts',(2.06155781517844,1.,0.134598026192107));
#38244=CARTESIAN_POINT('Ctrl Pts',(2.06735123910319,-1.,0.132372111547709));
#38245=CARTESIAN_POINT('Ctrl Pts',(2.06735123910319,1.,0.132372111547709));
#38246=CARTESIAN_POINT('Ctrl Pts',(2.07314114713047,-1.,0.1301007483284));
#38247=CARTESIAN_POINT('Ctrl Pts',(2.07314114713047,1.,0.1301007483284));
#38248=CARTESIAN_POINT('Ctrl Pts',(2.07892715110967,-1.,0.127784445276116));
#38249=CARTESIAN_POINT('Ctrl Pts',(2.07892715110967,1.,0.127784445276116));
#38250=CARTESIAN_POINT('Ctrl Pts',(2.08470840653628,-1.,0.125423679412058));
#38251=CARTESIAN_POINT('Ctrl Pts',(2.08470840653628,1.,0.125423679412058));
#38252=CARTESIAN_POINT('Ctrl Pts',(2.09048392424826,-1.,0.123018905621083));
#38253=CARTESIAN_POINT('Ctrl Pts',(2.09048392424826,1.,0.123018905621083));
#38254=CARTESIAN_POINT('Ctrl Pts',(2.09625292867756,-1.,0.120570567965129));
#38255=CARTESIAN_POINT('Ctrl Pts',(2.09625292867756,1.,0.120570567965129));
#38256=CARTESIAN_POINT('Ctrl Pts',(2.10201512132945,-1.,0.118079107988368));
#38257=CARTESIAN_POINT('Ctrl Pts',(2.10201512132945,1.,0.118079107988368));
#38258=CARTESIAN_POINT('Ctrl Pts',(2.10777050261359,-1.,0.11554495768794));
#38259=CARTESIAN_POINT('Ctrl Pts',(2.10777050261359,1.,0.11554495768794));
#38260=CARTESIAN_POINT('Ctrl Pts',(2.11351924490335,-1.,0.112968534419746));
#38261=CARTESIAN_POINT('Ctrl Pts',(2.11351924490335,1.,0.112968534419746));
#38262=CARTESIAN_POINT('Ctrl Pts',(2.11926155590849,-1.,0.11035023613502));
#38263=CARTESIAN_POINT('Ctrl Pts',(2.11926155590849,1.,0.11035023613502));
#38264=CARTESIAN_POINT('Ctrl Pts',(2.12499752306927,-1.,0.107690435231068));
#38265=CARTESIAN_POINT('Ctrl Pts',(2.12499752306927,1.,0.107690435231068));
#38266=CARTESIAN_POINT('Ctrl Pts',(2.1307270488718,-1.,0.104989479152703));
#38267=CARTESIAN_POINT('Ctrl Pts',(2.1307270488718,1.,0.104989479152703));
#38268=CARTESIAN_POINT('Ctrl Pts',(2.13644992667052,-1.,0.102247700556063));
#38269=CARTESIAN_POINT('Ctrl Pts',(2.13644992667052,1.,0.102247700556063));
#38270=CARTESIAN_POINT('Ctrl Pts',(2.14216588395974,-1.,0.0994654261990741));
#38271=CARTESIAN_POINT('Ctrl Pts',(2.14216588395974,1.,0.0994654261990741));
#38272=CARTESIAN_POINT('Ctrl Pts',(2.14787463531864,-1.,0.0966429852305688));
#38273=CARTESIAN_POINT('Ctrl Pts',(2.14787463531864,1.,0.0966429852305688));
#38274=CARTESIAN_POINT('Ctrl Pts',(2.15357593978377,-1.,0.0937807218868344));
#38275=CARTESIAN_POINT('Ctrl Pts',(2.15357593978377,1.,0.0937807218868344));
#38276=CARTESIAN_POINT('Ctrl Pts',(2.15926961544808,-1.,0.0908789888108265));
#38277=CARTESIAN_POINT('Ctrl Pts',(2.15926961544808,1.,0.0908789888108265));
#38278=CARTESIAN_POINT('Ctrl Pts',(2.16495552645275,-1.,0.0879381291387821));
#38279=CARTESIAN_POINT('Ctrl Pts',(2.16495552645275,1.,0.0879381291387821));
#38280=CARTESIAN_POINT('Ctrl Pts',(2.17063357871031,-1.,0.0849584620835642));
#38281=CARTESIAN_POINT('Ctrl Pts',(2.17063357871031,1.,0.0849584620835642));
#38282=CARTESIAN_POINT('Ctrl Pts',(2.1763037121106,-1.,0.0819402680871938));
#38283=CARTESIAN_POINT('Ctrl Pts',(2.1763037121106,1.,0.0819402680871938));
#38284=CARTESIAN_POINT('Ctrl Pts',(2.18196589448304,-1.,0.0788837727683226));
#38285=CARTESIAN_POINT('Ctrl Pts',(2.18196589448304,1.,0.0788837727683226));
#38286=CARTESIAN_POINT('Ctrl Pts',(2.1876201139874,-1.,0.075789146583341));
#38287=CARTESIAN_POINT('Ctrl Pts',(2.1876201139874,1.,0.075789146583341));
#38288=CARTESIAN_POINT('Ctrl Pts',(2.19213712012956,-1.,0.0732830357304275));
#38289=CARTESIAN_POINT('Ctrl Pts',(2.19213712012956,1.,0.0732830357304275));
#38290=CARTESIAN_POINT('Ctrl Pts',(2.19552129483562,-1.,0.0713863779524626));
#38291=CARTESIAN_POINT('Ctrl Pts',(2.19552129483562,1.,0.0713863779524626));
#38292=CARTESIAN_POINT('Ctrl Pts',(2.19777582085261,-1.,0.0701143536324925));
#38293=CARTESIAN_POINT('Ctrl Pts',(2.19777582085261,1.,0.0701143536324925));
#38294=CARTESIAN_POINT('Ctrl Pts',(2.19890268624765,-1.,0.0694764450219582));
#38295=CARTESIAN_POINT('Ctrl Pts',(2.19890268624765,1.,0.0694764450219582));
#38296=CARTESIAN_POINT('',(1.74236521665491,1.,0.163289472382896));
#38297=CARTESIAN_POINT('Ctrl Pts',(1.74236521665491,1.,0.163289472382896));
#38298=CARTESIAN_POINT('Ctrl Pts',(1.74720349503904,1.,0.163814161002474));
#38299=CARTESIAN_POINT('Ctrl Pts',(1.75666056640041,1.,0.164834765708484));
#38300=CARTESIAN_POINT('Ctrl Pts',(1.77018771687692,1.,0.166279355148738));
#38301=CARTESIAN_POINT('Ctrl Pts',(1.78690649988931,1.,0.16803277280837));
#38302=CARTESIAN_POINT('Ctrl Pts',(1.80561530633924,1.,0.169936923908078));
#38303=CARTESIAN_POINT('Ctrl Pts',(1.82215766815414,1.,0.171554770207306));
#38304=CARTESIAN_POINT('Ctrl Pts',(1.83658380530747,1.,0.17288944289442));
#38305=CARTESIAN_POINT('Ctrl Pts',(1.84898113200543,1.,0.173946627589401));
#38306=CARTESIAN_POINT('Ctrl Pts',(1.85948367089838,1.,0.174735259276856));
#38307=CARTESIAN_POINT('Ctrl Pts',(1.86828349694972,1.,0.1752683375909));
#38308=CARTESIAN_POINT('Ctrl Pts',(1.87563767773249,1.,0.175563480746205));
#38309=CARTESIAN_POINT('Ctrl Pts',(1.88188663144846,1.,0.175644148889271));
#38310=CARTESIAN_POINT('Ctrl Pts',(1.88742606272818,1.,0.175538155840286));
#38311=CARTESIAN_POINT('Ctrl Pts',(1.89264630198279,1.,0.175274276190664));
#38312=CARTESIAN_POINT('Ctrl Pts',(1.89788101117148,1.,0.174879405091277));
#38313=CARTESIAN_POINT('Ctrl Pts',(1.90335253863003,1.,0.174375518661222));
#38314=CARTESIAN_POINT('Ctrl Pts',(1.90911693975475,1.,0.173776635257983));
#38315=CARTESIAN_POINT('Ctrl Pts',(1.91511429159681,1.,0.173090695383619));
#38316=CARTESIAN_POINT('Ctrl Pts',(1.92122334398034,1.,0.172321621259556));
#38317=CARTESIAN_POINT('Ctrl Pts',(1.92731093582,1.,0.17147119153296));
#38318=CARTESIAN_POINT('Ctrl Pts',(1.93329183155455,1.,0.170541253116136));
#38319=CARTESIAN_POINT('Ctrl Pts',(1.93915639211497,1.,0.169534904817425));
#38320=CARTESIAN_POINT('Ctrl Pts',(1.94493757756879,1.,0.168455741607515));
#38321=CARTESIAN_POINT('Ctrl Pts',(1.95069027794286,1.,0.167307501784469));
#38322=CARTESIAN_POINT('Ctrl Pts',(1.95646759718755,1.,0.166093592002832));
#38323=CARTESIAN_POINT('Ctrl Pts',(1.96229379940174,1.,0.1648165689203));
#38324=CARTESIAN_POINT('Ctrl Pts',(1.96816512678,1.,0.16347818545776));
#38325=CARTESIAN_POINT('Ctrl Pts',(1.97406280235204,1.,0.162079693556302));
#38326=CARTESIAN_POINT('Ctrl Pts',(1.97996195437557,1.,0.16062206078461));
#38327=CARTESIAN_POINT('Ctrl Pts',(1.98584238283279,1.,0.159106226437288));
#38328=CARTESIAN_POINT('Ctrl Pts',(1.99169810931893,1.,0.157533331459215));
#38329=CARTESIAN_POINT('Ctrl Pts',(1.99753284771487,1.,0.155904629548774));
#38330=CARTESIAN_POINT('Ctrl Pts',(2.00335565310539,1.,0.154221403049719));
#38331=CARTESIAN_POINT('Ctrl Pts',(2.00917680318426,1.,0.152484883621452));
#38332=CARTESIAN_POINT('Ctrl Pts',(2.01500291940243,1.,0.150696157673084));
#38333=CARTESIAN_POINT('Ctrl Pts',(2.02083464969897,1.,0.148856124775342));
#38334=CARTESIAN_POINT('Ctrl Pts',(2.02666926182017,1.,0.146965557332586));
#38335=CARTESIAN_POINT('Ctrl Pts',(2.03250223739941,1.,0.145025140186058));
#38336=CARTESIAN_POINT('Ctrl Pts',(2.03832911025913,1.,0.143035515058208));
#38337=CARTESIAN_POINT('Ctrl Pts',(2.04414757947919,1.,0.140997332152545));
#38338=CARTESIAN_POINT('Ctrl Pts',(2.04995762001333,1.,0.138911255368966));
#38339=CARTESIAN_POINT('Ctrl Pts',(2.0557604441427,1.,0.136777941218044));
#38340=CARTESIAN_POINT('Ctrl Pts',(2.06155781517844,1.,0.134598026192107));
#38341=CARTESIAN_POINT('Ctrl Pts',(2.06735123910319,1.,0.132372111547709));
#38342=CARTESIAN_POINT('Ctrl Pts',(2.07314114713047,1.,0.1301007483284));
#38343=CARTESIAN_POINT('Ctrl Pts',(2.07892715110967,1.,0.127784445276116));
#38344=CARTESIAN_POINT('Ctrl Pts',(2.08470840653628,1.,0.125423679412058));
#38345=CARTESIAN_POINT('Ctrl Pts',(2.09048392424826,1.,0.123018905621083));
#38346=CARTESIAN_POINT('Ctrl Pts',(2.09625292867756,1.,0.120570567965129));
#38347=CARTESIAN_POINT('Ctrl Pts',(2.10201512132945,1.,0.118079107988368));
#38348=CARTESIAN_POINT('Ctrl Pts',(2.10777050261359,1.,0.11554495768794));
#38349=CARTESIAN_POINT('Ctrl Pts',(2.11351924490335,1.,0.112968534419746));
#38350=CARTESIAN_POINT('Ctrl Pts',(2.11926155590849,1.,0.11035023613502));
#38351=CARTESIAN_POINT('Ctrl Pts',(2.12499752306927,1.,0.107690435231068));
#38352=CARTESIAN_POINT('Ctrl Pts',(2.1307270488718,1.,0.104989479152703));
#38353=CARTESIAN_POINT('Ctrl Pts',(2.13644992667052,1.,0.102247700556063));
#38354=CARTESIAN_POINT('Ctrl Pts',(2.14216588395974,1.,0.0994654261990741));
#38355=CARTESIAN_POINT('Ctrl Pts',(2.14787463531864,1.,0.0966429852305688));
#38356=CARTESIAN_POINT('Ctrl Pts',(2.15357593978377,1.,0.0937807218868344));
#38357=CARTESIAN_POINT('Ctrl Pts',(2.15926961544808,1.,0.0908789888108265));
#38358=CARTESIAN_POINT('Ctrl Pts',(2.16495552645275,1.,0.0879381291387821));
#38359=CARTESIAN_POINT('Ctrl Pts',(2.17063357871031,1.,0.0849584620835642));
#38360=CARTESIAN_POINT('Ctrl Pts',(2.1763037121106,1.,0.0819402680871938));
#38361=CARTESIAN_POINT('Ctrl Pts',(2.18196589448304,1.,0.0788837727683226));
#38362=CARTESIAN_POINT('Ctrl Pts',(2.1876201139874,1.,0.075789146583341));
#38363=CARTESIAN_POINT('Ctrl Pts',(2.19213712012956,1.,0.0732830357304275));
#38364=CARTESIAN_POINT('Ctrl Pts',(2.19552129483562,1.,0.0713863779524626));
#38365=CARTESIAN_POINT('Ctrl Pts',(2.19777582085261,1.,0.0701143536324925));
#38366=CARTESIAN_POINT('Ctrl Pts',(2.19890268624765,1.,0.0694764450219582));
#38367=CARTESIAN_POINT('',(1.74236521665491,0.,0.163289472382896));
#38368=CARTESIAN_POINT('Origin',(0.,1.,0.));
#38369=CARTESIAN_POINT('Origin',(0.,1.,0.));
#38370=CARTESIAN_POINT('Origin',(0.,0.,0.));
#38371=CARTESIAN_POINT('',(0.,0.,0.));
#38372=CARTESIAN_POINT('Origin',(0.7,0.,0.25));
#38373=CARTESIAN_POINT('',(0.7,0.16,0.4));
#38374=CARTESIAN_POINT('',(0.7,0.2,0.36));
#38375=CARTESIAN_POINT('',(0.7,0.1675,0.3925));
#38376=CARTESIAN_POINT('',(0.7,-0.16,0.4));
#38377=CARTESIAN_POINT('',(0.7,0.,0.4));
#38378=CARTESIAN_POINT('',(0.7,-0.2,0.36));
#38379=CARTESIAN_POINT('',(0.7,-0.1675,0.3925));
#38380=CARTESIAN_POINT('',(0.7,-0.2,0.04));
#38381=CARTESIAN_POINT('',(0.7,-0.2,0.125));
#38382=CARTESIAN_POINT('',(0.7,-0.16,0.));
#38383=CARTESIAN_POINT('',(0.7,-0.1925,0.0325));
#38384=CARTESIAN_POINT('',(0.7,0.16,0.));
#38385=CARTESIAN_POINT('',(0.7,0.,0.));
#38386=CARTESIAN_POINT('',(0.7,0.2,0.04));
#38387=CARTESIAN_POINT('',(0.7,0.1925,0.0325));
#38388=CARTESIAN_POINT('',(0.7,0.2,0.125));
#38389=CARTESIAN_POINT('Origin',(-0.4,-0.18,0.02));
#38390=CARTESIAN_POINT('',(-0.7,-0.2,0.04));
#38391=CARTESIAN_POINT('',(-0.4,-0.2,0.04));
#38392=CARTESIAN_POINT('',(-0.7,-0.16,0.));
#38393=CARTESIAN_POINT('',(-0.7,-0.1925,0.0325));
#38394=CARTESIAN_POINT('',(-0.4,-0.16,0.));
#38395=CARTESIAN_POINT('Origin',(-0.8,-0.2,0.));
#38396=CARTESIAN_POINT('',(-0.7,-0.2,0.36));
#38397=CARTESIAN_POINT('',(-0.4,-0.2,0.36));
#38398=CARTESIAN_POINT('',(-0.7,-0.2,0.125));
#38399=CARTESIAN_POINT('Origin',(-0.4,-0.18,0.38));
#38400=CARTESIAN_POINT('',(-0.7,-0.16,0.4));
#38401=CARTESIAN_POINT('',(-0.4,-0.16,0.4));
#38402=CARTESIAN_POINT('',(-0.7,-0.1675,0.3925));
#38403=CARTESIAN_POINT('Origin',(0.,0.,0.4));
#38404=CARTESIAN_POINT('',(-0.7,0.16,0.4));
#38405=CARTESIAN_POINT('',(0.4,0.16,0.4));
#38406=CARTESIAN_POINT('',(-0.7,0.,0.4));
#38407=CARTESIAN_POINT('Origin',(-0.7,0.,0.25));
#38408=CARTESIAN_POINT('',(-0.7,0.2,0.36));
#38409=CARTESIAN_POINT('',(-0.7,0.1675,0.3925));
#38410=CARTESIAN_POINT('',(-0.7,0.2,0.04));
#38411=CARTESIAN_POINT('',(-0.7,0.2,0.125));
#38412=CARTESIAN_POINT('',(-0.7,0.16,0.));
#38413=CARTESIAN_POINT('',(-0.7,0.1925,0.0325));
#38414=CARTESIAN_POINT('',(-0.7,0.,0.));
#38415=CARTESIAN_POINT('Origin',(0.4,0.18,0.38));
#38416=CARTESIAN_POINT('',(0.4,0.2,0.36));
#38417=CARTESIAN_POINT('Origin',(0.8,0.2,0.));
#38418=CARTESIAN_POINT('',(0.4,0.2,0.04));
#38419=CARTESIAN_POINT('Origin',(0.4,0.18,0.02));
#38420=CARTESIAN_POINT('',(0.4,0.16,0.));
#38421=CARTESIAN_POINT('Origin',(0.,0.,0.));
#38422=CARTESIAN_POINT('',(0.,0.,0.));
#38423=CARTESIAN_POINT('',(0.,0.,0.));
#38424=CARTESIAN_POINT('Origin',(18.,4.6,9.));
#38425=CARTESIAN_POINT('',(17.835,4.6,9.));
#38426=CARTESIAN_POINT('Origin',(18.,4.6,9.));
#38427=CARTESIAN_POINT('',(17.835,6.,9.));
#38428=CARTESIAN_POINT('',(17.835,4.6,9.));
#38429=CARTESIAN_POINT('Origin',(18.,6.,9.));
#38430=CARTESIAN_POINT('Origin',(18.,4.6,9.));
#38431=CARTESIAN_POINT('Origin',(17.7,0.6,7.));
#38432=CARTESIAN_POINT('',(17.7,2.6,8.04606079858305));
#38433=CARTESIAN_POINT('',(17.7,0.6,8.04606079858305));
#38434=CARTESIAN_POINT('',(17.7,-3.6,8.04606079858305));
#38435=CARTESIAN_POINT('',(17.7,2.6,8.35));
#38436=CARTESIAN_POINT('',(17.7,2.6,8.35));
#38437=CARTESIAN_POINT('',(17.7,0.6,8.35));
#38438=CARTESIAN_POINT('',(17.7,0.6,8.35));
#38439=CARTESIAN_POINT('',(17.7,0.6,8.35));
#38440=CARTESIAN_POINT('Origin',(18.,0.6,7.675));
#38441=CARTESIAN_POINT('',(18.3,0.6,8.04606079858305));
#38442=CARTESIAN_POINT('Origin',(18.,0.6,9.));
#38443=CARTESIAN_POINT('',(18.3,0.6,8.35));
#38444=CARTESIAN_POINT('',(18.3,0.6,8.35));
#38445=CARTESIAN_POINT('',(18.3,0.6,7.));
#38446=CARTESIAN_POINT('Origin',(18.3,0.6,8.35));
#38447=CARTESIAN_POINT('',(18.3,2.6,8.04606079858305));
#38448=CARTESIAN_POINT('',(18.3,-3.6,8.04606079858305));
#38449=CARTESIAN_POINT('',(18.3,2.6,8.35));
#38450=CARTESIAN_POINT('',(18.3,0.6,8.35));
#38451=CARTESIAN_POINT('',(18.3,2.6,7.));
#38452=CARTESIAN_POINT('Origin',(17.7,0.6,8.35));
#38453=CARTESIAN_POINT('',(18.3,2.6,8.35));
#38454=CARTESIAN_POINT('Origin',(18.,2.6,7.675));
#38455=CARTESIAN_POINT('Origin',(18.,2.6,9.));
#38456=CARTESIAN_POINT('Origin',(18.,-0.4,9.));
#38457=CARTESIAN_POINT('',(16.7,-0.4,9.));
#38458=CARTESIAN_POINT('Origin',(18.,-0.4,9.));
#38459=CARTESIAN_POINT('',(17.,-0.4,9.));
#38460=CARTESIAN_POINT('Origin',(18.,-0.4,9.));
#38461=CARTESIAN_POINT('Origin',(18.,-0.8,9.));
#38462=CARTESIAN_POINT('',(16.7,-0.8,9.));
#38463=CARTESIAN_POINT('Origin',(18.,-0.8,9.));
#38464=CARTESIAN_POINT('',(17.,-0.8,9.));
#38465=CARTESIAN_POINT('Origin',(18.,-0.8,9.));
#38466=CARTESIAN_POINT('Origin',(18.,-0.8,9.));
#38467=CARTESIAN_POINT('',(16.7,-0.8,9.));
#38468=CARTESIAN_POINT('Origin',(18.,-3.6,9.));
#38469=CARTESIAN_POINT('',(17.,-3.6,9.));
#38470=CARTESIAN_POINT('',(17.,-3.6,9.));
#38471=CARTESIAN_POINT('Origin',(18.,-3.6,9.));
#38472=CARTESIAN_POINT('Origin',(18.,-3.6,9.));
#38473=CARTESIAN_POINT('',(17.,6.,9.));
#38474=CARTESIAN_POINT('Origin',(18.,6.,9.));
#38475=CARTESIAN_POINT('',(17.,-3.6,9.));
#38476=CARTESIAN_POINT('Origin',(18.,6.,9.));
#38477=CARTESIAN_POINT('Origin',(18.,-3.6,9.));
#38478=CARTESIAN_POINT('',(0.,0.,0.));
#38479=CARTESIAN_POINT('Origin',(18.,-0.4,9.));
#38480=CARTESIAN_POINT('',(16.995,0.,9.));
#38481=CARTESIAN_POINT('Origin',(18.,0.,9.));
#38482=CARTESIAN_POINT('',(16.995,-0.4,9.));
#38483=CARTESIAN_POINT('',(16.995,-0.4,9.));
#38484=CARTESIAN_POINT('Origin',(18.,-0.4,9.));
#38485=CARTESIAN_POINT('Origin',(18.,-0.4,9.));
#38486=CARTESIAN_POINT('',(16.7,0.,9.));
#38487=CARTESIAN_POINT('Origin',(18.,0.,9.));
#38488=CARTESIAN_POINT('',(16.7,-0.4,9.));
#38489=CARTESIAN_POINT('',(16.7,-0.4,9.));
#38490=CARTESIAN_POINT('Origin',(18.,-0.4,9.));
#38491=CARTESIAN_POINT('Origin',(18.,0.,9.));
#38492=CARTESIAN_POINT('Origin',(18.,-0.4,9.));
#38493=CARTESIAN_POINT('',(0.,0.,0.));
#38494=CARTESIAN_POINT('Origin',(18.,-2.8,9.));
#38495=CARTESIAN_POINT('',(16.995,-2.2,9.));
#38496=CARTESIAN_POINT('Origin',(18.,-2.2,9.));
#38497=CARTESIAN_POINT('',(16.995,-2.8,9.));
#38498=CARTESIAN_POINT('',(16.995,-2.8,9.));
#38499=CARTESIAN_POINT('Origin',(18.,-2.8,9.));
#38500=CARTESIAN_POINT('Origin',(18.,-2.8,9.));
#38501=CARTESIAN_POINT('',(16.7,-2.2,9.));
#38502=CARTESIAN_POINT('Origin',(18.,-2.2,9.));
#38503=CARTESIAN_POINT('',(16.7,-2.8,9.));
#38504=CARTESIAN_POINT('',(16.7,-2.8,9.));
#38505=CARTESIAN_POINT('Origin',(18.,-2.8,9.));
#38506=CARTESIAN_POINT('Origin',(18.,-2.2,9.));
#38507=CARTESIAN_POINT('Origin',(18.,-2.8,9.));
#38508=CARTESIAN_POINT('',(0.,0.,0.));
#38509=CARTESIAN_POINT('Origin',(18.,-3.2,9.99));
#38510=CARTESIAN_POINT('',(18.17298843892,-3.31905880899793,9.99));
#38511=CARTESIAN_POINT('',(18.17298843892,-3.08094119100207,9.99));
#38512=CARTESIAN_POINT('',(18.17298843892,-3.6,9.99));
#38513=CARTESIAN_POINT('Origin',(18.,-3.2,9.99));
#38514=CARTESIAN_POINT('Origin',(18.,-3.2,9.99));
#38515=CARTESIAN_POINT('',(17.82701156108,-3.31905880899793,9.99));
#38516=CARTESIAN_POINT('Ctrl Pts',(17.82701156108,-3.31905880899793,9.99));
#38517=CARTESIAN_POINT('Ctrl Pts',(17.8344051346887,-3.3298014223953,9.99129192197638));
#38518=CARTESIAN_POINT('Ctrl Pts',(17.8427028612744,-3.33968770937275,9.99265394943905));
#38519=CARTESIAN_POINT('Ctrl Pts',(17.8701079261549,-3.36709277425327,9.9967480843909));
#38520=CARTESIAN_POINT('Ctrl Pts',(17.8936698322407,-3.38324205633295,9.99969589327638));
#38521=CARTESIAN_POINT('Ctrl Pts',(17.9453870953676,-3.40469779396491,10.0038502947236));
#38522=CARTESIAN_POINT('Ctrl Pts',(17.9735487691701,-3.41,10.005));
#38523=CARTESIAN_POINT('Ctrl Pts',(18.0264512308299,-3.41,10.005));
#38524=CARTESIAN_POINT('Ctrl Pts',(18.0546129046324,-3.40469779396491,10.0038502947236));
#38525=CARTESIAN_POINT('Ctrl Pts',(18.1063301677593,-3.38324205633295,9.99969589327638));
#38526=CARTESIAN_POINT('Ctrl Pts',(18.1298920738451,-3.36709277425327,9.9967480843909));
#38527=CARTESIAN_POINT('Ctrl Pts',(18.1572971387256,-3.33968770937275,9.99265394943905));
#38528=CARTESIAN_POINT('Ctrl Pts',(18.1655948653113,-3.3298014223953,9.99129192197638));
#38529=CARTESIAN_POINT('Ctrl Pts',(18.17298843892,-3.31905880899793,9.99));
#38530=CARTESIAN_POINT('',(17.79,-3.2,9.99));
#38531=CARTESIAN_POINT('Origin',(18.,-3.2,9.99));
#38532=CARTESIAN_POINT('',(17.79,-3.2,10.38416039533));
#38533=CARTESIAN_POINT('',(17.79,-3.2,9.99));
#38534=CARTESIAN_POINT('',(18.21,-3.2,10.38416039533));
#38535=CARTESIAN_POINT('Ctrl Pts',(18.21,-3.2,10.38416039533));
#38536=CARTESIAN_POINT('Ctrl Pts',(18.21,-3.22641116018715,10.38416039533));
#38537=CARTESIAN_POINT('Ctrl Pts',(18.2047135491119,-3.2545550596171,10.3849944296993));
#38538=CARTESIAN_POINT('Ctrl Pts',(18.1832699958585,-3.30628264999174,10.3879947099895));
#38539=CARTESIAN_POINT('Ctrl Pts',(18.1671150376064,-3.32986981049193,10.3901162943626));
#38540=CARTESIAN_POINT('Ctrl Pts',(18.1298701351968,-3.36711471290157,10.394089123191));
#38541=CARTESIAN_POINT('Ctrl Pts',(18.1062828345902,-3.38326992585508,10.3962002442067));
#38542=CARTESIAN_POINT('Ctrl Pts',(18.0545547656039,-3.40471366447292,10.3991765222353));
#38543=CARTESIAN_POINT('Ctrl Pts',(18.0264106996808,-3.41,10.4));
#38544=CARTESIAN_POINT('Ctrl Pts',(17.9735893003192,-3.41,10.4));
#38545=CARTESIAN_POINT('Ctrl Pts',(17.9454452343961,-3.40471366447292,10.3991765222353));
#38546=CARTESIAN_POINT('Ctrl Pts',(17.8937171654098,-3.38326992585508,10.3962002442067));
#38547=CARTESIAN_POINT('Ctrl Pts',(17.8701298648032,-3.36711471290157,10.394089123191));
#38548=CARTESIAN_POINT('Ctrl Pts',(17.8328849623936,-3.32986981049193,10.3901162943626));
#38549=CARTESIAN_POINT('Ctrl Pts',(17.8167300041415,-3.30628264999174,10.3879947099895));
#38550=CARTESIAN_POINT('Ctrl Pts',(17.7952864508881,-3.2545550596171,10.3849944296993));
#38551=CARTESIAN_POINT('Ctrl Pts',(17.79,-3.22641116018715,10.38416039533));
#38552=CARTESIAN_POINT('Ctrl Pts',(17.79,-3.2,10.38416039533));
#38553=CARTESIAN_POINT('Ctrl Pts',(17.79,-3.2,10.38416039533));
#38554=CARTESIAN_POINT('Ctrl Pts',(17.79,-3.17358883981285,10.38416039533));
#38555=CARTESIAN_POINT('Ctrl Pts',(17.7952864508881,-3.1454449403829,10.3849944296993));
#38556=CARTESIAN_POINT('Ctrl Pts',(17.8167300041415,-3.09371735000826,10.3879947099895));
#38557=CARTESIAN_POINT('Ctrl Pts',(17.8328849623936,-3.07013018950808,10.3901162943626));
#38558=CARTESIAN_POINT('Ctrl Pts',(17.8701298648032,-3.03288528709843,10.394089123191));
#38559=CARTESIAN_POINT('Ctrl Pts',(17.8937171654098,-3.01673007414492,10.3962002442067));
#38560=CARTESIAN_POINT('Ctrl Pts',(17.9454452343961,-2.99528633552708,10.3991765222353));
#38561=CARTESIAN_POINT('Ctrl Pts',(17.9735893003192,-2.99,10.4));
#38562=CARTESIAN_POINT('Ctrl Pts',(18.0264106996808,-2.99,10.4));
#38563=CARTESIAN_POINT('Ctrl Pts',(18.0545547656039,-2.99528633552708,10.3991765222353));
#38564=CARTESIAN_POINT('Ctrl Pts',(18.1062828345902,-3.01673007414492,10.3962002442067));
#38565=CARTESIAN_POINT('Ctrl Pts',(18.1298701351968,-3.03288528709843,10.394089123191));
#38566=CARTESIAN_POINT('Ctrl Pts',(18.1671150376064,-3.07013018950807,10.3901162943626));
#38567=CARTESIAN_POINT('Ctrl Pts',(18.1832699958585,-3.09371735000826,10.3879947099895));
#38568=CARTESIAN_POINT('Ctrl Pts',(18.2047135491119,-3.1454449403829,10.3849944296993));
#38569=CARTESIAN_POINT('Ctrl Pts',(18.21,-3.17358883981285,10.38416039533));
#38570=CARTESIAN_POINT('Ctrl Pts',(18.21,-3.2,10.38416039533));
#38571=CARTESIAN_POINT('',(17.82701156108,-3.08094119100207,9.99));
#38572=CARTESIAN_POINT('Origin',(18.,-3.2,9.99));
#38573=CARTESIAN_POINT('Ctrl Pts',(18.17298843892,-3.08094119100207,9.99));
#38574=CARTESIAN_POINT('Ctrl Pts',(18.1655948653113,-3.0701985776047,9.99129192197638));
#38575=CARTESIAN_POINT('Ctrl Pts',(18.1572971387256,-3.06031229062725,9.99265394943905));
#38576=CARTESIAN_POINT('Ctrl Pts',(18.1298920738451,-3.03290722574673,9.9967480843909));
#38577=CARTESIAN_POINT('Ctrl Pts',(18.1063301677593,-3.01675794366705,9.99969589327638));
#38578=CARTESIAN_POINT('Ctrl Pts',(18.0546129046324,-2.99530220603509,10.0038502947236));
#38579=CARTESIAN_POINT('Ctrl Pts',(18.0264512308299,-2.99,10.005));
#38580=CARTESIAN_POINT('Ctrl Pts',(17.9735487691701,-2.99,10.005));
#38581=CARTESIAN_POINT('Ctrl Pts',(17.9453870953676,-2.99530220603509,10.0038502947236));
#38582=CARTESIAN_POINT('Ctrl Pts',(17.8936698322407,-3.01675794366705,9.99969589327638));
#38583=CARTESIAN_POINT('Ctrl Pts',(17.8701079261549,-3.03290722574673,9.9967480843909));
#38584=CARTESIAN_POINT('Ctrl Pts',(17.8427028612744,-3.06031229062725,9.99265394943905));
#38585=CARTESIAN_POINT('Ctrl Pts',(17.8344051346887,-3.0701985776047,9.99129192197638));
#38586=CARTESIAN_POINT('Ctrl Pts',(17.82701156108,-3.08094119100207,9.99));
#38587=CARTESIAN_POINT('Origin',(18.,-3.2,9.99));
#38588=CARTESIAN_POINT('',(17.82701156108,-3.6,9.99));
#38589=CARTESIAN_POINT('Origin',(18.,-3.6,9.));
#38590=CARTESIAN_POINT('',(16.995,-2.8,9.));
#38591=CARTESIAN_POINT('Origin',(18.,-2.8,9.));
#38592=CARTESIAN_POINT('',(16.995,-3.6,9.));
#38593=CARTESIAN_POINT('',(16.995,-3.6,9.));
#38594=CARTESIAN_POINT('Origin',(18.,-3.6,9.));
#38595=CARTESIAN_POINT('Origin',(18.,-3.6,9.));
#38596=CARTESIAN_POINT('',(16.6,-2.8,9.));
#38597=CARTESIAN_POINT('Origin',(18.,-2.8,9.));
#38598=CARTESIAN_POINT('',(16.6,-3.6,9.));
#38599=CARTESIAN_POINT('',(16.6,-3.6,9.));
#38600=CARTESIAN_POINT('Origin',(18.,-3.6,9.));
#38601=CARTESIAN_POINT('Origin',(18.,-2.8,9.));
#38602=CARTESIAN_POINT('Origin',(18.,-3.6,9.));
#38603=CARTESIAN_POINT('',(0.,0.,0.));
#38604=CARTESIAN_POINT('Origin',(18.,3.2,9.));
#38605=CARTESIAN_POINT('',(16.995,4.2,9.));
#38606=CARTESIAN_POINT('Origin',(18.,4.2,9.));
#38607=CARTESIAN_POINT('',(16.995,3.2,9.));
#38608=CARTESIAN_POINT('',(16.995,3.2,9.));
#38609=CARTESIAN_POINT('Origin',(18.,3.2,9.));
#38610=CARTESIAN_POINT('Origin',(18.,3.2,9.));
#38611=CARTESIAN_POINT('',(16.6,4.2,9.));
#38612=CARTESIAN_POINT('Origin',(18.,4.2,9.));
#38613=CARTESIAN_POINT('',(16.6,3.2,9.));
#38614=CARTESIAN_POINT('',(16.6,3.2,9.));
#38615=CARTESIAN_POINT('Origin',(18.,3.2,9.));
#38616=CARTESIAN_POINT('Origin',(18.,4.2,9.));
#38617=CARTESIAN_POINT('Origin',(18.,3.2,9.));
#38618=CARTESIAN_POINT('',(0.,0.,0.));
#38619=CARTESIAN_POINT('Origin',(18.,5.5,9.));
#38620=CARTESIAN_POINT('',(16.995,6.,9.));
#38621=CARTESIAN_POINT('Origin',(18.,6.,9.));
#38622=CARTESIAN_POINT('',(16.995,5.5,9.));
#38623=CARTESIAN_POINT('',(16.995,5.5,9.));
#38624=CARTESIAN_POINT('Origin',(18.,5.5,9.));
#38625=CARTESIAN_POINT('Origin',(18.,5.5,9.));
#38626=CARTESIAN_POINT('',(16.6,6.,9.));
#38627=CARTESIAN_POINT('Origin',(18.,6.,9.));
#38628=CARTESIAN_POINT('',(16.6,5.5,9.));
#38629=CARTESIAN_POINT('',(16.6,5.5,9.));
#38630=CARTESIAN_POINT('Origin',(18.,5.5,9.));
#38631=CARTESIAN_POINT('Origin',(18.,6.,9.));
#38632=CARTESIAN_POINT('Origin',(18.,5.5,9.));
#38633=CARTESIAN_POINT('',(0.,0.,0.));
#38634=CARTESIAN_POINT('Origin',(18.,4.8,9.99));
#38635=CARTESIAN_POINT('',(18.1410673597966,4.64443650813894,9.99));
#38636=CARTESIAN_POINT('',(18.1410673597966,4.95556349186105,9.99));
#38637=CARTESIAN_POINT('',(18.1410673597966,4.2,9.99));
#38638=CARTESIAN_POINT('Origin',(18.,4.8,9.99));
#38639=CARTESIAN_POINT('Origin',(18.,4.8,9.99));
#38640=CARTESIAN_POINT('',(17.8589326402034,4.64443650813894,9.99));
#38641=CARTESIAN_POINT('Ctrl Pts',(17.8589326402034,4.64443650813895,9.99));
#38642=CARTESIAN_POINT('Ctrl Pts',(17.8761816433018,4.6287948476368,9.99245784982447));
#38643=CARTESIAN_POINT('Ctrl Pts',(17.8970013568903,4.61537595666898,9.99493819304946));
#38644=CARTESIAN_POINT('Ctrl Pts',(17.9453858856016,4.59530253627557,9.99884449237241));
#38645=CARTESIAN_POINT('Ctrl Pts',(17.9735479263176,4.59,10.));
#38646=CARTESIAN_POINT('Ctrl Pts',(18.0264520736824,4.59,10.));
#38647=CARTESIAN_POINT('Ctrl Pts',(18.0546141143984,4.59530253627557,9.99884449237241));
#38648=CARTESIAN_POINT('Ctrl Pts',(18.1029986431097,4.61537595666898,9.99493819304946));
#38649=CARTESIAN_POINT('Ctrl Pts',(18.1238183566982,4.62879484763679,9.99245784982447));
#38650=CARTESIAN_POINT('Ctrl Pts',(18.1410673597966,4.64443650813894,9.99));
#38651=CARTESIAN_POINT('',(17.79,4.8,9.99));
#38652=CARTESIAN_POINT('Origin',(18.,4.8,9.99));
#38653=CARTESIAN_POINT('',(17.79,4.8,10.4852272553384));
#38654=CARTESIAN_POINT('',(17.79,4.8,9.99));
#38655=CARTESIAN_POINT('',(18.21,4.8,10.4852272553384));
#38656=CARTESIAN_POINT('Ctrl Pts',(18.21,4.8,10.4852272553384));
#38657=CARTESIAN_POINT('Ctrl Pts',(18.21,4.77359447307555,10.4852272553384));
#38658=CARTESIAN_POINT('Ctrl Pts',(18.2047157372696,4.74545292590929,10.4860041595441));
#38659=CARTESIAN_POINT('Ctrl Pts',(18.1832737630363,4.69372373109487,10.4888007328232));
#38660=CARTESIAN_POINT('Ctrl Pts',(18.1671179239704,4.67013307587204,10.4907789715758));
#38661=CARTESIAN_POINT('Ctrl Pts',(18.1298671698874,4.63288232178902,10.4944848114133));
#38662=CARTESIAN_POINT('Ctrl Pts',(18.1062764083058,4.61672628999865,10.4964545565713));
#38663=CARTESIAN_POINT('Ctrl Pts',(18.0545468514059,4.59528417517378,10.4992316551565));
#38664=CARTESIAN_POINT('Ctrl Pts',(18.0264051785093,4.59,10.5));
#38665=CARTESIAN_POINT('Ctrl Pts',(17.9735948214907,4.59,10.5));
#38666=CARTESIAN_POINT('Ctrl Pts',(17.9454531485941,4.59528417517378,10.4992316551565));
#38667=CARTESIAN_POINT('Ctrl Pts',(17.8937235916942,4.61672628999865,10.4964545565713));
#38668=CARTESIAN_POINT('Ctrl Pts',(17.8701328301126,4.63288232178902,10.4944848114133));
#38669=CARTESIAN_POINT('Ctrl Pts',(17.8328820760296,4.67013307587204,10.4907789715758));
#38670=CARTESIAN_POINT('Ctrl Pts',(17.8167262369637,4.69372373109487,10.4888007328232));
#38671=CARTESIAN_POINT('Ctrl Pts',(17.7952842627304,4.74545292590929,10.4860041595441));
#38672=CARTESIAN_POINT('Ctrl Pts',(17.79,4.77359447307555,10.4852272553384));
#38673=CARTESIAN_POINT('Ctrl Pts',(17.79,4.8,10.4852272553384));
#38674=CARTESIAN_POINT('Ctrl Pts',(17.79,4.8,10.4852272553384));
#38675=CARTESIAN_POINT('Ctrl Pts',(17.79,4.82640552692445,10.4852272553384));
#38676=CARTESIAN_POINT('Ctrl Pts',(17.7952842627304,4.85454707409071,10.4860041595441));
#38677=CARTESIAN_POINT('Ctrl Pts',(17.8167262369637,4.90627626890513,10.4888007328232));
#38678=CARTESIAN_POINT('Ctrl Pts',(17.8328820760296,4.92986692412796,10.4907789715758));
#38679=CARTESIAN_POINT('Ctrl Pts',(17.8701328301126,4.96711767821098,10.4944848114133));
#38680=CARTESIAN_POINT('Ctrl Pts',(17.8937235916942,4.98327371000135,10.4964545565713));
#38681=CARTESIAN_POINT('Ctrl Pts',(17.9454531485941,5.00471582482622,10.4992316551565));
#38682=CARTESIAN_POINT('Ctrl Pts',(17.9735948214907,5.01,10.5));
#38683=CARTESIAN_POINT('Ctrl Pts',(18.0264051785093,5.01,10.5));
#38684=CARTESIAN_POINT('Ctrl Pts',(18.0545468514059,5.00471582482622,10.4992316551565));
#38685=CARTESIAN_POINT('Ctrl Pts',(18.1062764083058,4.98327371000135,10.4964545565713));
#38686=CARTESIAN_POINT('Ctrl Pts',(18.1298671698874,4.96711767821098,10.4944848114133));
#38687=CARTESIAN_POINT('Ctrl Pts',(18.1671179239704,4.92986692412796,10.4907789715758));
#38688=CARTESIAN_POINT('Ctrl Pts',(18.1832737630363,4.90627626890513,10.4888007328232));
#38689=CARTESIAN_POINT('Ctrl Pts',(18.2047157372696,4.85454707409071,10.4860041595441));
#38690=CARTESIAN_POINT('Ctrl Pts',(18.21,4.82640552692445,10.4852272553384));
#38691=CARTESIAN_POINT('Ctrl Pts',(18.21,4.8,10.4852272553384));
#38692=CARTESIAN_POINT('',(17.8589326402034,4.95556349186105,9.99));
#38693=CARTESIAN_POINT('Origin',(18.,4.8,9.99));
#38694=CARTESIAN_POINT('Ctrl Pts',(18.1410673597966,4.95556349186106,9.99));
#38695=CARTESIAN_POINT('Ctrl Pts',(18.1238183566982,4.97120515236321,9.99245784982447));
#38696=CARTESIAN_POINT('Ctrl Pts',(18.1029986431097,4.98462404333102,9.99493819304946));
#38697=CARTESIAN_POINT('Ctrl Pts',(18.0546141143984,5.00469746372443,9.99884449237241));
#38698=CARTESIAN_POINT('Ctrl Pts',(18.0264520736824,5.01,10.));
#38699=CARTESIAN_POINT('Ctrl Pts',(17.9735479263176,5.01,10.));
#38700=CARTESIAN_POINT('Ctrl Pts',(17.9453858856016,5.00469746372443,9.99884449237241));
#38701=CARTESIAN_POINT('Ctrl Pts',(17.8970013568903,4.98462404333102,9.99493819304946));
#38702=CARTESIAN_POINT('Ctrl Pts',(17.8761816433018,4.97120515236321,9.99245784982447));
#38703=CARTESIAN_POINT('Ctrl Pts',(17.8589326402034,4.95556349186105,9.99));
#38704=CARTESIAN_POINT('Origin',(18.,4.8,9.99));
#38705=CARTESIAN_POINT('',(17.8589326402034,4.2,9.99));
#38706=CARTESIAN_POINT('Origin',(18.,4.4,9.1));
#38707=CARTESIAN_POINT('',(19.4906215647723,4.4,9.16747343262672));
#38708=CARTESIAN_POINT('',(19.4906215647723,4.6,9.16747343262672));
#38709=CARTESIAN_POINT('',(19.4906215647723,4.2,9.16747343262672));
#38710=CARTESIAN_POINT('',(20.9907520011994,4.4,9.23537728718354));
#38711=CARTESIAN_POINT('',(18.,4.4,9.1));
#38712=CARTESIAN_POINT('',(20.9907520011994,4.6,9.23537728718354));
#38713=CARTESIAN_POINT('',(20.9907520011994,4.4,9.23537728718354));
#38714=CARTESIAN_POINT('',(18.,4.6,9.1));
#38715=CARTESIAN_POINT('Origin',(19.4953760005997,4.4,9.06768864359177));
#38716=CARTESIAN_POINT('',(19.4984563276619,4.4,9.06803406565731));
#38717=CARTESIAN_POINT('Origin',(18.,4.4,9.));
#38718=CARTESIAN_POINT('',(20.9907520011994,4.4,9.23537728718354));
#38719=CARTESIAN_POINT('Origin',(19.4953760005997,4.6,9.06768864359177));
#38720=CARTESIAN_POINT('',(19.4984563276619,4.6,9.06803406565731));
#38721=CARTESIAN_POINT('Origin',(18.,4.6,9.));
#38722=CARTESIAN_POINT('',(20.9907520011994,4.6,9.23537728718354));
#38723=CARTESIAN_POINT('Origin',(20.9907520011994,4.4,9.23537728718354));
#38724=CARTESIAN_POINT('',(19.4984563276619,4.2,9.06803406565731));
#38725=CARTESIAN_POINT('Origin',(18.,4.2,9.));
#38726=CARTESIAN_POINT('',(17.,5.5,9.));
#38727=CARTESIAN_POINT('Origin',(18.,5.5,9.));
#38728=CARTESIAN_POINT('',(17.,4.2,9.));
#38729=CARTESIAN_POINT('',(17.,4.2,9.));
#38730=CARTESIAN_POINT('Origin',(18.,4.2,9.));
#38731=CARTESIAN_POINT('Origin',(18.,4.2,9.));
#38732=CARTESIAN_POINT('',(16.5,5.5,9.));
#38733=CARTESIAN_POINT('Origin',(18.,5.5,9.));
#38734=CARTESIAN_POINT('',(16.5,4.2,9.));
#38735=CARTESIAN_POINT('',(16.5,4.2,9.));
#38736=CARTESIAN_POINT('Origin',(18.,4.2,9.));
#38737=CARTESIAN_POINT('Origin',(18.,5.5,9.));
#38738=CARTESIAN_POINT('Origin',(18.,4.2,9.));
#38739=CARTESIAN_POINT('',(0.,0.,0.));
#38740=CARTESIAN_POINT('Origin',(18.,6.,9.));
#38741=CARTESIAN_POINT('',(17.775,6.2,9.));
#38742=CARTESIAN_POINT('Origin',(18.,6.2,9.));
#38743=CARTESIAN_POINT('',(17.775,6.,9.));
#38744=CARTESIAN_POINT('',(17.775,6.,9.));
#38745=CARTESIAN_POINT('Origin',(18.,6.,9.));
#38746=CARTESIAN_POINT('Origin',(18.,6.,9.));
#38747=CARTESIAN_POINT('',(16.6,6.2,9.));
#38748=CARTESIAN_POINT('Origin',(18.,6.2,9.));
#38749=CARTESIAN_POINT('',(16.6,6.,9.));
#38750=CARTESIAN_POINT('',(16.6,6.,9.));
#38751=CARTESIAN_POINT('Origin',(18.,6.,9.));
#38752=CARTESIAN_POINT('Origin',(18.,6.2,9.));
#38753=CARTESIAN_POINT('Origin',(18.,6.,9.));
#38754=CARTESIAN_POINT('',(0.,0.,0.));
#38755=CARTESIAN_POINT('Origin',(0.3,0.,0.));
#38756=CARTESIAN_POINT('',(0.3,2.2,-1.28));
#38757=CARTESIAN_POINT('',(0.3,2.2,-0.953939201416946));
#38758=CARTESIAN_POINT('',(0.3,2.2,0.));
#38759=CARTESIAN_POINT('',(0.3,-1.,-1.28));
#38760=CARTESIAN_POINT('',(0.3,0.,-1.28));
#38761=CARTESIAN_POINT('',(0.3,-1.,-0.953939201416946));
#38762=CARTESIAN_POINT('',(0.3,-1.,0.));
#38763=CARTESIAN_POINT('',(0.3,0.,-0.953939201416946));
#38764=CARTESIAN_POINT('Origin',(0.3,0.,-1.28));
#38765=CARTESIAN_POINT('',(-0.3,2.2,-1.28));
#38766=CARTESIAN_POINT('',(0.15,2.2,-1.28));
#38767=CARTESIAN_POINT('',(-0.3,-1.,-1.28));
#38768=CARTESIAN_POINT('',(-0.3,0.,-1.28));
#38769=CARTESIAN_POINT('',(0.15,-1.,-1.28));
#38770=CARTESIAN_POINT('Origin',(-0.3,0.,-1.28));
#38771=CARTESIAN_POINT('',(-0.3,2.2,-0.953939201416946));
#38772=CARTESIAN_POINT('',(-0.3,2.2,-0.64));
#38773=CARTESIAN_POINT('',(-0.3,-1.,-0.953939201416946));
#38774=CARTESIAN_POINT('',(-0.3,0.,-0.953939201416946));
#38775=CARTESIAN_POINT('',(-0.3,-1.,-0.64));
#38776=CARTESIAN_POINT('Origin',(0.,-1.,0.));
#38777=CARTESIAN_POINT('',(3.66661143271685,-1.,0.786422660831985));
#38778=CARTESIAN_POINT('',(3.62400312501245,-1.,0.963899035117249));
#38779=CARTESIAN_POINT('Origin',(0.,-1.,0.));
#38780=CARTESIAN_POINT('',(4.01728681790024,-1.,1.22531898815164));
#38781=CARTESIAN_POINT('Ctrl Pts',(3.62400312501245,-1.,0.963899035117249));
#38782=CARTESIAN_POINT('Ctrl Pts',(3.6240482887845,-1.,0.963880158555582));
#38783=CARTESIAN_POINT('Ctrl Pts',(3.62424461507588,-1.,0.963861297423241));
#38784=CARTESIAN_POINT('Ctrl Pts',(3.62489305727662,-1.,0.963957782642844));
#38785=CARTESIAN_POINT('Ctrl Pts',(3.62652618145335,-1.,0.964373850166458));
#38786=CARTESIAN_POINT('Ctrl Pts',(3.62988252139846,-1.,0.965395153165294));
#38787=CARTESIAN_POINT('Ctrl Pts',(3.63492122081143,-1.,0.967052554541386));
#38788=CARTESIAN_POINT('Ctrl Pts',(3.64113946505766,-1.,0.969195124675866));
#38789=CARTESIAN_POINT('Ctrl Pts',(3.64819756447455,-1.,0.971722122061341));
#38790=CARTESIAN_POINT('Ctrl Pts',(3.65571576735126,-1.,0.974519971354849));
#38791=CARTESIAN_POINT('Ctrl Pts',(3.66333049637475,-1.,0.977478312751618));
#38792=CARTESIAN_POINT('Ctrl Pts',(3.67074983340361,-1.,0.980505922458267));
#38793=CARTESIAN_POINT('Ctrl Pts',(3.67782408841715,-1.,0.98355079147042));
#38794=CARTESIAN_POINT('Ctrl Pts',(3.68455317926068,-1.,0.986602639863838));
#38795=CARTESIAN_POINT('Ctrl Pts',(3.69102682138846,-1.,0.989676715398559));
#38796=CARTESIAN_POINT('Ctrl Pts',(3.69738123415662,-1.,0.992802218332011));
#38797=CARTESIAN_POINT('Ctrl Pts',(3.70375282282138,-1.,0.996009819772518));
#38798=CARTESIAN_POINT('Ctrl Pts',(3.71022439713938,-1.,0.999317260756531));
#38799=CARTESIAN_POINT('Ctrl Pts',(3.71680667125118,-1.,1.00272423396822));
#38800=CARTESIAN_POINT('Ctrl Pts',(3.72346803750595,-1.,1.0062200073571));
#38801=CARTESIAN_POINT('Ctrl Pts',(3.73015276704426,-1.,1.00978798539496));
#38802=CARTESIAN_POINT('Ctrl Pts',(3.73680245055734,-1.,1.01341114319903));
#38803=CARTESIAN_POINT('Ctrl Pts',(3.74337942504959,-1.,1.01707794311079));
#38804=CARTESIAN_POINT('Ctrl Pts',(3.74987777155834,-1.,1.02078510487428));
#38805=CARTESIAN_POINT('Ctrl Pts',(3.75631037456194,-1.,1.0245342944466));
#38806=CARTESIAN_POINT('Ctrl Pts',(3.76270122291232,-1.,1.02833014458181));
#38807=CARTESIAN_POINT('Ctrl Pts',(3.76907609832522,-1.,1.0321778660492));
#38808=CARTESIAN_POINT('Ctrl Pts',(3.77545283140445,-1.,1.03608074678013));
#38809=CARTESIAN_POINT('Ctrl Pts',(3.78183535008192,-1.,1.04003862055804));
#38810=CARTESIAN_POINT('Ctrl Pts',(3.78821910787195,-1.,1.04404924374426));
#38811=CARTESIAN_POINT('Ctrl Pts',(3.79459440308793,-1.,1.04810913267641));
#38812=CARTESIAN_POINT('Ctrl Pts',(3.80095039790678,-1.,1.05221457990015));
#38813=CARTESIAN_POINT('Ctrl Pts',(3.80727913637784,-1.,1.05636266918643));
#38814=CARTESIAN_POINT('Ctrl Pts',(3.81357866117485,-1.,1.06055206187298));
#38815=CARTESIAN_POINT('Ctrl Pts',(3.81985083953012,-1.,1.06478244038931));
#38816=CARTESIAN_POINT('Ctrl Pts',(3.82609989967278,-1.,1.0690541318036));
#38817=CARTESIAN_POINT('Ctrl Pts',(3.83233071195145,-1.,1.0733676663346));
#38818=CARTESIAN_POINT('Ctrl Pts',(3.83854714117486,-1.,1.07772335353856));
#38819=CARTESIAN_POINT('Ctrl Pts',(3.84475048030615,-1.,1.08212087917986));
#38820=CARTESIAN_POINT('Ctrl Pts',(3.8509402522269,-1.,1.08655950846377));
#38821=CARTESIAN_POINT('Ctrl Pts',(3.85711487933911,-1.,1.09103825516288));
#38822=CARTESIAN_POINT('Ctrl Pts',(3.86327241021242,-1.,1.09555606505012));
#38823=CARTESIAN_POINT('Ctrl Pts',(3.86941120134872,-1.,1.10011198761203));
#38824=CARTESIAN_POINT('Ctrl Pts',(3.87553067187566,-1.,1.10470536603303));
#38825=CARTESIAN_POINT('Ctrl Pts',(3.88163105531791,-1.,1.10933577224029));
#38826=CARTESIAN_POINT('Ctrl Pts',(3.88771308285229,-1.,1.11400292434447));
#38827=CARTESIAN_POINT('Ctrl Pts',(3.89377768340362,-1.,1.11870660794609));
#38828=CARTESIAN_POINT('Ctrl Pts',(3.89982569749978,-1.,1.12344660099029));
#38829=CARTESIAN_POINT('Ctrl Pts',(3.90585753318622,-1.,1.12822258281518));
#38830=CARTESIAN_POINT('Ctrl Pts',(3.91187321145495,-1.,1.13303414693849));
#38831=CARTESIAN_POINT('Ctrl Pts',(3.91787251936688,-1.,1.13788084225511));
#38832=CARTESIAN_POINT('Ctrl Pts',(3.92385513133937,-1.,1.14276220561575));
#38833=CARTESIAN_POINT('Ctrl Pts',(3.92982073294334,-1.,1.14767779451147));
#38834=CARTESIAN_POINT('Ctrl Pts',(3.9357691705651,-1.,1.15262722716391));
#38835=CARTESIAN_POINT('Ctrl Pts',(3.94170046685542,-1.,1.15761018341061));
#38836=CARTESIAN_POINT('Ctrl Pts',(3.9476147478092,-1.,1.16262637999261));
#38837=CARTESIAN_POINT('Ctrl Pts',(3.95351219510062,-1.,1.16767555244495));
#38838=CARTESIAN_POINT('Ctrl Pts',(3.95939299213164,-1.,1.17275743590327));
#38839=CARTESIAN_POINT('Ctrl Pts',(3.96525726357682,-1.,1.17787174135446));
#38840=CARTESIAN_POINT('Ctrl Pts',(3.9711050516465,-1.,1.18301815039596));
#38841=CARTESIAN_POINT('Ctrl Pts',(3.97693634766926,-1.,1.18819633715285));
#38842=CARTESIAN_POINT('Ctrl Pts',(3.98275111052015,-1.,1.19340598349307));
#38843=CARTESIAN_POINT('Ctrl Pts',(3.98854928957287,-1.,1.19864679609596));
#38844=CARTESIAN_POINT('Ctrl Pts',(3.99433084800649,-1.,1.2039185237544));
#38845=CARTESIAN_POINT('Ctrl Pts',(4.00009577952534,-1.,1.20922097030107));
#38846=CARTESIAN_POINT('Ctrl Pts',(4.00584409524937,-1.,1.21455398918813));
#38847=CARTESIAN_POINT('Ctrl Pts',(4.01042947142681,-1.,1.21884478244983));
#38848=CARTESIAN_POINT('Ctrl Pts',(4.01386104434674,-1.,1.22207656456199));
#38849=CARTESIAN_POINT('Ctrl Pts',(4.0161454457032,-1.,1.22423716681447));
#38850=CARTESIAN_POINT('Ctrl Pts',(4.01728681790024,-1.,1.22531898815164));
#38851=CARTESIAN_POINT('',(3.97027773754922,-1.,1.36999806084573));
#38852=CARTESIAN_POINT('',(4.01728681790024,-1.,1.22531898815164));
#38853=CARTESIAN_POINT('',(3.4984457533445,-1.,1.35032489087101));
#38854=CARTESIAN_POINT('Ctrl Pts',(3.97027773754922,-1.,1.36999806084573));
#38855=CARTESIAN_POINT('Ctrl Pts',(3.9687184694131,-1.,1.37020239094614));
#38856=CARTESIAN_POINT('Ctrl Pts',(3.96560037974645,-1.,1.37060761745635));
#38857=CARTESIAN_POINT('Ctrl Pts',(3.96092458506535,-1.,1.3712051561502));
#38858=CARTESIAN_POINT('Ctrl Pts',(3.95469287280914,-1.,1.37198126432386));
#38859=CARTESIAN_POINT('Ctrl Pts',(3.94690771785133,-1.,1.37291699202807));
#38860=CARTESIAN_POINT('Ctrl Pts',(3.93912709040818,-1.,1.37381821967165));
#38861=CARTESIAN_POINT('Ctrl Pts',(3.93135106761844,-1.,1.37468482215751));
#38862=CARTESIAN_POINT('Ctrl Pts',(3.92357976987672,-1.,1.37551664448242));
#38863=CARTESIAN_POINT('Ctrl Pts',(3.91581337462644,-1.,1.37631350505797));
#38864=CARTESIAN_POINT('Ctrl Pts',(3.90805209523486,-1.,1.3770751963402));
#38865=CARTESIAN_POINT('Ctrl Pts',(3.90029615196727,-1.,1.37780148512792));
#38866=CARTESIAN_POINT('Ctrl Pts',(3.89254574338496,-1.,1.3784921128802));
#38867=CARTESIAN_POINT('Ctrl Pts',(3.88480102249277,-1.,1.37914679719383));
#38868=CARTESIAN_POINT('Ctrl Pts',(3.87706205830532,-1.,1.37976523097073));
#38869=CARTESIAN_POINT('Ctrl Pts',(3.86932885813068,-1.,1.38034709213014));
#38870=CARTESIAN_POINT('Ctrl Pts',(3.86160143043959,-1.,1.3808920599299));
#38871=CARTESIAN_POINT('Ctrl Pts',(3.85387983979481,-1.,1.3813998311505));
#38872=CARTESIAN_POINT('Ctrl Pts',(3.84616425605764,-1.,1.38187013346109));
#38873=CARTESIAN_POINT('Ctrl Pts',(3.83845502790746,-1.,1.38230274828822));
#38874=CARTESIAN_POINT('Ctrl Pts',(3.8307526698229,-1.,1.38269750245138));
#38875=CARTESIAN_POINT('Ctrl Pts',(3.82305771743829,-1.,1.38305421262763));
#38876=CARTESIAN_POINT('Ctrl Pts',(3.81537060817811,-1.,1.38337263902782));
#38877=CARTESIAN_POINT('Ctrl Pts',(3.80769156398411,-1.,1.3836524404622));
#38878=CARTESIAN_POINT('Ctrl Pts',(3.80002044322111,-1.,1.38389311766682));
#38879=CARTESIAN_POINT('Ctrl Pts',(3.79235669640841,-1.,1.38409399694566));
#38880=CARTESIAN_POINT('Ctrl Pts',(3.78469969805082,-1.,1.38425435883756));
#38881=CARTESIAN_POINT('Ctrl Pts',(3.77704902230418,-1.,1.38437354551428));
#38882=CARTESIAN_POINT('Ctrl Pts',(3.76940473185779,-1.,1.38445107339518));
#38883=CARTESIAN_POINT('Ctrl Pts',(3.76176768271367,-1.,1.3844867525335));
#38884=CARTESIAN_POINT('Ctrl Pts',(3.7541397631875,-1.,1.38448077997163));
#38885=CARTESIAN_POINT('Ctrl Pts',(3.74652317167876,-1.,1.38443344984394));
#38886=CARTESIAN_POINT('Ctrl Pts',(3.73891976418104,-1.,1.38434489156458));
#38887=CARTESIAN_POINT('Ctrl Pts',(3.73133035859282,-1.,1.38421479111531));
#38888=CARTESIAN_POINT('Ctrl Pts',(3.72375409358803,-1.,1.3840421342895));
#38889=CARTESIAN_POINT('Ctrl Pts',(3.7161876605181,-1.,1.38382489984586));
#38890=CARTESIAN_POINT('Ctrl Pts',(3.70862680753347,-1.,1.38356065402124));
#38891=CARTESIAN_POINT('Ctrl Pts',(3.701067921679,-1.,1.38324717612865));
#38892=CARTESIAN_POINT('Ctrl Pts',(3.69350967899526,-1.,1.38288311171651));
#38893=CARTESIAN_POINT('Ctrl Pts',(3.68595444983837,-1.,1.38246852827182));
#38894=CARTESIAN_POINT('Ctrl Pts',(3.67841038482414,-1.,1.3820057429062));
#38895=CARTESIAN_POINT('Ctrl Pts',(3.67088843112262,-1.,1.38149812653868));
#38896=CARTESIAN_POINT('Ctrl Pts',(3.66339848520857,-1.,1.38094856333552));
#38897=CARTESIAN_POINT('Ctrl Pts',(3.6559455440439,-1.,1.38035791051213));
#38898=CARTESIAN_POINT('Ctrl Pts',(3.64852652756456,-1.,1.37972372481603));
#38899=CARTESIAN_POINT('Ctrl Pts',(3.64112507791141,-1.,1.37903818567359));
#38900=CARTESIAN_POINT('Ctrl Pts',(3.63371727442486,-1.,1.37829035457339));
#38901=CARTESIAN_POINT('Ctrl Pts',(3.62628098665145,-1.,1.37746987919881));
#38902=CARTESIAN_POINT('Ctrl Pts',(3.6188048116042,-1.,1.37657053403107));
#38903=CARTESIAN_POINT('Ctrl Pts',(3.61129546591064,-1.,1.37559314436634));
#38904=CARTESIAN_POINT('Ctrl Pts',(3.60379020123988,-1.,1.37455051379623));
#38905=CARTESIAN_POINT('Ctrl Pts',(3.59634627869048,-1.,1.37346320103157));
#38906=CARTESIAN_POINT('Ctrl Pts',(3.58901853846365,-1.,1.37235053660976));
#38907=CARTESIAN_POINT('Ctrl Pts',(3.58183885982715,-1.,1.37122241663062));
#38908=CARTESIAN_POINT('Ctrl Pts',(3.57479875549486,-1.,1.37007229485659));
#38909=CARTESIAN_POINT('Ctrl Pts',(3.5678208030466,-1.,1.36886584973389));
#38910=CARTESIAN_POINT('Ctrl Pts',(3.56077662028649,-1.,1.36754771771233));
#38911=CARTESIAN_POINT('Ctrl Pts',(3.55353883995949,-1.,1.3660614545677));
#38912=CARTESIAN_POINT('Ctrl Pts',(3.54602591832973,-1.,1.36436666257598));
#38913=CARTESIAN_POINT('Ctrl Pts',(3.53824396424961,-1.,1.36245507339307));
#38914=CARTESIAN_POINT('Ctrl Pts',(3.530344649616,-1.,1.36037259643734));
#38915=CARTESIAN_POINT('Ctrl Pts',(3.52261776116748,-1.,1.35821701528836));
#38916=CARTESIAN_POINT('Ctrl Pts',(3.51542230699556,-1.,1.35611275237152));
#38917=CARTESIAN_POINT('Ctrl Pts',(3.50913227059999,-1.,1.35419113575956));
#38918=CARTESIAN_POINT('Ctrl Pts',(3.50408168106261,-1.,1.35257032843486));
#38919=CARTESIAN_POINT('Ctrl Pts',(3.5007660381649,-1.,1.35142377279517));
#38920=CARTESIAN_POINT('Ctrl Pts',(3.49920025459723,-1.,1.35080045218587));
#38921=CARTESIAN_POINT('Ctrl Pts',(3.49861894124827,-1.,1.35049736560527));
#38922=CARTESIAN_POINT('Ctrl Pts',(3.49847119623846,-1.,1.35036670892966));
#38923=CARTESIAN_POINT('Ctrl Pts',(3.4984457533445,-1.,1.35032489087101));
#38924=CARTESIAN_POINT('',(3.42859860294378,-1.,1.51895082866166));
#38925=CARTESIAN_POINT('Origin',(0.,-1.,0.));
#38926=CARTESIAN_POINT('',(3.77614523045147,-1.,1.83867539237861));
#38927=CARTESIAN_POINT('Ctrl Pts',(3.42859860294378,-1.,1.51895082866166));
#38928=CARTESIAN_POINT('Ctrl Pts',(3.42864616361967,-1.,1.51893924967231));
#38929=CARTESIAN_POINT('Ctrl Pts',(3.42884302333978,-1.,1.51895133295017));
#38930=CARTESIAN_POINT('Ctrl Pts',(3.42946838852728,-1.,1.51914806898539));
#38931=CARTESIAN_POINT('Ctrl Pts',(3.4310163189349,-1.,1.5198144909343));
#38932=CARTESIAN_POINT('Ctrl Pts',(3.43417156977749,-1.,1.52134826724227));
#38933=CARTESIAN_POINT('Ctrl Pts',(3.43888895974182,-1.,1.52377348950429));
#38934=CARTESIAN_POINT('Ctrl Pts',(3.44469547527,-1.,1.52686242875717));
#38935=CARTESIAN_POINT('Ctrl Pts',(3.45127136828667,-1.,1.530462444618));
#38936=CARTESIAN_POINT('Ctrl Pts',(3.45825932955273,-1.,1.53440195378902));
#38937=CARTESIAN_POINT('Ctrl Pts',(3.46531752207222,-1.,1.53851507915533));
#38938=CARTESIAN_POINT('Ctrl Pts',(3.47217189224576,-1.,1.54266605398152));
#38939=CARTESIAN_POINT('Ctrl Pts',(3.47868272898599,-1.,1.54678009290207));
#38940=CARTESIAN_POINT('Ctrl Pts',(3.48485155928414,-1.,1.55084702970382));
#38941=CARTESIAN_POINT('Ctrl Pts',(3.49076460877317,-1.,1.5548959590107));
#38942=CARTESIAN_POINT('Ctrl Pts',(3.49655185179623,-1.,1.55897703097859));
#38943=CARTESIAN_POINT('Ctrl Pts',(3.50234321621607,-1.,1.56314187758689));
#38944=CARTESIAN_POINT('Ctrl Pts',(3.50821771695427,-1.,1.56742097575041));
#38945=CARTESIAN_POINT('Ctrl Pts',(3.51418598431733,-1.,1.57181569799774));
#38946=CARTESIAN_POINT('Ctrl Pts',(3.52021847865961,-1.,1.5763104998818));
#38947=CARTESIAN_POINT('Ctrl Pts',(3.52626275334899,-1.,1.58088027227856));
#38948=CARTESIAN_POINT('Ctrl Pts',(3.53226378147068,-1.,1.58549906268083));
#38949=CARTESIAN_POINT('Ctrl Pts',(3.53818616861045,-1.,1.59014958368725));
#38950=CARTESIAN_POINT('Ctrl Pts',(3.544024581823,-1.,1.5948276694975));
#38951=CARTESIAN_POINT('Ctrl Pts',(3.54979148634426,-1.,1.59953698113444));
#38952=CARTESIAN_POINT('Ctrl Pts',(3.55550985096117,-1.,1.60428584699848));
#38953=CARTESIAN_POINT('Ctrl Pts',(3.56120432482986,-1.,1.60908344685459));
#38954=CARTESIAN_POINT('Ctrl Pts',(3.56689200468404,-1.,1.61393581747522));
#38955=CARTESIAN_POINT('Ctrl Pts',(3.57257679609826,-1.,1.61884340915412));
#38956=CARTESIAN_POINT('Ctrl Pts',(3.57825455954405,-1.,1.62380329464851));
#38957=CARTESIAN_POINT('Ctrl Pts',(3.5839162577435,-1.,1.62881051550748));
#38958=CARTESIAN_POINT('Ctrl Pts',(3.58955176627876,-1.,1.63385971451259));
#38959=CARTESIAN_POINT('Ctrl Pts',(3.59515368334887,-1.,1.63894676675349));
#38960=CARTESIAN_POINT('Ctrl Pts',(3.6007202851384,-1.,1.6440700438558));
#38961=CARTESIAN_POINT('Ctrl Pts',(3.60625346556992,-1.,1.64922952425833));
#38962=CARTESIAN_POINT('Ctrl Pts',(3.61175734965129,-1.,1.65442619244327));
#38963=CARTESIAN_POINT('Ctrl Pts',(3.61723666482457,-1.,1.65966133399186));
#38964=CARTESIAN_POINT('Ctrl Pts',(3.62269517989104,-1.,1.66493585923853));
#38965=CARTESIAN_POINT('Ctrl Pts',(3.62813422105257,-1.,1.67024966008037));
#38966=CARTESIAN_POINT('Ctrl Pts',(3.63355343201211,-1.,1.67560193613145));
#38967=CARTESIAN_POINT('Ctrl Pts',(3.63895140887443,-1.,1.68099146651577));
#38968=CARTESIAN_POINT('Ctrl Pts',(3.64432638915199,-1.,1.68641690471455));
#38969=CARTESIAN_POINT('Ctrl Pts',(3.64967689827393,-1.,1.691877054817));
#38970=CARTESIAN_POINT('Ctrl Pts',(3.65500246526798,-1.,1.69737117722559));
#38971=CARTESIAN_POINT('Ctrl Pts',(3.6603033877491,-1.,1.70289888566904));
#38972=CARTESIAN_POINT('Ctrl Pts',(3.6655804319893,-1.,1.70846001610983));
#38973=CARTESIAN_POINT('Ctrl Pts',(3.67083454901629,-1.,1.71405450210392));
#38974=CARTESIAN_POINT('Ctrl Pts',(3.67606660374665,-1.,1.71968225581787));
#38975=CARTESIAN_POINT('Ctrl Pts',(3.68127704936472,-1.,1.72534302437003));
#38976=CARTESIAN_POINT('Ctrl Pts',(3.68646597019188,-1.,1.73103640956647));
#38977=CARTESIAN_POINT('Ctrl Pts',(3.69163322647906,-1.,1.73676193254493));
#38978=CARTESIAN_POINT('Ctrl Pts',(3.6967785691046,-1.,1.74251908492589));
#38979=CARTESIAN_POINT('Ctrl Pts',(3.70190175673422,-1.,1.74830738046092));
#38980=CARTESIAN_POINT('Ctrl Pts',(3.70700269736876,-1.,1.75412641804148));
#38981=CARTESIAN_POINT('Ctrl Pts',(3.71208146346454,-1.,1.75997588499021));
#38982=CARTESIAN_POINT('Ctrl Pts',(3.71713822377675,-1.,1.76585552124549));
#38983=CARTESIAN_POINT('Ctrl Pts',(3.72217319911429,-1.,1.77176509401846));
#38984=CARTESIAN_POINT('Ctrl Pts',(3.72718661205504,-1.,1.77770437039606));
#38985=CARTESIAN_POINT('Ctrl Pts',(3.73217863095022,-1.,1.78367308442682));
#38986=CARTESIAN_POINT('Ctrl Pts',(3.73714934729962,-1.,1.78967092823139));
#38987=CARTESIAN_POINT('Ctrl Pts',(3.74209880351667,-1.,1.79569757859041));
#38988=CARTESIAN_POINT('Ctrl Pts',(3.74702700874954,-1.,1.80175271485519));
#38989=CARTESIAN_POINT('Ctrl Pts',(3.75193395888069,-1.,1.80783603939662));
#38990=CARTESIAN_POINT('Ctrl Pts',(3.75681965683995,-1.,1.81394729834032));
#38991=CARTESIAN_POINT('Ctrl Pts',(3.76168412709652,-1.,1.82008629694924));
#38992=CARTESIAN_POINT('Ctrl Pts',(3.76652740355856,-1.,1.82625289221933));
#38993=CARTESIAN_POINT('Ctrl Pts',(3.77038509819777,-1.,1.83120816956515));
#38994=CARTESIAN_POINT('Ctrl Pts',(3.77326886065484,-1.,1.83493697935064));
#38995=CARTESIAN_POINT('Ctrl Pts',(3.77518714458232,-1.,1.83742834010821));
#38996=CARTESIAN_POINT('Ctrl Pts',(3.77614523045147,-1.,1.83867539237861));
#38997=CARTESIAN_POINT('',(3.70708211654725,-1.,1.97421938526992));
#38998=CARTESIAN_POINT('',(3.77614523045147,-1.,1.83867539237861));
#38999=CARTESIAN_POINT('',(3.24413672884902,-1.,1.88097764062542));
#39000=CARTESIAN_POINT('Ctrl Pts',(3.70708211654725,-1.,1.97421938526992));
#39001=CARTESIAN_POINT('Ctrl Pts',(3.7055100813194,-1.,1.974177276451));
#39002=CARTESIAN_POINT('Ctrl Pts',(3.70236698911837,-1.,1.97408973726149));
#39003=CARTESIAN_POINT('Ctrl Pts',(3.69765528558292,-1.,1.97394846382289));
#39004=CARTESIAN_POINT('Ctrl Pts',(3.69137888597855,-1.,1.97374016224397));
#39005=CARTESIAN_POINT('Ctrl Pts',(3.68354319913416,-1.,1.97344650303631));
#39006=CARTESIAN_POINT('Ctrl Pts',(3.67571738106175,-1.,1.97311947678035));
#39007=CARTESIAN_POINT('Ctrl Pts',(3.66790152751984,-1.,1.9727589719863));
#39008=CARTESIAN_POINT('Ctrl Pts',(3.66009578166865,-1.,1.97236485439317));
#39009=CARTESIAN_POINT('Ctrl Pts',(3.65230034717364,-1.,1.97193697240645));
#39010=CARTESIAN_POINT('Ctrl Pts',(3.64451546724221,-1.,1.97147515441539));
#39011=CARTESIAN_POINT('Ctrl Pts',(3.63674139590853,-1.,1.97097920454698));
#39012=CARTESIAN_POINT('Ctrl Pts',(3.62897836973397,-1.,1.97044889850518));
#39013=CARTESIAN_POINT('Ctrl Pts',(3.62122658401722,-1.,1.96988398129888));
#39014=CARTESIAN_POINT('Ctrl Pts',(3.61348615496393,-1.,1.96928416040712));
#39015=CARTESIAN_POINT('Ctrl Pts',(3.60575714017676,-1.,1.96864911885775));
#39016=CARTESIAN_POINT('Ctrl Pts',(3.59803959819725,-1.,1.96797854118257));
#39017=CARTESIAN_POINT('Ctrl Pts',(3.5903336402273,-1.,1.96727213799507));
#39018=CARTESIAN_POINT('Ctrl Pts',(3.58263947663884,-1.,1.9665296668894));
#39019=CARTESIAN_POINT('Ctrl Pts',(3.57495748601088,-1.,1.96575096652857));
#39020=CARTESIAN_POINT('Ctrl Pts',(3.56728820357933,-1.,1.96493594634643));
#39021=CARTESIAN_POINT('Ctrl Pts',(3.55963218706201,-1.,1.96408450906868));
#39022=CARTESIAN_POINT('Ctrl Pts',(3.55198990600929,-1.,1.96319648628667));
#39023=CARTESIAN_POINT('Ctrl Pts',(3.54436163300425,-1.,1.96227157573058));
#39024=CARTESIAN_POINT('Ctrl Pts',(3.53674730625759,-1.,1.96130926212661));
#39025=CARTESIAN_POINT('Ctrl Pts',(3.52914648844289,-1.,1.96030879411534));
#39026=CARTESIAN_POINT('Ctrl Pts',(3.52155867431438,-1.,1.95926936324436));
#39027=CARTESIAN_POINT('Ctrl Pts',(3.51398354617772,-1.,1.95819025316768));
#39028=CARTESIAN_POINT('Ctrl Pts',(3.50642124159913,-1.,1.95707099606514));
#39029=CARTESIAN_POINT('Ctrl Pts',(3.49887263575602,-1.,1.9559115382367));
#39030=CARTESIAN_POINT('Ctrl Pts',(3.49133956289154,-1.,1.95471236969653));
#39031=CARTESIAN_POINT('Ctrl Pts',(3.48382414832648,-1.,1.95347412486316));
#39032=CARTESIAN_POINT('Ctrl Pts',(3.47632820495926,-1.,1.95219722189878));
#39033=CARTESIAN_POINT('Ctrl Pts',(3.4688525897419,-1.,1.95088147859876));
#39034=CARTESIAN_POINT('Ctrl Pts',(3.46139661060959,-1.,1.94952575850196));
#39035=CARTESIAN_POINT('Ctrl Pts',(3.45395731584051,-1.,1.94812754766524));
#39036=CARTESIAN_POINT('Ctrl Pts',(3.44653088665685,-1.,1.94668377715332));
#39037=CARTESIAN_POINT('Ctrl Pts',(3.43911410197693,-1.,1.94519168842883));
#39038=CARTESIAN_POINT('Ctrl Pts',(3.43170586602436,-1.,1.94364973660285));
#39039=CARTESIAN_POINT('Ctrl Pts',(3.42430850941497,-1.,1.94205835913692));
#39040=CARTESIAN_POINT('Ctrl Pts',(3.41692971994082,-1.,1.94042111965237));
#39041=CARTESIAN_POINT('Ctrl Pts',(3.40957978266622,-1.,1.93874306008132));
#39042=CARTESIAN_POINT('Ctrl Pts',(3.40226802104093,-1.,1.93702857723089));
#39043=CARTESIAN_POINT('Ctrl Pts',(3.39499923640789,-1.,1.93527929945982));
#39044=CARTESIAN_POINT('Ctrl Pts',(3.38777076883267,-1.,1.93349233176794));
#39045=CARTESIAN_POINT('Ctrl Pts',(3.38056768525577,-1.,1.93165739093292));
#39046=CARTESIAN_POINT('Ctrl Pts',(3.37336807068078,-1.,1.92975993109897));
#39047=CARTESIAN_POINT('Ctrl Pts',(3.36615168657597,-1.,1.92778626543803));
#39048=CARTESIAN_POINT('Ctrl Pts',(3.35890824422976,-1.,1.92572846125763));
#39049=CARTESIAN_POINT('Ctrl Pts',(3.35164424847206,-1.,1.92358838440518));
#39050=CARTESIAN_POINT('Ctrl Pts',(3.34439448941915,-1.,1.92138450828378));
#39051=CARTESIAN_POINT('Ctrl Pts',(3.33721230709948,-1.,1.91914609610173));
#39052=CARTESIAN_POINT('Ctrl Pts',(3.33014884257812,-1.,1.91690081930297));
#39053=CARTESIAN_POINT('Ctrl Pts',(3.32323403454507,-1.,1.91466343916612));
#39054=CARTESIAN_POINT('Ctrl Pts',(3.31646052426395,-1.,1.91242616234459));
#39055=CARTESIAN_POINT('Ctrl Pts',(3.30975721158694,-1.,1.91014297830502));
#39056=CARTESIAN_POINT('Ctrl Pts',(3.30300595568341,-1.,1.90773912171424));
#39057=CARTESIAN_POINT('Ctrl Pts',(3.29608978722258,-1.,1.9051389186417));
#39058=CARTESIAN_POINT('Ctrl Pts',(3.28893448600364,-1.,1.9022897124757));
#39059=CARTESIAN_POINT('Ctrl Pts',(3.28154737912287,-1.,1.89918429230425));
#39060=CARTESIAN_POINT('Ctrl Pts',(3.27407108932908,-1.,1.89589172903662));
#39061=CARTESIAN_POINT('Ctrl Pts',(3.2667765388833,-1.,1.89255393500769));
#39062=CARTESIAN_POINT('Ctrl Pts',(3.2599988519361,-1.,1.88934996203508));
#39063=CARTESIAN_POINT('Ctrl Pts',(3.25408686339298,-1.,1.88646802523372));
#39064=CARTESIAN_POINT('Ctrl Pts',(3.24935200512055,-1.,1.88407708646435));
#39065=CARTESIAN_POINT('Ctrl Pts',(3.24625654410705,-1.,1.88242596600422));
#39066=CARTESIAN_POINT('Ctrl Pts',(3.24480754675942,-1.,1.88156537699118));
#39067=CARTESIAN_POINT('Ctrl Pts',(3.24428080352952,-1.,1.88117508446657));
#39068=CARTESIAN_POINT('Ctrl Pts',(3.2441553167131,-1.,1.88102292397987));
#39069=CARTESIAN_POINT('Ctrl Pts',(3.24413672884902,-1.,1.88097764062542));
#39070=CARTESIAN_POINT('',(3.14877060440425,-1.,2.03660101169564));
#39071=CARTESIAN_POINT('Origin',(0.,-1.,0.));
#39072=CARTESIAN_POINT('',(3.44202241512147,-1.,2.40675750623143));
#39073=CARTESIAN_POINT('Ctrl Pts',(3.14877060440425,-1.,2.03660101169564));
#39074=CARTESIAN_POINT('Ctrl Pts',(3.1488193908823,-1.,2.03659701539175));
#39075=CARTESIAN_POINT('Ctrl Pts',(3.14901193669147,-1.,2.03663974554941));
#39076=CARTESIAN_POINT('Ctrl Pts',(3.14959882629936,-1.,2.03693188810614));
#39077=CARTESIAN_POINT('Ctrl Pts',(3.15102344775396,-1.,2.03783225496023));
#39078=CARTESIAN_POINT('Ctrl Pts',(3.1538999167466,-1.,2.03984073791432));
#39079=CARTESIAN_POINT('Ctrl Pts',(3.15817983946525,-1.,2.04297406404132));
#39080=CARTESIAN_POINT('Ctrl Pts',(3.16343165059235,-1.,2.0469333124766));
#39081=CARTESIAN_POINT('Ctrl Pts',(3.16936341689859,-1.,2.05151770247452));
#39082=CARTESIAN_POINT('Ctrl Pts',(3.17564906975592,-1.,2.05650186773279));
#39083=CARTESIAN_POINT('Ctrl Pts',(3.18197692964677,-1.,2.06166849827143));
#39084=CARTESIAN_POINT('Ctrl Pts',(3.18809755562297,-1.,2.06684062744065));
#39085=CARTESIAN_POINT('Ctrl Pts',(3.19388465568113,-1.,2.07192253497765));
#39086=CARTESIAN_POINT('Ctrl Pts',(3.19934132835879,-1.,2.0769044187063));
#39087=CARTESIAN_POINT('Ctrl Pts',(3.20454818630635,-1.,2.08182850370816));
#39088=CARTESIAN_POINT('Ctrl Pts',(3.20962575845433,-1.,2.08676465517435));
#39089=CARTESIAN_POINT('Ctrl Pts',(3.2146942960168,-1.,2.0917841946046));
#39090=CARTESIAN_POINT('Ctrl Pts',(3.21982707347067,-1.,2.09692958434933));
#39091=CARTESIAN_POINT('Ctrl Pts',(3.22503437553496,-1.,2.10220384298534));
#39092=CARTESIAN_POINT('Ctrl Pts',(3.23028945793334,-1.,2.1075869964248));
#39093=CARTESIAN_POINT('Ctrl Pts',(3.23554444767115,-1.,2.11304604021784));
#39094=CARTESIAN_POINT('Ctrl Pts',(3.24074905517282,-1.,2.11854673326972));
#39095=CARTESIAN_POINT('Ctrl Pts',(3.24587102613347,-1.,2.12406646410943));
#39096=CARTESIAN_POINT('Ctrl Pts',(3.25090574493994,-1.,2.1296002839681));
#39097=CARTESIAN_POINT('Ctrl Pts',(3.25586495065027,-1.,2.13515375878786));
#39098=CARTESIAN_POINT('Ctrl Pts',(3.26077002641868,-1.,2.14073870754258));
#39099=CARTESIAN_POINT('Ctrl Pts',(3.26564388189764,-1.,2.14636805295663));
#39100=CARTESIAN_POINT('Ctrl Pts',(3.27050245897244,-1.,2.15205043199818));
#39101=CARTESIAN_POINT('Ctrl Pts',(3.27534954469206,-1.,2.15778690038359));
#39102=CARTESIAN_POINT('Ctrl Pts',(3.28018150841414,-1.,2.16357391934434));
#39103=CARTESIAN_POINT('Ctrl Pts',(3.2849901997973,-1.,2.16940517773459));
#39104=CARTESIAN_POINT('Ctrl Pts',(3.28976645712566,-1.,2.17527380048422));
#39105=CARTESIAN_POINT('Ctrl Pts',(3.29450361500484,-1.,2.18117455557062));
#39106=CARTESIAN_POINT('Ctrl Pts',(3.29920022557635,-1.,2.18710556500325));
#39107=CARTESIAN_POINT('Ctrl Pts',(3.30385816281831,-1.,2.19306710376112));
#39108=CARTESIAN_POINT('Ctrl Pts',(3.30848134694596,-1.,2.19906078949925));
#39109=CARTESIAN_POINT('Ctrl Pts',(3.3130742460895,-1.,2.20508863150608));
#39110=CARTESIAN_POINT('Ctrl Pts',(3.31764044024231,-1.,2.21115211847872));
#39111=CARTESIAN_POINT('Ctrl Pts',(3.32218125618955,-1.,2.21725135110889));
#39112=CARTESIAN_POINT('Ctrl Pts',(3.32669646722871,-1.,2.22338548312759));
#39113=CARTESIAN_POINT('Ctrl Pts',(3.33118487773593,-1.,2.22955308907221));
#39114=CARTESIAN_POINT('Ctrl Pts',(3.33564495756478,-1.,2.2357525632881));
#39115=CARTESIAN_POINT('Ctrl Pts',(3.34007543738044,-1.,2.24198249391437));
#39116=CARTESIAN_POINT('Ctrl Pts',(3.34447596770768,-1.,2.24824207678288));
#39117=CARTESIAN_POINT('Ctrl Pts',(3.34884690292342,-1.,2.25453097693524));
#39118=CARTESIAN_POINT('Ctrl Pts',(3.35318902552676,-1.,2.26084915222484));
#39119=CARTESIAN_POINT('Ctrl Pts',(3.35750328523077,-1.,2.26719668579921));
#39120=CARTESIAN_POINT('Ctrl Pts',(3.36179055004369,-1.,2.27357362620902));
#39121=CARTESIAN_POINT('Ctrl Pts',(3.36605130712978,-1.,2.27997979457968));
#39122=CARTESIAN_POINT('Ctrl Pts',(3.37028570206357,-1.,2.28641481081045));
#39123=CARTESIAN_POINT('Ctrl Pts',(3.37449367172707,-1.,2.2928781800731));
#39124=CARTESIAN_POINT('Ctrl Pts',(3.37867504959382,-1.,2.29936936127588));
#39125=CARTESIAN_POINT('Ctrl Pts',(3.38282967336676,-1.,2.30588783640389));
#39126=CARTESIAN_POINT('Ctrl Pts',(3.38695751492659,-1.,2.31243319489505));
#39127=CARTESIAN_POINT('Ctrl Pts',(3.39105869475112,-1.,2.31900513925627));
#39128=CARTESIAN_POINT('Ctrl Pts',(3.39513342020045,-1.,2.32560343902683));
#39129=CARTESIAN_POINT('Ctrl Pts',(3.39918194578115,-1.,2.33222789882601));
#39130=CARTESIAN_POINT('Ctrl Pts',(3.40320452776646,-1.,2.33887832342715));
#39131=CARTESIAN_POINT('Ctrl Pts',(3.40720137403888,-1.,2.34555447648901));
#39132=CARTESIAN_POINT('Ctrl Pts',(3.41117262313464,-1.,2.35225606823649));
#39133=CARTESIAN_POINT('Ctrl Pts',(3.4151183675076,-1.,2.35898278606449));
#39134=CARTESIAN_POINT('Ctrl Pts',(3.41903866635384,-1.,2.36573431470314));
#39135=CARTESIAN_POINT('Ctrl Pts',(3.42293356216595,-1.,2.37251035954351));
#39136=CARTESIAN_POINT('Ctrl Pts',(3.42680309755241,-1.,2.37931067029517));
#39137=CARTESIAN_POINT('Ctrl Pts',(3.43064732714472,-1.,2.38613505844641));
#39138=CARTESIAN_POINT('Ctrl Pts',(3.43446630680436,-1.,2.39298338805823));
#39139=CARTESIAN_POINT('Ctrl Pts',(3.43750133066036,-1.,2.39848113411429));
#39140=CARTESIAN_POINT('Ctrl Pts',(3.43976627485223,-1.,2.40261515590099));
#39141=CARTESIAN_POINT('Ctrl Pts',(3.44127120683402,-1.,2.40537592959345));
#39142=CARTESIAN_POINT('Ctrl Pts',(3.44202241512147,-1.,2.40675750623143));
#39143=CARTESIAN_POINT('',(3.35260583073571,-1.,2.52982887637028));
#39144=CARTESIAN_POINT('',(3.44202241512147,-1.,2.40675750623143));
#39145=CARTESIAN_POINT('',(2.90994629141676,-1.,2.36531447826074));
#39146=CARTESIAN_POINT('Ctrl Pts',(3.35260583073571,-1.,2.52982887637028));
#39147=CARTESIAN_POINT('Ctrl Pts',(3.35105973714071,-1.,2.5295413654909));
#39148=CARTESIAN_POINT('Ctrl Pts',(3.34796903576663,-1.,2.52896321610703));
#39149=CARTESIAN_POINT('Ctrl Pts',(3.34333744115511,-1.,2.52808660915689));
#39150=CARTESIAN_POINT('Ctrl Pts',(3.33717089999103,-1.,2.52689902690158));
#39151=CARTESIAN_POINT('Ctrl Pts',(3.32947762187533,-1.,2.52538321164634));
#39152=CARTESIAN_POINT('Ctrl Pts',(3.32179931078699,-1.,2.5238359839626));
#39153=CARTESIAN_POINT('Ctrl Pts',(3.31413607874645,-1.,2.52225724871313));
#39154=CARTESIAN_POINT('Ctrl Pts',(3.30648808815442,-1.,2.52064689568511));
#39155=CARTESIAN_POINT('Ctrl Pts',(3.29885556388352,-1.,2.51900480701069));
#39156=CARTESIAN_POINT('Ctrl Pts',(3.2912387729927,-1.,2.51733085123797));
#39157=CARTESIAN_POINT('Ctrl Pts',(3.28363799702982,-1.,2.51562487464514));
#39158=CARTESIAN_POINT('Ctrl Pts',(3.27605350473142,-1.,2.513886692704));
#39159=CARTESIAN_POINT('Ctrl Pts',(3.26848552888115,-1.,2.51211608411423));
#39160=CARTESIAN_POINT('Ctrl Pts',(3.26093423001434,-1.,2.51031277813486));
#39161=CARTESIAN_POINT('Ctrl Pts',(3.25339971460982,-1.,2.50847647070723));
#39162=CARTESIAN_POINT('Ctrl Pts',(3.24588208983849,-1.,2.506606859405));
#39163=CARTESIAN_POINT('Ctrl Pts',(3.23838151080319,-1.,2.5047036758003));
#39164=CARTESIAN_POINT('Ctrl Pts',(3.23089822320646,-1.,2.50276671338111));
#39165=CARTESIAN_POINT('Ctrl Pts',(3.22343262620503,-1.,2.50079587201958));
#39166=CARTESIAN_POINT('Ctrl Pts',(3.21598526261286,-1.,2.4987911459939));
#39167=CARTESIAN_POINT('Ctrl Pts',(3.20855669849836,-1.,2.4967525264737));
#39168=CARTESIAN_POINT('Ctrl Pts',(3.20114742397588,-1.,2.49467992057755));
#39169=CARTESIAN_POINT('Ctrl Pts',(3.19375775555798,-1.,2.49257307239848));
#39170=CARTESIAN_POINT('Ctrl Pts',(3.18638771282266,-1.,2.49043146334059));
#39171=CARTESIAN_POINT('Ctrl Pts',(3.17903698136622,-1.,2.48825428288201));
#39172=CARTESIAN_POINT('Ctrl Pts',(3.17170518863313,-1.,2.48604065348587));
#39173=CARTESIAN_POINT('Ctrl Pts',(3.16439213290161,-1.,2.48378981792725));
#39174=CARTESIAN_POINT('Ctrl Pts',(3.15709802322739,-1.,2.48150133566571));
#39175=CARTESIAN_POINT('Ctrl Pts',(3.14982373241352,-1.,2.47917529057029));
#39176=CARTESIAN_POINT('Ctrl Pts',(3.1425709954655,-1.,2.47681245356109));
#39177=CARTESIAN_POINT('Ctrl Pts',(3.13534181229295,-1.,2.47441378371932));
#39178=CARTESIAN_POINT('Ctrl Pts',(3.12813790805952,-1.,2.47197997765871));
#39179=CARTESIAN_POINT('Ctrl Pts',(3.12096015766983,-1.,2.46951098947469));
#39180=CARTESIAN_POINT('Ctrl Pts',(3.11380805536122,-1.,2.46700558843506));
#39181=CARTESIAN_POINT('Ctrl Pts',(3.1066790790198,-1.,2.46446082979646));
#39182=CARTESIAN_POINT('Ctrl Pts',(3.09956993697052,-1.,2.46187308501884));
#39183=CARTESIAN_POINT('Ctrl Pts',(3.09247787931887,-1.,2.4592391256388));
#39184=CARTESIAN_POINT('Ctrl Pts',(3.08540206545315,-1.,2.45655725437039));
#39185=CARTESIAN_POINT('Ctrl Pts',(3.07834472886139,-1.,2.4538282678779));
#39186=CARTESIAN_POINT('Ctrl Pts',(3.07131290521297,-1.,2.45105688854422));
#39187=CARTESIAN_POINT('Ctrl Pts',(3.06431596421405,-1.,2.44824970516544));
#39188=CARTESIAN_POINT('Ctrl Pts',(3.05736242671506,-1.,2.44541251892556));
#39189=CARTESIAN_POINT('Ctrl Pts',(3.05045678021504,-1.,2.44254768923105));
#39190=CARTESIAN_POINT('Ctrl Pts',(3.04359685040555,-1.,2.43965194061857));
#39191=CARTESIAN_POINT('Ctrl Pts',(3.03676949672821,-1.,2.43671278042414));
#39192=CARTESIAN_POINT('Ctrl Pts',(3.02995534946978,-1.,2.43371241361488));
#39193=CARTESIAN_POINT('Ctrl Pts',(3.02313656036004,-1.,2.43063415586637));
#39194=CARTESIAN_POINT('Ctrl Pts',(3.01630420830504,-1.,2.42746856264168));
#39195=CARTESIAN_POINT('Ctrl Pts',(3.00946442616658,-1.,2.42421849439613));
#39196=CARTESIAN_POINT('Ctrl Pts',(3.00264868585996,-1.,2.42090763946779));
#39197=CARTESIAN_POINT('Ctrl Pts',(2.99590509293503,-1.,2.41757324500514));
#39198=CARTESIAN_POINT('Ctrl Pts',(2.98927983005796,-1.,2.41425064199586));
#39199=CARTESIAN_POINT('Ctrl Pts',(2.98280015815107,-1.,2.41095909342571));
#39200=CARTESIAN_POINT('Ctrl Pts',(2.97646002822422,-1.,2.40768975073713));
#39201=CARTESIAN_POINT('Ctrl Pts',(2.9701964131236,-1.,2.40438604734919));
#39202=CARTESIAN_POINT('Ctrl Pts',(2.96390432240312,-1.,2.4009556571164));
#39203=CARTESIAN_POINT('Ctrl Pts',(2.95748006482942,-1.,2.39730553974517));
#39204=CARTESIAN_POINT('Ctrl Pts',(2.95085857128439,-1.,2.39337207631667));
#39205=CARTESIAN_POINT('Ctrl Pts',(2.94404820669076,-1.,2.38914929090759));
#39206=CARTESIAN_POINT('Ctrl Pts',(2.93717903280391,-1.,2.38472771516311));
#39207=CARTESIAN_POINT('Ctrl Pts',(2.93049643640206,-1.,2.38028989582073));
#39208=CARTESIAN_POINT('Ctrl Pts',(2.92430340582608,-1.,2.3760651052403));
#39209=CARTESIAN_POINT('Ctrl Pts',(2.91891503791411,-1.,2.37229381109821));
#39210=CARTESIAN_POINT('Ctrl Pts',(2.9146124988314,-1.,2.36919161373173));
#39211=CARTESIAN_POINT('Ctrl Pts',(2.91181344022548,-1.,2.36707658451664));
#39212=CARTESIAN_POINT('Ctrl Pts',(2.91051690822156,-1.,2.36599991765749));
#39213=CARTESIAN_POINT('Ctrl Pts',(2.91005770527719,-1.,2.36553202948613));
#39214=CARTESIAN_POINT('Ctrl Pts',(2.90995756655606,-1.,2.36536211188453));
#39215=CARTESIAN_POINT('Ctrl Pts',(2.90994629141676,-1.,2.36531447826074));
#39216=CARTESIAN_POINT('',(2.79140942341378,-1.,2.50410331873042));
#39217=CARTESIAN_POINT('Origin',(0.,-1.,0.));
#39218=CARTESIAN_POINT('',(3.02314558451372,-1.,2.91557726271063));
#39219=CARTESIAN_POINT('Ctrl Pts',(2.79140942341378,-1.,2.50410331873043));
#39220=CARTESIAN_POINT('Ctrl Pts',(2.79145823440899,-1.,2.50410700351427));
#39221=CARTESIAN_POINT('Ctrl Pts',(2.79164172519039,-1.,2.50417932839343));
#39222=CARTESIAN_POINT('Ctrl Pts',(2.79217568804874,-1.,2.50455968395235));
#39223=CARTESIAN_POINT('Ctrl Pts',(2.79344192164204,-1.,2.50567182569153));
#39224=CARTESIAN_POINT('Ctrl Pts',(2.7959687805717,-1.,2.50810555977564));
#39225=CARTESIAN_POINT('Ctrl Pts',(2.79970585014308,-1.,2.51186983687947));
#39226=CARTESIAN_POINT('Ctrl Pts',(2.80427363984939,-1.,2.51660190466067));
#39227=CARTESIAN_POINT('Ctrl Pts',(2.80941521967234,-1.,2.52205778589922));
#39228=CARTESIAN_POINT('Ctrl Pts',(2.8148437904867,-1.,2.52796388055457));
#39229=CARTESIAN_POINT('Ctrl Pts',(2.82028550483744,-1.,2.53405679667463));
#39230=CARTESIAN_POINT('Ctrl Pts',(2.82552167649157,-1.,2.54012272520141));
#39231=CARTESIAN_POINT('Ctrl Pts',(2.83044254225794,-1.,2.54604736792542));
#39232=CARTESIAN_POINT('Ctrl Pts',(2.83505269592412,-1.,2.55182152806964));
#39233=CARTESIAN_POINT('Ctrl Pts',(2.83942515220699,-1.,2.55749952145165));
#39234=CARTESIAN_POINT('Ctrl Pts',(2.84366802680211,-1.,2.56316920798489));
#39235=CARTESIAN_POINT('Ctrl Pts',(2.84788893329091,-1.,2.56891984251743));
#39236=CARTESIAN_POINT('Ctrl Pts',(2.85215360144482,-1.,2.57480482727128));
#39237=CARTESIAN_POINT('Ctrl Pts',(2.85647171715147,-1.,2.58082875254407));
#39238=CARTESIAN_POINT('Ctrl Pts',(2.86081999003668,-1.,2.5869677064356));
#39239=CARTESIAN_POINT('Ctrl Pts',(2.86515629953528,-1.,2.59318160184921));
#39240=CARTESIAN_POINT('Ctrl Pts',(2.86943633170712,-1.,2.59942875223202));
#39241=CARTESIAN_POINT('Ctrl Pts',(2.87363176656475,-1.,2.6056817788128));
#39242=CARTESIAN_POINT('Ctrl Pts',(2.87773881947885,-1.,2.61193507170928));
#39243=CARTESIAN_POINT('Ctrl Pts',(2.88176821427502,-1.,2.61819596473087));
#39244=CARTESIAN_POINT('Ctrl Pts',(2.88573922195049,-1.,2.62447947640253));
#39245=CARTESIAN_POINT('Ctrl Pts',(2.88967244854243,-1.,2.63080195420771));
#39246=CARTESIAN_POINT('Ctrl Pts',(2.89358228854557,-1.,2.63717442263944));
#39247=CARTESIAN_POINT('Ctrl Pts',(2.89747231723361,-1.,2.64359851684146));
#39248=CARTESIAN_POINT('Ctrl Pts',(2.90133950224879,-1.,2.65007017365576));
#39249=CARTESIAN_POINT('Ctrl Pts',(2.90517678087467,-1.,2.65658188464287));
#39250=CARTESIAN_POINT('Ctrl Pts',(2.90897617968921,-1.,2.66312542616809));
#39251=CARTESIAN_POINT('Ctrl Pts',(2.91273193382876,-1.,2.66969458792627));
#39252=CARTESIAN_POINT('Ctrl Pts',(2.91644290704281,-1.,2.67628728855309));
#39253=CARTESIAN_POINT('Ctrl Pts',(2.92011090722152,-1.,2.68290409279689));
#39254=CARTESIAN_POINT('Ctrl Pts',(2.92373955325876,-1.,2.68954721165342));
#39255=CARTESIAN_POINT('Ctrl Pts',(2.92733294395268,-1.,2.69621932864302));
#39256=CARTESIAN_POINT('Ctrl Pts',(2.93089438233746,-1.,2.70292247416881));
#39257=CARTESIAN_POINT('Ctrl Pts',(2.93442516311167,-1.,2.70965695523776));
#39258=CARTESIAN_POINT('Ctrl Pts',(2.93792519474955,-1.,2.71642190053575));
#39259=CARTESIAN_POINT('Ctrl Pts',(2.94139351933882,-1.,2.72321571511322));
#39260=CARTESIAN_POINT('Ctrl Pts',(2.94482887675139,-1.,2.73003657371613));
#39261=CARTESIAN_POINT('Ctrl Pts',(2.94823023414381,-1.,2.73688288329825));
#39262=CARTESIAN_POINT('Ctrl Pts',(2.95159737214304,-1.,2.7437537949221));
#39263=CARTESIAN_POINT('Ctrl Pts',(2.95493069316211,-1.,2.75064903318996));
#39264=CARTESIAN_POINT('Ctrl Pts',(2.9582309766594,-1.,2.75756867888393));
#39265=CARTESIAN_POINT('Ctrl Pts',(2.96149914764832,-1.,2.76451296269571));
#39266=CARTESIAN_POINT('Ctrl Pts',(2.96473605585548,-1.,2.77148206836464));
#39267=CARTESIAN_POINT('Ctrl Pts',(2.9679422104295,-1.,2.77847589542767));
#39268=CARTESIAN_POINT('Ctrl Pts',(2.97111781461349,-1.,2.78549409123657));
#39269=CARTESIAN_POINT('Ctrl Pts',(2.97426288347475,-1.,2.79253615718147));
#39270=CARTESIAN_POINT('Ctrl Pts',(2.97737733718242,-1.,2.79960153278186));
#39271=CARTESIAN_POINT('Ctrl Pts',(2.98046109647299,-1.,2.80668968101162));
#39272=CARTESIAN_POINT('Ctrl Pts',(2.9835141977994,-1.,2.81380019196454));
#39273=CARTESIAN_POINT('Ctrl Pts',(2.98653680669434,-1.,2.82093279065704));
#39274=CARTESIAN_POINT('Ctrl Pts',(2.98952916401699,-1.,2.82808728190402));
#39275=CARTESIAN_POINT('Ctrl Pts',(2.99249155170479,-1.,2.83526351254383));
#39276=CARTESIAN_POINT('Ctrl Pts',(2.995424253416,-1.,2.84246132984334));
#39277=CARTESIAN_POINT('Ctrl Pts',(2.99832751144566,-1.,2.84968053289104));
#39278=CARTESIAN_POINT('Ctrl Pts',(3.0012015079552,-1.,2.85692085715129));
#39279=CARTESIAN_POINT('Ctrl Pts',(3.00404638316245,-1.,2.86418200833065));
#39280=CARTESIAN_POINT('Ctrl Pts',(3.00686224485374,-1.,2.87146368430104));
#39281=CARTESIAN_POINT('Ctrl Pts',(3.0096491810855,-1.,2.87876560072799));
#39282=CARTESIAN_POINT('Ctrl Pts',(3.01240727309568,-1.,2.88608751706796));
#39283=CARTESIAN_POINT('Ctrl Pts',(3.01513660433291,-1.,2.8934292556764));
#39284=CARTESIAN_POINT('Ctrl Pts',(3.01783725123646,-1.,2.90079069102661));
#39285=CARTESIAN_POINT('Ctrl Pts',(3.01997487194926,-1.,2.90669553303902));
#39286=CARTESIAN_POINT('Ctrl Pts',(3.02156522743299,-1.,2.91113297349052));
#39287=CARTESIAN_POINT('Ctrl Pts',(3.02261975104912,-1.,2.91409518070707));
#39288=CARTESIAN_POINT('Ctrl Pts',(3.02314558451372,-1.,2.91557726271063));
#39289=CARTESIAN_POINT('',(2.91557726271063,-1.,3.02314558451372));
#39290=CARTESIAN_POINT('',(3.02314558451372,-1.,2.91557726271063));
#39291=CARTESIAN_POINT('',(2.50410331873176,-1.,2.79140942341258));
#39292=CARTESIAN_POINT('Ctrl Pts',(2.91557726271063,-1.,3.02314558451372));
#39293=CARTESIAN_POINT('Ctrl Pts',(2.91409518070399,-1.,3.02261975104593));
#39294=CARTESIAN_POINT('Ctrl Pts',(2.91113297348212,-1.,3.02156522742431));
#39295=CARTESIAN_POINT('Ctrl Pts',(2.90669553302526,-1.,3.01997487193503));
#39296=CARTESIAN_POINT('Ctrl Pts',(2.9007906910105,-1.,3.01783725121981));
#39297=CARTESIAN_POINT('Ctrl Pts',(2.89342925566321,-1.,3.01513660431928));
#39298=CARTESIAN_POINT('Ctrl Pts',(2.8860875170608,-1.,3.01240727308829));
#39299=CARTESIAN_POINT('Ctrl Pts',(2.87876560072727,-1.,3.00964918108476));
#39300=CARTESIAN_POINT('Ctrl Pts',(2.87146368430501,-1.,3.00686224485784));
#39301=CARTESIAN_POINT('Ctrl Pts',(2.86418200833667,-1.,3.00404638316867));
#39302=CARTESIAN_POINT('Ctrl Pts',(2.85692085715685,-1.,3.00120150796095));
#39303=CARTESIAN_POINT('Ctrl Pts',(2.84968053289451,-1.,2.99832751144925));
#39304=CARTESIAN_POINT('Ctrl Pts',(2.84246132984415,-1.,2.99542425341685));
#39305=CARTESIAN_POINT('Ctrl Pts',(2.83526351254248,-1.,2.9924915517034));
#39306=CARTESIAN_POINT('Ctrl Pts',(2.82808728190157,-1.,2.98952916401446));
#39307=CARTESIAN_POINT('Ctrl Pts',(2.82093279065457,-1.,2.9865368066918));
#39308=CARTESIAN_POINT('Ctrl Pts',(2.81380019196286,-1.,2.98351419779767));
#39309=CARTESIAN_POINT('Ctrl Pts',(2.80668968101106,-1.,2.98046109647241));
#39310=CARTESIAN_POINT('Ctrl Pts',(2.7996015327823,-1.,2.97737733718287));
#39311=CARTESIAN_POINT('Ctrl Pts',(2.79253615718248,-1.,2.9742628834758));
#39312=CARTESIAN_POINT('Ctrl Pts',(2.78549409123769,-1.,2.97111781461465));
#39313=CARTESIAN_POINT('Ctrl Pts',(2.7784758954285,-1.,2.96794221043036));
#39314=CARTESIAN_POINT('Ctrl Pts',(2.77148206836498,-1.,2.96473605585583));
#39315=CARTESIAN_POINT('Ctrl Pts',(2.76451296269557,-1.,2.96149914764818));
#39316=CARTESIAN_POINT('Ctrl Pts',(2.7575686788835,-1.,2.95823097665896));
#39317=CARTESIAN_POINT('Ctrl Pts',(2.75064903318947,-1.,2.95493069316161));
#39318=CARTESIAN_POINT('Ctrl Pts',(2.74375379492172,-1.,2.95159737214266));
#39319=CARTESIAN_POINT('Ctrl Pts',(2.73688288329808,-1.,2.94823023414364));
#39320=CARTESIAN_POINT('Ctrl Pts',(2.73003657371616,-1.,2.94482887675143));
#39321=CARTESIAN_POINT('Ctrl Pts',(2.72321571511337,-1.,2.94139351933897));
#39322=CARTESIAN_POINT('Ctrl Pts',(2.71642190053592,-1.,2.93792519474972));
#39323=CARTESIAN_POINT('Ctrl Pts',(2.70965695523787,-1.,2.93442516311179));
#39324=CARTESIAN_POINT('Ctrl Pts',(2.70292247416885,-1.,2.9308943823375));
#39325=CARTESIAN_POINT('Ctrl Pts',(2.69621932864301,-1.,2.92733294395267));
#39326=CARTESIAN_POINT('Ctrl Pts',(2.68954721165339,-1.,2.92373955325875));
#39327=CARTESIAN_POINT('Ctrl Pts',(2.68290409279688,-1.,2.92011090722152));
#39328=CARTESIAN_POINT('Ctrl Pts',(2.67628728855312,-1.,2.91644290704285));
#39329=CARTESIAN_POINT('Ctrl Pts',(2.66969458792631,-1.,2.91273193382882));
#39330=CARTESIAN_POINT('Ctrl Pts',(2.6631254261681,-1.,2.90897617968923));
#39331=CARTESIAN_POINT('Ctrl Pts',(2.65658188464282,-1.,2.90517678087461));
#39332=CARTESIAN_POINT('Ctrl Pts',(2.65007017365564,-1.,2.90133950224867));
#39333=CARTESIAN_POINT('Ctrl Pts',(2.64359851684131,-1.,2.89747231723345));
#39334=CARTESIAN_POINT('Ctrl Pts',(2.63717442263932,-1.,2.89358228854544));
#39335=CARTESIAN_POINT('Ctrl Pts',(2.63080195420767,-1.,2.88967244854239));
#39336=CARTESIAN_POINT('Ctrl Pts',(2.62447947640262,-1.,2.88573922195059));
#39337=CARTESIAN_POINT('Ctrl Pts',(2.61819596473108,-1.,2.88176821427525));
#39338=CARTESIAN_POINT('Ctrl Pts',(2.61193507170955,-1.,2.87773881947916));
#39339=CARTESIAN_POINT('Ctrl Pts',(2.60568177881303,-1.,2.87363176656501));
#39340=CARTESIAN_POINT('Ctrl Pts',(2.5994287522321,-1.,2.86943633170722));
#39341=CARTESIAN_POINT('Ctrl Pts',(2.59318160184908,-1.,2.86515629953513));
#39342=CARTESIAN_POINT('Ctrl Pts',(2.58696770643524,-1.,2.86081999003629));
#39343=CARTESIAN_POINT('Ctrl Pts',(2.58082875254357,-1.,2.85647171715092));
#39344=CARTESIAN_POINT('Ctrl Pts',(2.57480482727081,-1.,2.85215360144431));
#39345=CARTESIAN_POINT('Ctrl Pts',(2.56891984251721,-1.,2.84788893329067));
#39346=CARTESIAN_POINT('Ctrl Pts',(2.56316920798513,-1.,2.84366802680237));
#39347=CARTESIAN_POINT('Ctrl Pts',(2.55749952145241,-1.,2.83942515220782));
#39348=CARTESIAN_POINT('Ctrl Pts',(2.55182152807077,-1.,2.83505269592536));
#39349=CARTESIAN_POINT('Ctrl Pts',(2.54604736792655,-1.,2.83044254225917));
#39350=CARTESIAN_POINT('Ctrl Pts',(2.54012272520199,-1.,2.8255216764922));
#39351=CARTESIAN_POINT('Ctrl Pts',(2.53405679667412,-1.,2.82028550483689));
#39352=CARTESIAN_POINT('Ctrl Pts',(2.52796388055278,-1.,2.81484379048475));
#39353=CARTESIAN_POINT('Ctrl Pts',(2.52205778589653,-1.,2.80941521966941));
#39354=CARTESIAN_POINT('Ctrl Pts',(2.51660190465805,-1.,2.80427363984653));
#39355=CARTESIAN_POINT('Ctrl Pts',(2.51186983687818,-1.,2.79970585014168));
#39356=CARTESIAN_POINT('Ctrl Pts',(2.5081055597767,-1.,2.79596878057287));
#39357=CARTESIAN_POINT('Ctrl Pts',(2.50567182569081,-1.,2.79344192164147));
#39358=CARTESIAN_POINT('Ctrl Pts',(2.50455968395146,-1.,2.79217568804755));
#39359=CARTESIAN_POINT('Ctrl Pts',(2.50417932839313,-1.,2.79164172518905));
#39360=CARTESIAN_POINT('Ctrl Pts',(2.50410700351493,-1.,2.79145823440781));
#39361=CARTESIAN_POINT('Ctrl Pts',(2.50410331873176,-1.,2.79140942341258));
#39362=CARTESIAN_POINT('',(2.36531447826213,-1.,2.90994629141563));
#39363=CARTESIAN_POINT('Origin',(0.,-1.,0.));
#39364=CARTESIAN_POINT('',(2.52982887637028,-1.,3.35260583073571));
#39365=CARTESIAN_POINT('Ctrl Pts',(2.36531447826213,-1.,2.90994629141563));
#39366=CARTESIAN_POINT('Ctrl Pts',(2.3653621118858,-1.,2.90995756655559));
#39367=CARTESIAN_POINT('Ctrl Pts',(2.36553202948741,-1.,2.9100577052777));
#39368=CARTESIAN_POINT('Ctrl Pts',(2.36599991765853,-1.,2.91051690822262));
#39369=CARTESIAN_POINT('Ctrl Pts',(2.36707658451709,-1.,2.91181344022628));
#39370=CARTESIAN_POINT('Ctrl Pts',(2.36919161373074,-1.,2.91461249883016));
#39371=CARTESIAN_POINT('Ctrl Pts',(2.37229381109939,-1.,2.9189150379156));
#39372=CARTESIAN_POINT('Ctrl Pts',(2.37606510524271,-1.,2.92430340582912));
#39373=CARTESIAN_POINT('Ctrl Pts',(2.3802898958232,-1.,2.93049643640517));
#39374=CARTESIAN_POINT('Ctrl Pts',(2.38472771516476,-1.,2.93717903280599));
#39375=CARTESIAN_POINT('Ctrl Pts',(2.38914929090806,-1.,2.94404820669135));
#39376=CARTESIAN_POINT('Ctrl Pts',(2.39337207631613,-1.,2.95085857128372));
#39377=CARTESIAN_POINT('Ctrl Pts',(2.39730553974412,-1.,2.95748006482811));
#39378=CARTESIAN_POINT('Ctrl Pts',(2.40095565711535,-1.,2.96390432240181));
#39379=CARTESIAN_POINT('Ctrl Pts',(2.40438604734848,-1.,2.97019641312272));
#39380=CARTESIAN_POINT('Ctrl Pts',(2.40768975073691,-1.,2.97646002822395));
#39381=CARTESIAN_POINT('Ctrl Pts',(2.41095909342591,-1.,2.98280015815132));
#39382=CARTESIAN_POINT('Ctrl Pts',(2.4142506419963,-1.,2.98927983005851));
#39383=CARTESIAN_POINT('Ctrl Pts',(2.4175732450056,-1.,2.99590509293561));
#39384=CARTESIAN_POINT('Ctrl Pts',(2.42090763946812,-1.,3.00264868586038));
#39385=CARTESIAN_POINT('Ctrl Pts',(2.42421849439625,-1.,3.00946442616674));
#39386=CARTESIAN_POINT('Ctrl Pts',(2.4274685626416,-1.,3.01630420830494));
#39387=CARTESIAN_POINT('Ctrl Pts',(2.43063415586615,-1.,3.02313656035977));
#39388=CARTESIAN_POINT('Ctrl Pts',(2.43371241361462,-1.,3.02995534946946));
#39389=CARTESIAN_POINT('Ctrl Pts',(2.43671278042394,-1.,3.03676949672797));
#39390=CARTESIAN_POINT('Ctrl Pts',(2.43965194061849,-1.,3.04359685040545));
#39391=CARTESIAN_POINT('Ctrl Pts',(2.44254768923109,-1.,3.05045678021509));
#39392=CARTESIAN_POINT('Ctrl Pts',(2.44541251892568,-1.,3.05736242671521));
#39393=CARTESIAN_POINT('Ctrl Pts',(2.44824970516557,-1.,3.06431596421422));
#39394=CARTESIAN_POINT('Ctrl Pts',(2.45105688854432,-1.,3.0713129052131));
#39395=CARTESIAN_POINT('Ctrl Pts',(2.45382826787795,-1.,3.07834472886145));
#39396=CARTESIAN_POINT('Ctrl Pts',(2.45655725437037,-1.,3.08540206545313));
#39397=CARTESIAN_POINT('Ctrl Pts',(2.45923912563875,-1.,3.09247787931881));
#39398=CARTESIAN_POINT('Ctrl Pts',(2.4618730850188,-1.,3.09956993697048));
#39399=CARTESIAN_POINT('Ctrl Pts',(2.46446082979645,-1.,3.10667907901981));
#39400=CARTESIAN_POINT('Ctrl Pts',(2.46700558843507,-1.,3.11380805536124));
#39401=CARTESIAN_POINT('Ctrl Pts',(2.4695109894747,-1.,3.12096015766984));
#39402=CARTESIAN_POINT('Ctrl Pts',(2.47197997765868,-1.,3.12813790805948));
#39403=CARTESIAN_POINT('Ctrl Pts',(2.47441378371923,-1.,3.13534181229282));
#39404=CARTESIAN_POINT('Ctrl Pts',(2.47681245356095,-1.,3.14257099546531));
#39405=CARTESIAN_POINT('Ctrl Pts',(2.47917529057016,-1.,3.14982373241335));
#39406=CARTESIAN_POINT('Ctrl Pts',(2.48150133566568,-1.,3.15709802322735));
#39407=CARTESIAN_POINT('Ctrl Pts',(2.48378981792739,-1.,3.16439213290181));
#39408=CARTESIAN_POINT('Ctrl Pts',(2.48604065348619,-1.,3.17170518863357));
#39409=CARTESIAN_POINT('Ctrl Pts',(2.48825428288242,-1.,3.17903698136679));
#39410=CARTESIAN_POINT('Ctrl Pts',(2.49043146334095,-1.,3.18638771282315));
#39411=CARTESIAN_POINT('Ctrl Pts',(2.4925730723986,-1.,3.19375775555814));
#39412=CARTESIAN_POINT('Ctrl Pts',(2.49467992057726,-1.,3.20114742397549));
#39413=CARTESIAN_POINT('Ctrl Pts',(2.49675252647298,-1.,3.2085566984974));
#39414=CARTESIAN_POINT('Ctrl Pts',(2.49879114599293,-1.,3.21598526261157));
#39415=CARTESIAN_POINT('Ctrl Pts',(2.5007958720187,-1.,3.22343262620387));
#39416=CARTESIAN_POINT('Ctrl Pts',(2.50276671338074,-1.,3.23089822320596));
#39417=CARTESIAN_POINT('Ctrl Pts',(2.50470367580078,-1.,3.23838151080383));
#39418=CARTESIAN_POINT('Ctrl Pts',(2.50660685940645,-1.,3.24588208984042));
#39419=CARTESIAN_POINT('Ctrl Pts',(2.50847647070936,-1.,3.25339971461265));
#39420=CARTESIAN_POINT('Ctrl Pts',(2.51031277813697,-1.,3.26093423001716));
#39421=CARTESIAN_POINT('Ctrl Pts',(2.51211608411539,-1.,3.26848552888271));
#39422=CARTESIAN_POINT('Ctrl Pts',(2.51388669270329,-1.,3.27605350473048));
#39423=CARTESIAN_POINT('Ctrl Pts',(2.51562487464214,-1.,3.28363799702583));
#39424=CARTESIAN_POINT('Ctrl Pts',(2.51733085123316,-1.,3.2912387729863));
#39425=CARTESIAN_POINT('Ctrl Pts',(2.51900480700548,-1.,3.29885556387661));
#39426=CARTESIAN_POINT('Ctrl Pts',(2.52064689568167,-1.,3.30648808814986));
#39427=CARTESIAN_POINT('Ctrl Pts',(2.52225724871375,-1.,3.31413607874727));
#39428=CARTESIAN_POINT('Ctrl Pts',(2.52383598396878,-1.,3.32179931079521));
#39429=CARTESIAN_POINT('Ctrl Pts',(2.52538321165774,-1.,3.32947762189049));
#39430=CARTESIAN_POINT('Ctrl Pts',(2.52689902691551,-1.,3.33717090000955));
#39431=CARTESIAN_POINT('Ctrl Pts',(2.52808660916879,-1.,3.34333744117093));
#39432=CARTESIAN_POINT('Ctrl Pts',(2.5289632161143,-1.,3.34796903577628));
#39433=CARTESIAN_POINT('Ctrl Pts',(2.52954136549357,-1.,3.35105973714426));
#39434=CARTESIAN_POINT('Ctrl Pts',(2.52982887637028,-1.,3.35260583073571));
#39435=CARTESIAN_POINT('',(2.40675750623143,-1.,3.44202241512147));
#39436=CARTESIAN_POINT('',(2.52982887637028,-1.,3.35260583073571));
#39437=CARTESIAN_POINT('',(2.03660101169714,-1.,3.14877060440328));
#39438=CARTESIAN_POINT('Ctrl Pts',(2.40675750623143,-1.,3.44202241512147));
#39439=CARTESIAN_POINT('Ctrl Pts',(2.4053759295909,-1.,3.44127120683039));
#39440=CARTESIAN_POINT('Ctrl Pts',(2.40261515589405,-1.,3.43976627484234));
#39441=CARTESIAN_POINT('Ctrl Pts',(2.39848113410292,-1.,3.43750133064416));
#39442=CARTESIAN_POINT('Ctrl Pts',(2.39298338804493,-1.,3.4344663067854));
#39443=CARTESIAN_POINT('Ctrl Pts',(2.38613505843552,-1.,3.4306473271292));
#39444=CARTESIAN_POINT('Ctrl Pts',(2.37931067028926,-1.,3.42680309754399));
#39445=CARTESIAN_POINT('Ctrl Pts',(2.37251035954292,-1.,3.42293356216511));
#39446=CARTESIAN_POINT('Ctrl Pts',(2.36573431470642,-1.,3.41903866635852));
#39447=CARTESIAN_POINT('Ctrl Pts',(2.35898278606946,-1.,3.41511836751469));
#39448=CARTESIAN_POINT('Ctrl Pts',(2.35225606824109,-1.,3.41117262314119));
#39449=CARTESIAN_POINT('Ctrl Pts',(2.34555447649188,-1.,3.40720137404297));
#39450=CARTESIAN_POINT('Ctrl Pts',(2.33887832342782,-1.,3.40320452776743));
#39451=CARTESIAN_POINT('Ctrl Pts',(2.33222789882489,-1.,3.39918194577956));
#39452=CARTESIAN_POINT('Ctrl Pts',(2.3256034390248,-1.,3.39513342019756));
#39453=CARTESIAN_POINT('Ctrl Pts',(2.31900513925424,-1.,3.39105869474822));
#39454=CARTESIAN_POINT('Ctrl Pts',(2.31243319489367,-1.,3.38695751492462));
#39455=CARTESIAN_POINT('Ctrl Pts',(2.30588783640343,-1.,3.3828296733661));
#39456=CARTESIAN_POINT('Ctrl Pts',(2.29936936127624,-1.,3.37867504959433));
#39457=CARTESIAN_POINT('Ctrl Pts',(2.29287818007393,-1.,3.37449367172826));
#39458=CARTESIAN_POINT('Ctrl Pts',(2.28641481081137,-1.,3.37028570206488));
#39459=CARTESIAN_POINT('Ctrl Pts',(2.27997979458037,-1.,3.36605130713076));
#39460=CARTESIAN_POINT('Ctrl Pts',(2.2735736262093,-1.,3.36179055004409));
#39461=CARTESIAN_POINT('Ctrl Pts',(2.26719668579909,-1.,3.35750328523061));
#39462=CARTESIAN_POINT('Ctrl Pts',(2.26084915222449,-1.,3.35318902552626));
#39463=CARTESIAN_POINT('Ctrl Pts',(2.25453097693483,-1.,3.34884690292285));
#39464=CARTESIAN_POINT('Ctrl Pts',(2.24824207678256,-1.,3.34447596770723));
#39465=CARTESIAN_POINT('Ctrl Pts',(2.24198249391422,-1.,3.34007543738025));
#39466=CARTESIAN_POINT('Ctrl Pts',(2.23575256328812,-1.,3.33564495756482));
#39467=CARTESIAN_POINT('Ctrl Pts',(2.22955308907233,-1.,3.33118487773611));
#39468=CARTESIAN_POINT('Ctrl Pts',(2.22338548312772,-1.,3.3266964672289));
#39469=CARTESIAN_POINT('Ctrl Pts',(2.21725135110898,-1.,3.32218125618968));
#39470=CARTESIAN_POINT('Ctrl Pts',(2.21115211847875,-1.,3.31764044024235));
#39471=CARTESIAN_POINT('Ctrl Pts',(2.20508863150607,-1.,3.31307424608949));
#39472=CARTESIAN_POINT('Ctrl Pts',(2.19906078949922,-1.,3.30848134694595));
#39473=CARTESIAN_POINT('Ctrl Pts',(2.19306710376111,-1.,3.30385816281831));
#39474=CARTESIAN_POINT('Ctrl Pts',(2.18710556500327,-1.,3.29920022557639));
#39475=CARTESIAN_POINT('Ctrl Pts',(2.18117455557065,-1.,3.2945036150049));
#39476=CARTESIAN_POINT('Ctrl Pts',(2.17527380048423,-1.,3.28976645712568));
#39477=CARTESIAN_POINT('Ctrl Pts',(2.16940517773455,-1.,3.28499019979724));
#39478=CARTESIAN_POINT('Ctrl Pts',(2.16357391934425,-1.,3.280181508414));
#39479=CARTESIAN_POINT('Ctrl Pts',(2.15778690038347,-1.,3.27534954469187));
#39480=CARTESIAN_POINT('Ctrl Pts',(2.15205043199808,-1.,3.27050245897228));
#39481=CARTESIAN_POINT('Ctrl Pts',(2.1463680529566,-1.,3.26564388189759));
#39482=CARTESIAN_POINT('Ctrl Pts',(2.14073870754264,-1.,3.26077002641879));
#39483=CARTESIAN_POINT('Ctrl Pts',(2.13515375878803,-1.,3.25586495065054));
#39484=CARTESIAN_POINT('Ctrl Pts',(2.12960028396832,-1.,3.25090574494028));
#39485=CARTESIAN_POINT('Ctrl Pts',(2.12406646410962,-1.,3.24587102613376));
#39486=CARTESIAN_POINT('Ctrl Pts',(2.11854673326979,-1.,3.24074905517293));
#39487=CARTESIAN_POINT('Ctrl Pts',(2.11304604021773,-1.,3.23554444767099));
#39488=CARTESIAN_POINT('Ctrl Pts',(2.10758699642451,-1.,3.23028945793289));
#39489=CARTESIAN_POINT('Ctrl Pts',(2.10220384298492,-1.,3.22503437553434));
#39490=CARTESIAN_POINT('Ctrl Pts',(2.09692958434895,-1.,3.21982707347009));
#39491=CARTESIAN_POINT('Ctrl Pts',(2.09178419460443,-1.,3.21469429601654));
#39492=CARTESIAN_POINT('Ctrl Pts',(2.08676465517455,-1.,3.20962575845463));
#39493=CARTESIAN_POINT('Ctrl Pts',(2.08182850370878,-1.,3.2045481863073));
#39494=CARTESIAN_POINT('Ctrl Pts',(2.07690441870722,-1.,3.19934132836019));
#39495=CARTESIAN_POINT('Ctrl Pts',(2.07192253497857,-1.,3.19388465568252));
#39496=CARTESIAN_POINT('Ctrl Pts',(2.06684062744112,-1.,3.18809755562368));
#39497=CARTESIAN_POINT('Ctrl Pts',(2.06166849827101,-1.,3.18197692964614));
#39498=CARTESIAN_POINT('Ctrl Pts',(2.05650186773132,-1.,3.17564906975371));
#39499=CARTESIAN_POINT('Ctrl Pts',(2.05151770247233,-1.,3.16936341689527));
#39500=CARTESIAN_POINT('Ctrl Pts',(2.04693331247446,-1.,3.16343165058912));
#39501=CARTESIAN_POINT('Ctrl Pts',(2.04297406404027,-1.,3.15817983946367));
#39502=CARTESIAN_POINT('Ctrl Pts',(2.03984073791519,-1.,3.15389991674792));
#39503=CARTESIAN_POINT('Ctrl Pts',(2.03783225495961,-1.,3.15102344775328));
#39504=CARTESIAN_POINT('Ctrl Pts',(2.03693188810544,-1.,3.14959882629805));
#39505=CARTESIAN_POINT('Ctrl Pts',(2.03663974554932,-1.,3.1490119366901));
#39506=CARTESIAN_POINT('Ctrl Pts',(2.03659701539259,-1.,3.14881939088124));
#39507=CARTESIAN_POINT('Ctrl Pts',(2.03660101169714,-1.,3.14877060440328));
#39508=CARTESIAN_POINT('',(1.88097764062697,-1.,3.24413672884812));
#39509=CARTESIAN_POINT('Origin',(0.,-1.,0.));
#39510=CARTESIAN_POINT('',(1.97421938526992,-1.,3.70708211654725));
#39511=CARTESIAN_POINT('Ctrl Pts',(1.88097764062697,-1.,3.24413672884812));
#39512=CARTESIAN_POINT('Ctrl Pts',(1.8810229239812,-1.,3.24415531671284));
#39513=CARTESIAN_POINT('Ctrl Pts',(1.88117508446775,-1.,3.24428080353022));
#39514=CARTESIAN_POINT('Ctrl Pts',(1.88156537699203,-1.,3.24480754676064));
#39515=CARTESIAN_POINT('Ctrl Pts',(1.88242596600454,-1.,3.2462565441079));
#39516=CARTESIAN_POINT('Ctrl Pts',(1.88407708646357,-1.,3.24935200511918));
#39517=CARTESIAN_POINT('Ctrl Pts',(1.88646802523466,-1.,3.25408686339463));
#39518=CARTESIAN_POINT('Ctrl Pts',(1.88934996203698,-1.,3.25999885193947));
#39519=CARTESIAN_POINT('Ctrl Pts',(1.89255393500965,-1.,3.26677653888676));
#39520=CARTESIAN_POINT('Ctrl Pts',(1.89589172903793,-1.,3.27407108933139));
#39521=CARTESIAN_POINT('Ctrl Pts',(1.89918429230462,-1.,3.28154737912352));
#39522=CARTESIAN_POINT('Ctrl Pts',(1.90228971247527,-1.,3.2889344860029));
#39523=CARTESIAN_POINT('Ctrl Pts',(1.90513891864087,-1.,3.29608978722113));
#39524=CARTESIAN_POINT('Ctrl Pts',(1.90773912171341,-1.,3.30300595568195));
#39525=CARTESIAN_POINT('Ctrl Pts',(1.91014297830446,-1.,3.30975721158596));
#39526=CARTESIAN_POINT('Ctrl Pts',(1.91242616234442,-1.,3.31646052426364));
#39527=CARTESIAN_POINT('Ctrl Pts',(1.91466343916627,-1.,3.32323403454535));
#39528=CARTESIAN_POINT('Ctrl Pts',(1.91690081930331,-1.,3.33014884257873));
#39529=CARTESIAN_POINT('Ctrl Pts',(1.9191460961021,-1.,3.33721230710012));
#39530=CARTESIAN_POINT('Ctrl Pts',(1.92138450828404,-1.,3.34439448941961));
#39531=CARTESIAN_POINT('Ctrl Pts',(1.92358838440528,-1.,3.35164424847223));
#39532=CARTESIAN_POINT('Ctrl Pts',(1.92572846125756,-1.,3.35890824422965));
#39533=CARTESIAN_POINT('Ctrl Pts',(1.92778626543786,-1.,3.36615168657567));
#39534=CARTESIAN_POINT('Ctrl Pts',(1.92975993109877,-1.,3.37336807068043));
#39535=CARTESIAN_POINT('Ctrl Pts',(1.93165739093276,-1.,3.3805676852555));
#39536=CARTESIAN_POINT('Ctrl Pts',(1.93349233176788,-1.,3.38777076883256));
#39537=CARTESIAN_POINT('Ctrl Pts',(1.93527929945985,-1.,3.39499923640795));
#39538=CARTESIAN_POINT('Ctrl Pts',(1.93702857723098,-1.,3.40226802104109));
#39539=CARTESIAN_POINT('Ctrl Pts',(1.93874306008143,-1.,3.40957978266642));
#39540=CARTESIAN_POINT('Ctrl Pts',(1.94042111965246,-1.,3.41692971994096));
#39541=CARTESIAN_POINT('Ctrl Pts',(1.94205835913696,-1.,3.42430850941503));
#39542=CARTESIAN_POINT('Ctrl Pts',(1.94364973660284,-1.,3.43170586602434));
#39543=CARTESIAN_POINT('Ctrl Pts',(1.94519168842879,-1.,3.43911410197687));
#39544=CARTESIAN_POINT('Ctrl Pts',(1.94668377715329,-1.,3.44653088665681));
#39545=CARTESIAN_POINT('Ctrl Pts',(1.94812754766524,-1.,3.45395731584051));
#39546=CARTESIAN_POINT('Ctrl Pts',(1.94952575850197,-1.,3.46139661060962));
#39547=CARTESIAN_POINT('Ctrl Pts',(1.95088147859876,-1.,3.46885258974191));
#39548=CARTESIAN_POINT('Ctrl Pts',(1.95219722189876,-1.,3.47632820495921));
#39549=CARTESIAN_POINT('Ctrl Pts',(1.95347412486308,-1.,3.48382414832634));
#39550=CARTESIAN_POINT('Ctrl Pts',(1.95471236969643,-1.,3.49133956289133));
#39551=CARTESIAN_POINT('Ctrl Pts',(1.95591153823661,-1.,3.49887263575583));
#39552=CARTESIAN_POINT('Ctrl Pts',(1.95707099606511,-1.,3.50642124159909));
#39553=CARTESIAN_POINT('Ctrl Pts',(1.95819025316779,-1.,3.51398354617794));
#39554=CARTESIAN_POINT('Ctrl Pts',(1.95926936324461,-1.,3.52155867431486));
#39555=CARTESIAN_POINT('Ctrl Pts',(1.96030879411566,-1.,3.52914648844351));
#39556=CARTESIAN_POINT('Ctrl Pts',(1.96130926212689,-1.,3.53674730625813));
#39557=CARTESIAN_POINT('Ctrl Pts',(1.96227157573067,-1.,3.54436163300443));
#39558=CARTESIAN_POINT('Ctrl Pts',(1.96319648628644,-1.,3.55198990600886));
#39559=CARTESIAN_POINT('Ctrl Pts',(1.96408450906812,-1.,3.55963218706096));
#39560=CARTESIAN_POINT('Ctrl Pts',(1.96493594634567,-1.,3.56728820357791));
#39561=CARTESIAN_POINT('Ctrl Pts',(1.96575096652789,-1.,3.57495748600959));
#39562=CARTESIAN_POINT('Ctrl Pts',(1.96652966688911,-1.,3.58263947663829));
#39563=CARTESIAN_POINT('Ctrl Pts',(1.96727213799544,-1.,3.59033364022801));
#39564=CARTESIAN_POINT('Ctrl Pts',(1.96797854118369,-1.,3.59803959819938));
#39565=CARTESIAN_POINT('Ctrl Pts',(1.9686491188594,-1.,3.60575714017989));
#39566=CARTESIAN_POINT('Ctrl Pts',(1.96928416040877,-1.,3.61348615496704));
#39567=CARTESIAN_POINT('Ctrl Pts',(1.96988398129978,-1.,3.62122658401893));
#39568=CARTESIAN_POINT('Ctrl Pts',(1.97044889850463,-1.,3.62897836973293));
#39569=CARTESIAN_POINT('Ctrl Pts',(1.97097920454464,-1.,3.63674139590412));
#39570=CARTESIAN_POINT('Ctrl Pts',(1.97147515441164,-1.,3.64451546723514));
#39571=CARTESIAN_POINT('Ctrl Pts',(1.97193697240239,-1.,3.652300347166));
#39572=CARTESIAN_POINT('Ctrl Pts',(1.9723648543905,-1.,3.6600957816636));
#39573=CARTESIAN_POINT('Ctrl Pts',(1.97275897198678,-1.,3.66790152752075));
#39574=CARTESIAN_POINT('Ctrl Pts',(1.97311947678516,-1.,3.67571738107084));
#39575=CARTESIAN_POINT('Ctrl Pts',(1.97344650304519,-1.,3.68354319915092));
#39576=CARTESIAN_POINT('Ctrl Pts',(1.97374016225483,-1.,3.69137888599902));
#39577=CARTESIAN_POINT('Ctrl Pts',(1.97394846383216,-1.,3.6976552856004));
#39578=CARTESIAN_POINT('Ctrl Pts',(1.97408973726715,-1.,3.70236698912904));
#39579=CARTESIAN_POINT('Ctrl Pts',(1.97417727645308,-1.,3.70551008132332));
#39580=CARTESIAN_POINT('Ctrl Pts',(1.97421938526992,-1.,3.70708211654725));
#39581=CARTESIAN_POINT('',(1.8386753923786,-1.,3.77614523045147));
#39582=CARTESIAN_POINT('',(1.97421938526992,-1.,3.70708211654725));
#39583=CARTESIAN_POINT('',(1.5189508286633,-1.,3.42859860294306));
#39584=CARTESIAN_POINT('Ctrl Pts',(1.8386753923786,-1.,3.77614523045147));
#39585=CARTESIAN_POINT('Ctrl Pts',(1.83742834010626,-1.,3.77518714457833));
#39586=CARTESIAN_POINT('Ctrl Pts',(1.83493697934534,-1.,3.77326886064398));
#39587=CARTESIAN_POINT('Ctrl Pts',(1.83120816955645,-1.,3.77038509817999));
#39588=CARTESIAN_POINT('Ctrl Pts',(1.82625289220915,-1.,3.76652740353775));
#39589=CARTESIAN_POINT('Ctrl Pts',(1.82008629694091,-1.,3.76168412707948));
#39590=CARTESIAN_POINT('Ctrl Pts',(1.8139472983358,-1.,3.75681965683071));
#39591=CARTESIAN_POINT('Ctrl Pts',(1.80783603939617,-1.,3.75193395887977));
#39592=CARTESIAN_POINT('Ctrl Pts',(1.8017527148577,-1.,3.74702700875467));
#39593=CARTESIAN_POINT('Ctrl Pts',(1.79569757859422,-1.,3.74209880352445));
#39594=CARTESIAN_POINT('Ctrl Pts',(1.78967092823491,-1.,3.73714934730681));
#39595=CARTESIAN_POINT('Ctrl Pts',(1.78367308442901,-1.,3.7321786309547));
#39596=CARTESIAN_POINT('Ctrl Pts',(1.77770437039658,-1.,3.72718661205609));
#39597=CARTESIAN_POINT('Ctrl Pts',(1.77176509401761,-1.,3.72217319911254));
#39598=CARTESIAN_POINT('Ctrl Pts',(1.76585552124394,-1.,3.71713822377359));
#39599=CARTESIAN_POINT('Ctrl Pts',(1.75997588498865,-1.,3.71208146346136));
#39600=CARTESIAN_POINT('Ctrl Pts',(1.75412641804042,-1.,3.70700269736659));
#39601=CARTESIAN_POINT('Ctrl Pts',(1.74830738046057,-1.,3.7019017567335));
#39602=CARTESIAN_POINT('Ctrl Pts',(1.74251908492617,-1.,3.69677856910517));
#39603=CARTESIAN_POINT('Ctrl Pts',(1.73676193254557,-1.,3.69163322648036));
#39604=CARTESIAN_POINT('Ctrl Pts',(1.73103640956717,-1.,3.68646597019332));
#39605=CARTESIAN_POINT('Ctrl Pts',(1.72534302437056,-1.,3.68127704936579));
#39606=CARTESIAN_POINT('Ctrl Pts',(1.71968225581808,-1.,3.67606660374709));
#39607=CARTESIAN_POINT('Ctrl Pts',(1.71405450210383,-1.,3.67083454901611));
#39608=CARTESIAN_POINT('Ctrl Pts',(1.70846001610956,-1.,3.66558043198876));
#39609=CARTESIAN_POINT('Ctrl Pts',(1.70289888566873,-1.,3.66030338774847));
#39610=CARTESIAN_POINT('Ctrl Pts',(1.69737117722534,-1.,3.65500246526749));
#39611=CARTESIAN_POINT('Ctrl Pts',(1.69187705481689,-1.,3.64967689827371));
#39612=CARTESIAN_POINT('Ctrl Pts',(1.68641690471457,-1.,3.64432638915203));
#39613=CARTESIAN_POINT('Ctrl Pts',(1.68099146651586,-1.,3.63895140887462));
#39614=CARTESIAN_POINT('Ctrl Pts',(1.67560193613156,-1.,3.63355343201232));
#39615=CARTESIAN_POINT('Ctrl Pts',(1.67024966008044,-1.,3.62813422105271));
#39616=CARTESIAN_POINT('Ctrl Pts',(1.66493585923855,-1.,3.62269517989109));
#39617=CARTESIAN_POINT('Ctrl Pts',(1.65966133399186,-1.,3.61723666482456));
#39618=CARTESIAN_POINT('Ctrl Pts',(1.65442619244325,-1.,3.61175734965127));
#39619=CARTESIAN_POINT('Ctrl Pts',(1.64922952425832,-1.,3.60625346556992));
#39620=CARTESIAN_POINT('Ctrl Pts',(1.64407004385582,-1.,3.60072028513845));
#39621=CARTESIAN_POINT('Ctrl Pts',(1.63894676675352,-1.,3.59515368334893));
#39622=CARTESIAN_POINT('Ctrl Pts',(1.6338597145126,-1.,3.58955176627879));
#39623=CARTESIAN_POINT('Ctrl Pts',(1.62881051550745,-1.,3.58391625774343));
#39624=CARTESIAN_POINT('Ctrl Pts',(1.62380329464844,-1.,3.5782545595439));
#39625=CARTESIAN_POINT('Ctrl Pts',(1.61884340915404,-1.,3.57257679609806));
#39626=CARTESIAN_POINT('Ctrl Pts',(1.61393581747514,-1.,3.56689200468387));
#39627=CARTESIAN_POINT('Ctrl Pts',(1.60908344685457,-1.,3.5612043248298));
#39628=CARTESIAN_POINT('Ctrl Pts',(1.60428584699853,-1.,3.55550985096129));
#39629=CARTESIAN_POINT('Ctrl Pts',(1.59953698113457,-1.,3.54979148634454));
#39630=CARTESIAN_POINT('Ctrl Pts',(1.59482766949766,-1.,3.54402458182337));
#39631=CARTESIAN_POINT('Ctrl Pts',(1.59014958368739,-1.,3.53818616861077));
#39632=CARTESIAN_POINT('Ctrl Pts',(1.58549906268088,-1.,3.5322637814708));
#39633=CARTESIAN_POINT('Ctrl Pts',(1.58088027227848,-1.,3.52626275334881));
#39634=CARTESIAN_POINT('Ctrl Pts',(1.57631049988158,-1.,3.52021847865912));
#39635=CARTESIAN_POINT('Ctrl Pts',(1.57181569799743,-1.,3.51418598431665));
#39636=CARTESIAN_POINT('Ctrl Pts',(1.56742097575012,-1.,3.50821771695363));
#39637=CARTESIAN_POINT('Ctrl Pts',(1.56314187758675,-1.,3.50234321621578));
#39638=CARTESIAN_POINT('Ctrl Pts',(1.55897703097874,-1.,3.49655185179655));
#39639=CARTESIAN_POINT('Ctrl Pts',(1.55489595901116,-1.,3.4907646087742));
#39640=CARTESIAN_POINT('Ctrl Pts',(1.55084702970452,-1.,3.48485155928567));
#39641=CARTESIAN_POINT('Ctrl Pts',(1.54678009290276,-1.,3.47868272898751));
#39642=CARTESIAN_POINT('Ctrl Pts',(1.54266605398187,-1.,3.47217189224653));
#39643=CARTESIAN_POINT('Ctrl Pts',(1.53851507915502,-1.,3.46531752207153));
#39644=CARTESIAN_POINT('Ctrl Pts',(1.53440195378792,-1.,3.45825932955032));
#39645=CARTESIAN_POINT('Ctrl Pts',(1.53046244461635,-1.,3.45127136828305));
#39646=CARTESIAN_POINT('Ctrl Pts',(1.52686242875556,-1.,3.44469547526647));
#39647=CARTESIAN_POINT('Ctrl Pts',(1.5237734895035,-1.,3.4388889597401));
#39648=CARTESIAN_POINT('Ctrl Pts',(1.52134826724292,-1.,3.43417156977893));
#39649=CARTESIAN_POINT('Ctrl Pts',(1.5198144909338,-1.,3.43101631893414));
#39650=CARTESIAN_POINT('Ctrl Pts',(1.51914806898491,-1.,3.42946838852587));
#39651=CARTESIAN_POINT('Ctrl Pts',(1.5189513329503,-1.,3.42884302333841));
#39652=CARTESIAN_POINT('Ctrl Pts',(1.51893924967331,-1.,3.42864616361875));
#39653=CARTESIAN_POINT('Ctrl Pts',(1.5189508286633,-1.,3.42859860294306));
#39654=CARTESIAN_POINT('',(1.35032489087269,-1.,3.49844575334386));
#39655=CARTESIAN_POINT('Origin',(0.,-1.,0.));
#39656=CARTESIAN_POINT('',(1.36999806084572,-1.,3.97027773754922));
#39657=CARTESIAN_POINT('Ctrl Pts',(1.35032489087269,-1.,3.49844575334386));
#39658=CARTESIAN_POINT('Ctrl Pts',(1.35036670893102,-1.,3.49847119623841));
#39659=CARTESIAN_POINT('Ctrl Pts',(1.35049736560633,-1.,3.49861894124915));
#39660=CARTESIAN_POINT('Ctrl Pts',(1.35080045218652,-1.,3.49920025459856));
#39661=CARTESIAN_POINT('Ctrl Pts',(1.35142377279535,-1.,3.5007660381658));
#39662=CARTESIAN_POINT('Ctrl Pts',(1.3525703284343,-1.,3.50408168106113));
#39663=CARTESIAN_POINT('Ctrl Pts',(1.35419113576022,-1.,3.50913227060177));
#39664=CARTESIAN_POINT('Ctrl Pts',(1.35611275237288,-1.,3.51542230699919));
#39665=CARTESIAN_POINT('Ctrl Pts',(1.35821701528975,-1.,3.52261776117121));
#39666=CARTESIAN_POINT('Ctrl Pts',(1.36037259643827,-1.,3.53034464961849));
#39667=CARTESIAN_POINT('Ctrl Pts',(1.36245507339334,-1.,3.53824396425032));
#39668=CARTESIAN_POINT('Ctrl Pts',(1.36436666257567,-1.,3.54602591832893));
#39669=CARTESIAN_POINT('Ctrl Pts',(1.36606145456711,-1.,3.55353883995793));
#39670=CARTESIAN_POINT('Ctrl Pts',(1.36754771771174,-1.,3.56077662028492));
#39671=CARTESIAN_POINT('Ctrl Pts',(1.36886584973349,-1.,3.56782080304554));
#39672=CARTESIAN_POINT('Ctrl Pts',(1.37007229485646,-1.,3.57479875549453));
#39673=CARTESIAN_POINT('Ctrl Pts',(1.37122241663073,-1.,3.58183885982745));
#39674=CARTESIAN_POINT('Ctrl Pts',(1.37235053661,-1.,3.5890185384643));
#39675=CARTESIAN_POINT('Ctrl Pts',(1.37346320103184,-1.,3.59634627869117));
#39676=CARTESIAN_POINT('Ctrl Pts',(1.37455051379642,-1.,3.60379020124038));
#39677=CARTESIAN_POINT('Ctrl Pts',(1.37559314436641,-1.,3.61129546591082));
#39678=CARTESIAN_POINT('Ctrl Pts',(1.37657053403102,-1.,3.61880481160408));
#39679=CARTESIAN_POINT('Ctrl Pts',(1.37746987919868,-1.,3.62628098665112));
#39680=CARTESIAN_POINT('Ctrl Pts',(1.37829035457324,-1.,3.63371727442448));
#39681=CARTESIAN_POINT('Ctrl Pts',(1.37903818567347,-1.,3.64112507791112));
#39682=CARTESIAN_POINT('Ctrl Pts',(1.37972372481598,-1.,3.64852652756444));
#39683=CARTESIAN_POINT('Ctrl Pts',(1.38035791051215,-1.,3.65594554404396));
#39684=CARTESIAN_POINT('Ctrl Pts',(1.38094856333558,-1.,3.66339848520874));
#39685=CARTESIAN_POINT('Ctrl Pts',(1.38149812653876,-1.,3.67088843112282));
#39686=CARTESIAN_POINT('Ctrl Pts',(1.38200574290626,-1.,3.6784103848243));
#39687=CARTESIAN_POINT('Ctrl Pts',(1.38246852827185,-1.,3.68595444983844));
#39688=CARTESIAN_POINT('Ctrl Pts',(1.38288311171649,-1.,3.69350967899523));
#39689=CARTESIAN_POINT('Ctrl Pts',(1.38324717612862,-1.,3.70106792167894));
#39690=CARTESIAN_POINT('Ctrl Pts',(1.38356065402122,-1.,3.70862680753343));
#39691=CARTESIAN_POINT('Ctrl Pts',(1.38382489984585,-1.,3.7161876605181));
#39692=CARTESIAN_POINT('Ctrl Pts',(1.3840421342895,-1.,3.72375409358805));
#39693=CARTESIAN_POINT('Ctrl Pts',(1.38421479111531,-1.,3.73133035859283));
#39694=CARTESIAN_POINT('Ctrl Pts',(1.38434489156456,-1.,3.73891976418099));
#39695=CARTESIAN_POINT('Ctrl Pts',(1.38443344984389,-1.,3.7465231716786));
#39696=CARTESIAN_POINT('Ctrl Pts',(1.38448077997155,-1.,3.75413976318727));
#39697=CARTESIAN_POINT('Ctrl Pts',(1.38448675253343,-1.,3.76176768271347));
#39698=CARTESIAN_POINT('Ctrl Pts',(1.38445107339517,-1.,3.76940473185775));
#39699=CARTESIAN_POINT('Ctrl Pts',(1.38437354551435,-1.,3.77704902230441));
#39700=CARTESIAN_POINT('Ctrl Pts',(1.38425435883773,-1.,3.78469969805134));
#39701=CARTESIAN_POINT('Ctrl Pts',(1.38409399694588,-1.,3.79235669640907));
#39702=CARTESIAN_POINT('Ctrl Pts',(1.38389311766701,-1.,3.80002044322169));
#39703=CARTESIAN_POINT('Ctrl Pts',(1.38365244046226,-1.,3.80769156398429));
#39704=CARTESIAN_POINT('Ctrl Pts',(1.38337263902766,-1.,3.81537060817765));
#39705=CARTESIAN_POINT('Ctrl Pts',(1.38305421262724,-1.,3.82305771743715));
#39706=CARTESIAN_POINT('Ctrl Pts',(1.38269750245086,-1.,3.83075266982138));
#39707=CARTESIAN_POINT('Ctrl Pts',(1.38230274828774,-1.,3.83845502790609));
#39708=CARTESIAN_POINT('Ctrl Pts',(1.38187013346089,-1.,3.84616425605705));
#39709=CARTESIAN_POINT('Ctrl Pts',(1.38139983115075,-1.,3.85387983979557));
#39710=CARTESIAN_POINT('Ctrl Pts',(1.38089205993067,-1.,3.86160143044187));
#39711=CARTESIAN_POINT('Ctrl Pts',(1.38034709213129,-1.,3.86932885813403));
#39712=CARTESIAN_POINT('Ctrl Pts',(1.37976523097187,-1.,3.87706205830865));
#39713=CARTESIAN_POINT('Ctrl Pts',(1.37914679719446,-1.,3.88480102249461));
#39714=CARTESIAN_POINT('Ctrl Pts',(1.37849211287981,-1.,3.89254574338385));
#39715=CARTESIAN_POINT('Ctrl Pts',(1.3778014851263,-1.,3.90029615196255));
#39716=CARTESIAN_POINT('Ctrl Pts',(1.3770751963376,-1.,3.90805209522729));
#39717=CARTESIAN_POINT('Ctrl Pts',(1.37631350505516,-1.,3.91581337461825));
#39718=CARTESIAN_POINT('Ctrl Pts',(1.37551664448057,-1.,3.92357976987132));
#39719=CARTESIAN_POINT('Ctrl Pts',(1.37468482215784,-1.,3.93135106761941));
#39720=CARTESIAN_POINT('Ctrl Pts',(1.37381821967499,-1.,3.93912709041791));
#39721=CARTESIAN_POINT('Ctrl Pts',(1.37291699203423,-1.,3.94690771786926));
#39722=CARTESIAN_POINT('Ctrl Pts',(1.37198126433139,-1.,3.95469287283105));
#39723=CARTESIAN_POINT('Ctrl Pts',(1.37120515615663,-1.,3.96092458508407));
#39724=CARTESIAN_POINT('Ctrl Pts',(1.37060761746027,-1.,3.96560037975788));
#39725=CARTESIAN_POINT('Ctrl Pts',(1.37020239094758,-1.,3.9687184694173));
#39726=CARTESIAN_POINT('Ctrl Pts',(1.36999806084572,-1.,3.97027773754922));
#39727=CARTESIAN_POINT('',(1.22531898815164,-1.,4.01728681790024));
#39728=CARTESIAN_POINT('',(1.36999806084572,-1.,3.97027773754922));
#39729=CARTESIAN_POINT('',(0.963899035118985,-1.,3.62400312501199));
#39730=CARTESIAN_POINT('Ctrl Pts',(1.22531898815164,-1.,4.01728681790024));
#39731=CARTESIAN_POINT('Ctrl Pts',(1.22423716681317,-1.,4.01614544569895));
#39732=CARTESIAN_POINT('Ctrl Pts',(1.22207656455845,-1.,4.01386104433519));
#39733=CARTESIAN_POINT('Ctrl Pts',(1.21884478244403,-1.,4.01042947140789));
#39734=CARTESIAN_POINT('Ctrl Pts',(1.21455398918133,-1.,4.00584409522722));
#39735=CARTESIAN_POINT('Ctrl Pts',(1.20922097029551,-1.,4.00009577950721));
#39736=CARTESIAN_POINT('Ctrl Pts',(1.20391852375138,-1.,3.99433084799666));
#39737=CARTESIAN_POINT('Ctrl Pts',(1.19864679609566,-1.,3.98854928957189));
#39738=CARTESIAN_POINT('Ctrl Pts',(1.19340598349475,-1.,3.98275111052561));
#39739=CARTESIAN_POINT('Ctrl Pts',(1.18819633715539,-1.,3.97693634767754));
#39740=CARTESIAN_POINT('Ctrl Pts',(1.18301815039831,-1.,3.97110505165415));
#39741=CARTESIAN_POINT('Ctrl Pts',(1.17787174135592,-1.,3.96525726358159));
#39742=CARTESIAN_POINT('Ctrl Pts',(1.17275743590361,-1.,3.95939299213276));
#39743=CARTESIAN_POINT('Ctrl Pts',(1.16767555244438,-1.,3.95351219509876));
#39744=CARTESIAN_POINT('Ctrl Pts',(1.16262637999157,-1.,3.94761474780583));
#39745=CARTESIAN_POINT('Ctrl Pts',(1.15761018340956,-1.,3.94170046685203));
#39746=CARTESIAN_POINT('Ctrl Pts',(1.1526272271632,-1.,3.9357691705628));
#39747=CARTESIAN_POINT('Ctrl Pts',(1.14767779451123,-1.,3.92982073294257));
#39748=CARTESIAN_POINT('Ctrl Pts',(1.14276220561593,-1.,3.92385513133997));
#39749=CARTESIAN_POINT('Ctrl Pts',(1.13788084225554,-1.,3.91787251936827));
#39750=CARTESIAN_POINT('Ctrl Pts',(1.13303414693896,-1.,3.91187321145649));
#39751=CARTESIAN_POINT('Ctrl Pts',(1.12822258281553,-1.,3.90585753318737));
#39752=CARTESIAN_POINT('Ctrl Pts',(1.12344660099043,-1.,3.89982569750025));
#39753=CARTESIAN_POINT('Ctrl Pts',(1.11870660794603,-1.,3.89377768340344));
#39754=CARTESIAN_POINT('Ctrl Pts',(1.11400292434429,-1.,3.88771308285171));
#39755=CARTESIAN_POINT('Ctrl Pts',(1.10933577224008,-1.,3.88163105531724));
#39756=CARTESIAN_POINT('Ctrl Pts',(1.10470536603287,-1.,3.87553067187514));
#39757=CARTESIAN_POINT('Ctrl Pts',(1.10011198761195,-1.,3.86941120134849));
#39758=CARTESIAN_POINT('Ctrl Pts',(1.09555606505013,-1.,3.86327241021247));
#39759=CARTESIAN_POINT('Ctrl Pts',(1.09103825516294,-1.,3.85711487933931));
#39760=CARTESIAN_POINT('Ctrl Pts',(1.08655950846384,-1.,3.85094025222713));
#39761=CARTESIAN_POINT('Ctrl Pts',(1.08212087917991,-1.,3.8447504803063));
#39762=CARTESIAN_POINT('Ctrl Pts',(1.07772335353858,-1.,3.83854714117491));
#39763=CARTESIAN_POINT('Ctrl Pts',(1.07336766633459,-1.,3.83233071195144));
#39764=CARTESIAN_POINT('Ctrl Pts',(1.06905413180359,-1.,3.82609989967276));
#39765=CARTESIAN_POINT('Ctrl Pts',(1.0647824403893,-1.,3.81985083953012));
#39766=CARTESIAN_POINT('Ctrl Pts',(1.06055206187299,-1.,3.8135786611749));
#39767=CARTESIAN_POINT('Ctrl Pts',(1.05636266918644,-1.,3.80727913637791));
#39768=CARTESIAN_POINT('Ctrl Pts',(1.05221457990016,-1.,3.80095039790681));
#39769=CARTESIAN_POINT('Ctrl Pts',(1.04810913267639,-1.,3.79459440308786));
#39770=CARTESIAN_POINT('Ctrl Pts',(1.04404924374422,-1.,3.78821910787179));
#39771=CARTESIAN_POINT('Ctrl Pts',(1.04003862055798,-1.,3.7818353500817));
#39772=CARTESIAN_POINT('Ctrl Pts',(1.03608074678008,-1.,3.77545283140427));
#39773=CARTESIAN_POINT('Ctrl Pts',(1.03217786604919,-1.,3.76907609832516));
#39774=CARTESIAN_POINT('Ctrl Pts',(1.02833014458184,-1.,3.76270122291245));
#39775=CARTESIAN_POINT('Ctrl Pts',(1.02453429444668,-1.,3.75631037456224));
#39776=CARTESIAN_POINT('Ctrl Pts',(1.02078510487439,-1.,3.74987777155873));
#39777=CARTESIAN_POINT('Ctrl Pts',(1.01707794311088,-1.,3.74337942504993));
#39778=CARTESIAN_POINT('Ctrl Pts',(1.01341114319906,-1.,3.73680245055747));
#39779=CARTESIAN_POINT('Ctrl Pts',(1.00978798539491,-1.,3.73015276704407));
#39780=CARTESIAN_POINT('Ctrl Pts',(1.00622000735696,-1.,3.72346803750544));
#39781=CARTESIAN_POINT('Ctrl Pts',(1.00272423396802,-1.,3.71680667125047));
#39782=CARTESIAN_POINT('Ctrl Pts',(0.999317260756344,-1.,3.7102243971387));
#39783=CARTESIAN_POINT('Ctrl Pts',(0.996009819772431,-1.,3.70375282282107));
#39784=CARTESIAN_POINT('Ctrl Pts',(0.992802218332103,-1.,3.69738123415696));
#39785=CARTESIAN_POINT('Ctrl Pts',(0.989676715398858,-1.,3.69102682138955));
#39786=CARTESIAN_POINT('Ctrl Pts',(0.986602639864285,-1.,3.6845531792623));
#39787=CARTESIAN_POINT('Ctrl Pts',(0.983550791470864,-1.,3.67782408841876));
#39788=CARTESIAN_POINT('Ctrl Pts',(0.980505922458494,-1.,3.67074983340444));
#39789=CARTESIAN_POINT('Ctrl Pts',(0.977478312751416,-1.,3.66333049637403));
#39790=CARTESIAN_POINT('Ctrl Pts',(0.974519971354138,-1.,3.6557157673487));
#39791=CARTESIAN_POINT('Ctrl Pts',(0.971722122060277,-1.,3.64819756447072));
#39792=CARTESIAN_POINT('Ctrl Pts',(0.969195124674828,-1.,3.64113946505393));
#39793=CARTESIAN_POINT('Ctrl Pts',(0.967052554540877,-1.,3.6349212208096));
#39794=CARTESIAN_POINT('Ctrl Pts',(0.965395153165715,-1.,3.62988252139998));
#39795=CARTESIAN_POINT('Ctrl Pts',(0.964373850166081,-1.,3.62652618145252));
#39796=CARTESIAN_POINT('Ctrl Pts',(0.963957782642589,-1.,3.62489305727516));
#39797=CARTESIAN_POINT('Ctrl Pts',(0.963861297423578,-1.,3.62424461507455));
#39798=CARTESIAN_POINT('Ctrl Pts',(0.963880158556713,-1.,3.62404828878374));
#39799=CARTESIAN_POINT('Ctrl Pts',(0.963899035118985,-1.,3.62400312501199));
#39800=CARTESIAN_POINT('',(0.786422660833742,-1.,3.66661143271648));
#39801=CARTESIAN_POINT('Origin',(0.,-1.,0.));
#39802=CARTESIAN_POINT('',(0.732042837400619,-1.,4.13571194405636));
#39803=CARTESIAN_POINT('Ctrl Pts',(0.786422660833742,-1.,3.66661143271648));
#39804=CARTESIAN_POINT('Ctrl Pts',(0.786459983896781,-1.,3.66664310415236));
#39805=CARTESIAN_POINT('Ctrl Pts',(0.786565919559889,-1.,3.66680946938396));
#39806=CARTESIAN_POINT('Ctrl Pts',(0.786774337198499,-1.,3.66743103898844));
#39807=CARTESIAN_POINT('Ctrl Pts',(0.787145041181588,-1.,3.66907505398769));
#39808=CARTESIAN_POINT('Ctrl Pts',(0.787758799995426,-1.,3.672529236635));
#39809=CARTESIAN_POINT('Ctrl Pts',(0.788569566220662,-1.,3.67777119516438));
#39810=CARTESIAN_POINT('Ctrl Pts',(0.789483546065158,-1.,3.68428439784285));
#39811=CARTESIAN_POINT('Ctrl Pts',(0.790436284989579,-1.,3.69172044327754));
#39812=CARTESIAN_POINT('Ctrl Pts',(0.791356575696508,-1.,3.69968940808982));
#39813=CARTESIAN_POINT('Ctrl Pts',(0.792177688845967,-1.,3.70781724021879));
#39814=CARTESIAN_POINT('Ctrl Pts',(0.792848377370115,-1.,3.7158024239604));
#39815=CARTESIAN_POINT('Ctrl Pts',(0.79334702378387,-1.,3.7234879729357));
#39816=CARTESIAN_POINT('Ctrl Pts',(0.793682750269347,-1.,3.7308691469564));
#39817=CARTESIAN_POINT('Ctrl Pts',(0.79388270093679,-1.,3.73803280541576));
#39818=CARTESIAN_POINT('Ctrl Pts',(0.79398270045988,-1.,3.74511357728827));
#39819=CARTESIAN_POINT('Ctrl Pts',(0.79401734737144,-1.,3.75224692493895));
#39820=CARTESIAN_POINT('Ctrl Pts',(0.794008429135046,-1.,3.75951468666325));
#39821=CARTESIAN_POINT('Ctrl Pts',(0.793961083689141,-1.,3.76692626931184));
#39822=CARTESIAN_POINT('Ctrl Pts',(0.793870523787515,-1.,3.77444863801264));
#39823=CARTESIAN_POINT('Ctrl Pts',(0.793726235781339,-1.,3.78202460377617));
#39824=CARTESIAN_POINT('Ctrl Pts',(0.793516871680965,-1.,3.78959439439222));
#39825=CARTESIAN_POINT('Ctrl Pts',(0.7932356129732,-1.,3.79711921389862));
#39826=CARTESIAN_POINT('Ctrl Pts',(0.792882695234692,-1.,3.80459229925598));
#39827=CARTESIAN_POINT('Ctrl Pts',(0.792462483517568,-1.,3.81202588694726));
#39828=CARTESIAN_POINT('Ctrl Pts',(0.791981740718606,-1.,3.81944345442237));
#39829=CARTESIAN_POINT('Ctrl Pts',(0.791447528662381,-1.,3.82687033899799));
#39830=CARTESIAN_POINT('Ctrl Pts',(0.790865012705339,-1.,3.83432392054804));
#39831=CARTESIAN_POINT('Ctrl Pts',(0.790236124191289,-1.,3.84180762342476));
#39832=CARTESIAN_POINT('Ctrl Pts',(0.789560798155618,-1.,3.8493163780891));
#39833=CARTESIAN_POINT('Ctrl Pts',(0.788837734090688,-1.,3.85683995872536));
#39834=CARTESIAN_POINT('Ctrl Pts',(0.78806531509377,-1.,3.86436702561342));
#39835=CARTESIAN_POINT('Ctrl Pts',(0.78724252761798,-1.,3.87188916600905));
#39836=CARTESIAN_POINT('Ctrl Pts',(0.786369675812591,-1.,3.87940402818186));
#39837=CARTESIAN_POINT('Ctrl Pts',(0.785447890340723,-1.,3.88691313167399));
#39838=CARTESIAN_POINT('Ctrl Pts',(0.784478799358335,-1.,3.89442039235105));
#39839=CARTESIAN_POINT('Ctrl Pts',(0.783464141529082,-1.,3.90193039043971));
#39840=CARTESIAN_POINT('Ctrl Pts',(0.782405395622758,-1.,3.90944671004536));
#39841=CARTESIAN_POINT('Ctrl Pts',(0.781303428618343,-1.,3.9169703605466));
#39842=CARTESIAN_POINT('Ctrl Pts',(0.780158678615506,-1.,3.92450058323799));
#39843=CARTESIAN_POINT('Ctrl Pts',(0.778971308134786,-1.,3.93203552473153));
#39844=CARTESIAN_POINT('Ctrl Pts',(0.777741370568549,-1.,3.93957296768098));
#39845=CARTESIAN_POINT('Ctrl Pts',(0.776468966697959,-1.,3.94711101619471));
#39846=CARTESIAN_POINT('Ctrl Pts',(0.775154418039441,-1.,3.95464885452364));
#39847=CARTESIAN_POINT('Ctrl Pts',(0.773798212026682,-1.,3.96218649639876));
#39848=CARTESIAN_POINT('Ctrl Pts',(0.772400931772238,-1.,3.96972446532832));
#39849=CARTESIAN_POINT('Ctrl Pts',(0.770963190030503,-1.,3.97726349165507));
#39850=CARTESIAN_POINT('Ctrl Pts',(0.769485566245459,-1.,3.98480422348403));
#39851=CARTESIAN_POINT('Ctrl Pts',(0.767968531377707,-1.,3.99234687880892));
#39852=CARTESIAN_POINT('Ctrl Pts',(0.766412457135785,-1.,3.99989129179464));
#39853=CARTESIAN_POINT('Ctrl Pts',(0.764817648784946,-1.,4.00743706791366));
#39854=CARTESIAN_POINT('Ctrl Pts',(0.763184371182826,-1.,4.01498370680434));
#39855=CARTESIAN_POINT('Ctrl Pts',(0.761512875859941,-1.,4.02253072741347));
#39856=CARTESIAN_POINT('Ctrl Pts',(0.759803433244165,-1.,4.0300778195465));
#39857=CARTESIAN_POINT('Ctrl Pts',(0.758056338885553,-1.,4.03762485803468));
#39858=CARTESIAN_POINT('Ctrl Pts',(0.756271902370186,-1.,4.04517182654344));
#39859=CARTESIAN_POINT('Ctrl Pts',(0.754450441816411,-1.,4.05271876688106));
#39860=CARTESIAN_POINT('Ctrl Pts',(0.752592276482868,-1.,4.06026572221399));
#39861=CARTESIAN_POINT('Ctrl Pts',(0.750697720483175,-1.,4.06781267241886));
#39862=CARTESIAN_POINT('Ctrl Pts',(0.748767076679176,-1.,4.07535951055363));
#39863=CARTESIAN_POINT('Ctrl Pts',(0.746800631490821,-1.,4.08290608094789));
#39864=CARTESIAN_POINT('Ctrl Pts',(0.744798649705513,-1.,4.09045220253011));
#39865=CARTESIAN_POINT('Ctrl Pts',(0.742761369690017,-1.,4.09799769702712));
#39866=CARTESIAN_POINT('Ctrl Pts',(0.740688998555151,-1.,4.1055424175856));
#39867=CARTESIAN_POINT('Ctrl Pts',(0.738581708229118,-1.,4.11308626953795));
#39868=CARTESIAN_POINT('Ctrl Pts',(0.736439634335347,-1.,4.12062919626082));
#39869=CARTESIAN_POINT('Ctrl Pts',(0.734698226767512,-1.,4.12666277572794));
#39870=CARTESIAN_POINT('Ctrl Pts',(0.733376589325634,-1.,4.13118752796397));
#39871=CARTESIAN_POINT('Ctrl Pts',(0.732488575135925,-1.,4.13420383737278));
#39872=CARTESIAN_POINT('Ctrl Pts',(0.732042837400619,-1.,4.13571194405636));
#39873=CARTESIAN_POINT('',(0.581791163835814,-1.,4.15950947128175));
#39874=CARTESIAN_POINT('',(0.732042837400619,-1.,4.13571194405636));
#39875=CARTESIAN_POINT('',(0.385112848332549,-1.,3.73017266276632));
#39876=CARTESIAN_POINT('Ctrl Pts',(0.581791163835814,-1.,4.15950947128175));
#39877=CARTESIAN_POINT('Ctrl Pts',(0.580901211462913,-1.,4.15821291712391));
#39878=CARTESIAN_POINT('Ctrl Pts',(0.579124568912543,-1.,4.15561864787379));
#39879=CARTESIAN_POINT('Ctrl Pts',(0.576469391673916,-1.,4.1517237611974));
#39880=CARTESIAN_POINT('Ctrl Pts',(0.572948736066276,-1.,4.14652361065787));
#39881=CARTESIAN_POINT('Ctrl Pts',(0.568580610187115,-1.,4.14001179828669));
#39882=CARTESIAN_POINT('Ctrl Pts',(0.564245279535705,-1.,4.13348835726086));
#39883=CARTESIAN_POINT('Ctrl Pts',(0.559942890594628,-1.,4.12695329951859));
#39884=CARTESIAN_POINT('Ctrl Pts',(0.555673636130778,-1.,4.1204066619623));
#39885=CARTESIAN_POINT('Ctrl Pts',(0.551437758498246,-1.,4.11384852025578));
#39886=CARTESIAN_POINT('Ctrl Pts',(0.547235539486759,-1.,4.1072789702877));
#39887=CARTESIAN_POINT('Ctrl Pts',(0.543067286878457,-1.,4.10069810244473));
#39888=CARTESIAN_POINT('Ctrl Pts',(0.53893332117992,-1.,4.09410597627116));
#39889=CARTESIAN_POINT('Ctrl Pts',(0.534833963476999,-1.,4.08750259988693));
#39890=CARTESIAN_POINT('Ctrl Pts',(0.530769518728075,-1.,4.08088789536488));
#39891=CARTESIAN_POINT('Ctrl Pts',(0.526740277226999,-1.,4.07426172299496));
#39892=CARTESIAN_POINT('Ctrl Pts',(0.522746528602767,-1.,4.06762394471075));
#39893=CARTESIAN_POINT('Ctrl Pts',(0.518788572336809,-1.,4.06097448037934));
#39894=CARTESIAN_POINT('Ctrl Pts',(0.514866728193103,-1.,4.05431335771261));
#39895=CARTESIAN_POINT('Ctrl Pts',(0.510981349219173,-1.,4.04764078815591));
#39896=CARTESIAN_POINT('Ctrl Pts',(0.507132823288361,-1.,4.04095715149074));
#39897=CARTESIAN_POINT('Ctrl Pts',(0.503321556915513,-1.,4.0342628417439));
#39898=CARTESIAN_POINT('Ctrl Pts',(0.499547962340889,-1.,4.0275581398015));
#39899=CARTESIAN_POINT('Ctrl Pts',(0.495812444326222,-1.,4.02084308851813));
#39900=CARTESIAN_POINT('Ctrl Pts',(0.49211538341793,-1.,4.01411733503486));
#39901=CARTESIAN_POINT('Ctrl Pts',(0.48845713042453,-1.,4.0073800839092));
#39902=CARTESIAN_POINT('Ctrl Pts',(0.484838042421754,-1.,4.00063045119234));
#39903=CARTESIAN_POINT('Ctrl Pts',(0.481258512209637,-1.,3.99386775880655));
#39904=CARTESIAN_POINT('Ctrl Pts',(0.477718999122033,-1.,3.98709184306743));
#39905=CARTESIAN_POINT('Ctrl Pts',(0.474220061019542,-1.,3.9803033804443));
#39906=CARTESIAN_POINT('Ctrl Pts',(0.470762379613477,-1.,3.97350414289415));
#39907=CARTESIAN_POINT('Ctrl Pts',(0.467346690880671,-1.,3.96669622273946));
#39908=CARTESIAN_POINT('Ctrl Pts',(0.463973722115744,-1.,3.95988133243543));
#39909=CARTESIAN_POINT('Ctrl Pts',(0.460644124429119,-1.,3.95306005817363));
#39910=CARTESIAN_POINT('Ctrl Pts',(0.457358410451673,-1.,3.94623117206675));
#39911=CARTESIAN_POINT('Ctrl Pts',(0.454116879027575,-1.,3.93939080846298));
#39912=CARTESIAN_POINT('Ctrl Pts',(0.450919768356346,-1.,3.93253407403128));
#39913=CARTESIAN_POINT('Ctrl Pts',(0.447767416837296,-1.,3.92565674143424));
#39914=CARTESIAN_POINT('Ctrl Pts',(0.444660430230592,-1.,3.91875701610721));
#39915=CARTESIAN_POINT('Ctrl Pts',(0.441599824524047,-1.,3.91183704069146));
#39916=CARTESIAN_POINT('Ctrl Pts',(0.438587235458233,-1.,3.90490512938546));
#39917=CARTESIAN_POINT('Ctrl Pts',(0.435624629433505,-1.,3.8979725665544));
#39918=CARTESIAN_POINT('Ctrl Pts',(0.432713929544439,-1.,3.89104947940592));
#39919=CARTESIAN_POINT('Ctrl Pts',(0.429856640579733,-1.,3.88414070943334));
#39920=CARTESIAN_POINT('Ctrl Pts',(0.427053541173469,-1.,3.87724240306609));
#39921=CARTESIAN_POINT('Ctrl Pts',(0.424304173195142,-1.,3.87033643487882));
#39922=CARTESIAN_POINT('Ctrl Pts',(0.421607423177575,-1.,3.86339652542749));
#39923=CARTESIAN_POINT('Ctrl Pts',(0.418962468086809,-1.,3.85639825648031));
#39924=CARTESIAN_POINT('Ctrl Pts',(0.41636967805292,-1.,3.8493286415751));
#39925=CARTESIAN_POINT('Ctrl Pts',(0.413831367016726,-1.,3.84219403994742));
#39926=CARTESIAN_POINT('Ctrl Pts',(0.411353038798459,-1.,3.83503345578645));
#39927=CARTESIAN_POINT('Ctrl Pts',(0.408942371447376,-1.,3.82790724256397));
#39928=CARTESIAN_POINT('Ctrl Pts',(0.406607038258906,-1.,3.82087303913741));
#39929=CARTESIAN_POINT('Ctrl Pts',(0.404352694628236,-1.,3.81396374287762));
#39930=CARTESIAN_POINT('Ctrl Pts',(0.402181320148474,-1.,3.80716881962763));
#39931=CARTESIAN_POINT('Ctrl Pts',(0.400088346504726,-1.,3.80040370384659));
#39932=CARTESIAN_POINT('Ctrl Pts',(0.398064818684158,-1.,3.79352887163457));
#39933=CARTESIAN_POINT('Ctrl Pts',(0.396103205335028,-1.,3.78640521279479));
#39934=CARTESIAN_POINT('Ctrl Pts',(0.394202481011595,-1.,3.77894173114368));
#39935=CARTESIAN_POINT('Ctrl Pts',(0.392372786223346,-1.,3.77114011595892));
#39936=CARTESIAN_POINT('Ctrl Pts',(0.390642072979258,-1.,3.76315635032993));
#39937=CARTESIAN_POINT('Ctrl Pts',(0.38905477589825,-1.,3.75529302894757));
#39938=CARTESIAN_POINT('Ctrl Pts',(0.387663020050396,-1.,3.74792651696269));
#39939=CARTESIAN_POINT('Ctrl Pts',(0.386519576222035,-1.,3.74144965781088));
#39940=CARTESIAN_POINT('Ctrl Pts',(0.385670806454744,-1.,3.73621371845475));
#39941=CARTESIAN_POINT('Ctrl Pts',(0.385187124633964,-1.,3.73273893363318));
#39942=CARTESIAN_POINT('Ctrl Pts',(0.385031656499141,-1.,3.73106082862399));
#39943=CARTESIAN_POINT('Ctrl Pts',(0.385037797882046,-1.,3.73040527620929));
#39944=CARTESIAN_POINT('Ctrl Pts',(0.385087139001608,-1.,3.73021431755218));
#39945=CARTESIAN_POINT('Ctrl Pts',(0.385112848332549,-1.,3.73017266276632));
#39946=CARTESIAN_POINT('',(0.203156094897895,-1.,3.74449296982994));
#39947=CARTESIAN_POINT('Origin',(0.,-1.,0.));
#39948=CARTESIAN_POINT('',(0.0760622897878233,-1.,4.19931119685982));
#39949=CARTESIAN_POINT('Ctrl Pts',(0.203156094897895,-1.,3.74449296982994));
#39950=CARTESIAN_POINT('Ctrl Pts',(0.203188003947964,-1.,3.74453008995129));
#39951=CARTESIAN_POINT('Ctrl Pts',(0.203266610111263,-1.,3.74471097893961));
#39952=CARTESIAN_POINT('Ctrl Pts',(0.203375226874331,-1.,3.74535749969262));
#39953=CARTESIAN_POINT('Ctrl Pts',(0.203484186269314,-1.,3.74703926501843));
#39954=CARTESIAN_POINT('Ctrl Pts',(0.203550035479096,-1.,3.75054693397716));
#39955=CARTESIAN_POINT('Ctrl Pts',(0.203530796848403,-1.,3.75585118707924));
#39956=CARTESIAN_POINT('Ctrl Pts',(0.203414634707646,-1.,3.76242717937273));
#39957=CARTESIAN_POINT('Ctrl Pts',(0.203192390045337,-1.,3.76992071595267));
#39958=CARTESIAN_POINT('Ctrl Pts',(0.202854729699196,-1.,3.77793553476879));
#39959=CARTESIAN_POINT('Ctrl Pts',(0.202394260512192,-1.,3.78609175019317));
#39960=CARTESIAN_POINT('Ctrl Pts',(0.201807533800798,-1.,3.79408354187274));
#39961=CARTESIAN_POINT('Ctrl Pts',(0.201097756307251,-1.,3.80175247447171));
#39962=CARTESIAN_POINT('Ctrl Pts',(0.200274679433289,-1.,3.80909529318501));
#39963=CARTESIAN_POINT('Ctrl Pts',(0.199351525297396,-1.,3.81620203429702));
#39964=CARTESIAN_POINT('Ctrl Pts',(0.198342616900469,-1.,3.82321127348981));
#39965=CARTESIAN_POINT('Ctrl Pts',(0.197260935827375,-1.,3.83026221776488));
#39966=CARTESIAN_POINT('Ctrl Pts',(0.196115198971889,-1.,3.83743910616265));
#39967=CARTESIAN_POINT('Ctrl Pts',(0.194909009460254,-1.,3.84475203347052));
#39968=CARTESIAN_POINT('Ctrl Pts',(0.193642806777747,-1.,3.85216762264019));
#39969=CARTESIAN_POINT('Ctrl Pts',(0.192315153044979,-1.,3.85962774407652));
#39970=CARTESIAN_POINT('Ctrl Pts',(0.190924190418612,-1.,3.8670715862477));
#39971=CARTESIAN_POINT('Ctrl Pts',(0.189469253358254,-1.,3.87445976418377));
#39972=CARTESIAN_POINT('Ctrl Pts',(0.187951632512663,-1.,3.88178563496187));
#39973=CARTESIAN_POINT('Ctrl Pts',(0.186373724985263,-1.,3.88906196725817));
#39974=CARTESIAN_POINT('Ctrl Pts',(0.184738537728034,-1.,3.89631300742633));
#39975=CARTESIAN_POINT('Ctrl Pts',(0.183049081993193,-1.,3.90356488555138));
#39976=CARTESIAN_POINT('Ctrl Pts',(0.181307740731795,-1.,3.91083557557193));
#39977=CARTESIAN_POINT('Ctrl Pts',(0.179515885822894,-1.,3.91812876180948));
#39978=CARTESIAN_POINT('Ctrl Pts',(0.177674246152328,-1.,3.92543942697672));
#39979=CARTESIAN_POINT('Ctrl Pts',(0.175783136893872,-1.,3.93275726771049));
#39980=CARTESIAN_POINT('Ctrl Pts',(0.173842734974607,-1.,3.94007083096214));
#39981=CARTESIAN_POINT('Ctrl Pts',(0.171853355369232,-1.,3.94737164900861));
#39982=CARTESIAN_POINT('Ctrl Pts',(0.16981566637413,-1.,3.95465744665263));
#39983=CARTESIAN_POINT('Ctrl Pts',(0.167730547023312,-1.,3.96192990160296));
#39984=CARTESIAN_POINT('Ctrl Pts',(0.165598992851097,-1.,3.9691931362141));
#39985=CARTESIAN_POINT('Ctrl Pts',(0.163422004609998,-1.,3.97645194630944));
#39986=CARTESIAN_POINT('Ctrl Pts',(0.161200482186087,-1.,3.98371010319866));
#39987=CARTESIAN_POINT('Ctrl Pts',(0.158935123982796,-1.,3.99096873945862));
#39988=CARTESIAN_POINT('Ctrl Pts',(0.156626481393735,-1.,3.99822717425869));
#39989=CARTESIAN_POINT('Ctrl Pts',(0.154275004872309,-1.,4.00548360245297));
#39990=CARTESIAN_POINT('Ctrl Pts',(0.151881094022909,-1.,4.01273584234684));
#39991=CARTESIAN_POINT('Ctrl Pts',(0.149445144968707,-1.,4.01998203715588));
#39992=CARTESIAN_POINT('Ctrl Pts',(0.146967602878998,-1.,4.02722143147048));
#39993=CARTESIAN_POINT('Ctrl Pts',(0.144448947038352,-1.,4.03445411510403));
#39994=CARTESIAN_POINT('Ctrl Pts',(0.141889671485507,-1.,4.04168069633842));
#39995=CARTESIAN_POINT('Ctrl Pts',(0.139290267180059,-1.,4.04890199238056));
#39996=CARTESIAN_POINT('Ctrl Pts',(0.136651205046111,-1.,4.05611873400122));
#39997=CARTESIAN_POINT('Ctrl Pts',(0.133972916144225,-1.,4.06333121018476));
#39998=CARTESIAN_POINT('Ctrl Pts',(0.131255793548914,-1.,4.07053931528579));
#39999=CARTESIAN_POINT('Ctrl Pts',(0.128500200484813,-1.,4.07774270738809));
#40000=CARTESIAN_POINT('Ctrl Pts',(0.125706476822529,-1.,4.08494093372315));
#40001=CARTESIAN_POINT('Ctrl Pts',(0.122874946249119,-1.,4.09213355850836));
#40002=CARTESIAN_POINT('Ctrl Pts',(0.120005924388162,-1.,4.09932031767243));
#40003=CARTESIAN_POINT('Ctrl Pts',(0.117099722731704,-1.,4.10650113382187));
#40004=CARTESIAN_POINT('Ctrl Pts',(0.114156649609601,-1.,4.11367603925313));
#40005=CARTESIAN_POINT('Ctrl Pts',(0.111177012683377,-1.,4.12084512502444));
#40006=CARTESIAN_POINT('Ctrl Pts',(0.10816112052835,-1.,4.12800848371386));
#40007=CARTESIAN_POINT('Ctrl Pts',(0.105109286538864,-1.,4.13516614458396));
#40008=CARTESIAN_POINT('Ctrl Pts',(0.102021826577453,-1.,4.14231804938737));
#40009=CARTESIAN_POINT('Ctrl Pts',(0.0988990478899809,-1.,4.1494640891762));
#40010=CARTESIAN_POINT('Ctrl Pts',(0.0957412403297065,-1.,4.15660412653006));
#40011=CARTESIAN_POINT('Ctrl Pts',(0.0925486672167687,-1.,4.16373802265942));
#40012=CARTESIAN_POINT('Ctrl Pts',(0.0893215560850325,-1.,4.17086566491823));
#40013=CARTESIAN_POINT('Ctrl Pts',(0.0860600915552512,-1.,4.17798698669991));
#40014=CARTESIAN_POINT('Ctrl Pts',(0.0827644164389507,-1.,4.1851019532944));
#40015=CARTESIAN_POINT('Ctrl Pts',(0.08010058871176,-1.,4.19078883322483));
#40016=CARTESIAN_POINT('Ctrl Pts',(0.0780873956244399,-1.,4.19505112860624));
#40017=CARTESIAN_POINT('Ctrl Pts',(0.0767384596142192,-1.,4.19789138621624));
#40018=CARTESIAN_POINT('Ctrl Pts',(0.0760622897878233,-1.,4.19931119685982));
#40019=CARTESIAN_POINT('',(-0.0760622897878249,-1.,4.19931119685982));
#40020=CARTESIAN_POINT('',(0.0760622897878233,-1.,4.19931119685982));
#40021=CARTESIAN_POINT('',(-0.203156094896101,-1.,3.74449296983004));
#40022=CARTESIAN_POINT('Ctrl Pts',(-0.0760622897878249,-1.,4.19931119685982));
#40023=CARTESIAN_POINT('Ctrl Pts',(-0.0767384596141467,-1.,4.1978913862118));
#40024=CARTESIAN_POINT('Ctrl Pts',(-0.07808739562424,-1.,4.19505112859416));
#40025=CARTESIAN_POINT('Ctrl Pts',(-0.0801005887114322,-1.,4.19078883320504));
#40026=CARTESIAN_POINT('Ctrl Pts',(-0.0827644164385681,-1.,4.18510195327123));
#40027=CARTESIAN_POINT('Ctrl Pts',(-0.0860600915549399,-1.,4.17798698668094));
#40028=CARTESIAN_POINT('Ctrl Pts',(-0.0893215560848652,-1.,4.17086566490794));
#40029=CARTESIAN_POINT('Ctrl Pts',(-0.0925486672167534,-1.,4.16373802265839));
#40030=CARTESIAN_POINT('Ctrl Pts',(-0.0957412403298009,-1.,4.15660412653577));
#40031=CARTESIAN_POINT('Ctrl Pts',(-0.0988990478901228,-1.,4.14946408918485));
#40032=CARTESIAN_POINT('Ctrl Pts',(-0.102021826577584,-1.,4.14231804939538));
#40033=CARTESIAN_POINT('Ctrl Pts',(-0.105109286538945,-1.,4.13516614458895));
#40034=CARTESIAN_POINT('Ctrl Pts',(-0.10816112052837,-1.,4.12800848371504));
#40035=CARTESIAN_POINT('Ctrl Pts',(-0.111177012683347,-1.,4.1208451250225));
#40036=CARTESIAN_POINT('Ctrl Pts',(-0.114156649609546,-1.,4.11367603924961));
#40037=CARTESIAN_POINT('Ctrl Pts',(-0.117099722731648,-1.,4.10650113381833));
#40038=CARTESIAN_POINT('Ctrl Pts',(-0.120005924388124,-1.,4.09932031767002));
#40039=CARTESIAN_POINT('Ctrl Pts',(-0.122874946249107,-1.,4.09213355850756));
#40040=CARTESIAN_POINT('Ctrl Pts',(-0.12570647682254,-1.,4.08494093372377));
#40041=CARTESIAN_POINT('Ctrl Pts',(-0.128500200484838,-1.,4.07774270738954));
#40042=CARTESIAN_POINT('Ctrl Pts',(-0.131255793548941,-1.,4.0705393152874));
#40043=CARTESIAN_POINT('Ctrl Pts',(-0.133972916144245,-1.,4.06333121018596));
#40044=CARTESIAN_POINT('Ctrl Pts',(-0.136651205046119,-1.,4.05611873400172));
#40045=CARTESIAN_POINT('Ctrl Pts',(-0.139290267180057,-1.,4.04890199238036));
#40046=CARTESIAN_POINT('Ctrl Pts',(-0.1418896714855,-1.,4.04168069633781));
#40047=CARTESIAN_POINT('Ctrl Pts',(-0.144448947038345,-1.,4.03445411510333));
#40048=CARTESIAN_POINT('Ctrl Pts',(-0.146967602878994,-1.,4.02722143146994));
#40049=CARTESIAN_POINT('Ctrl Pts',(-0.149445144968707,-1.,4.01998203715564));
#40050=CARTESIAN_POINT('Ctrl Pts',(-0.151881094022911,-1.,4.01273584234689));
#40051=CARTESIAN_POINT('Ctrl Pts',(-0.154275004872311,-1.,4.00548360245319));
#40052=CARTESIAN_POINT('Ctrl Pts',(-0.156626481393734,-1.,3.99822717425893));
#40053=CARTESIAN_POINT('Ctrl Pts',(-0.158935123982793,-1.,3.99096873945878));
#40054=CARTESIAN_POINT('Ctrl Pts',(-0.161200482186085,-1.,3.98371010319872));
#40055=CARTESIAN_POINT('Ctrl Pts',(-0.163422004609999,-1.,3.97645194630943));
#40056=CARTESIAN_POINT('Ctrl Pts',(-0.165598992851102,-1.,3.96919313621407));
#40057=CARTESIAN_POINT('Ctrl Pts',(-0.16773054702332,-1.,3.96192990160296));
#40058=CARTESIAN_POINT('Ctrl Pts',(-0.169815666374139,-1.,3.95465744665268));
#40059=CARTESIAN_POINT('Ctrl Pts',(-0.17185335536924,-1.,3.94737164900868));
#40060=CARTESIAN_POINT('Ctrl Pts',(-0.17384273497461,-1.,3.94007083096217));
#40061=CARTESIAN_POINT('Ctrl Pts',(-0.175783136893868,-1.,3.93275726771042));
#40062=CARTESIAN_POINT('Ctrl Pts',(-0.177674246152318,-1.,3.92543942697655));
#40063=CARTESIAN_POINT('Ctrl Pts',(-0.179515885822882,-1.,3.91812876180926));
#40064=CARTESIAN_POINT('Ctrl Pts',(-0.181307740731786,-1.,3.91083557557175));
#40065=CARTESIAN_POINT('Ctrl Pts',(-0.183049081993191,-1.,3.90356488555132));
#40066=CARTESIAN_POINT('Ctrl Pts',(-0.184738537728043,-1.,3.89631300742646));
#40067=CARTESIAN_POINT('Ctrl Pts',(-0.186373724985281,-1.,3.88906196725848));
#40068=CARTESIAN_POINT('Ctrl Pts',(-0.187951632512685,-1.,3.88178563496228));
#40069=CARTESIAN_POINT('Ctrl Pts',(-0.189469253358273,-1.,3.87445976418412));
#40070=CARTESIAN_POINT('Ctrl Pts',(-0.19092419041862,-1.,3.86707158624783));
#40071=CARTESIAN_POINT('Ctrl Pts',(-0.192315153044971,-1.,3.85962774407633));
#40072=CARTESIAN_POINT('Ctrl Pts',(-0.193642806777723,-1.,3.85216762263966));
#40073=CARTESIAN_POINT('Ctrl Pts',(-0.194909009460221,-1.,3.84475203346977));
#40074=CARTESIAN_POINT('Ctrl Pts',(-0.196115198971859,-1.,3.83743910616195));
#40075=CARTESIAN_POINT('Ctrl Pts',(-0.197260935827362,-1.,3.83026221776456));
#40076=CARTESIAN_POINT('Ctrl Pts',(-0.198342616900487,-1.,3.82321127349016));
#40077=CARTESIAN_POINT('Ctrl Pts',(-0.199351525297447,-1.,3.81620203429815));
#40078=CARTESIAN_POINT('Ctrl Pts',(-0.200274679433365,-1.,3.80909529318669));
#40079=CARTESIAN_POINT('Ctrl Pts',(-0.201097756307326,-1.,3.80175247447337));
#40080=CARTESIAN_POINT('Ctrl Pts',(-0.201807533800837,-1.,3.7940835418736));
#40081=CARTESIAN_POINT('Ctrl Pts',(-0.20239426051216,-1.,3.78609175019242));
#40082=CARTESIAN_POINT('Ctrl Pts',(-0.202854729699081,-1.,3.77793553476614));
#40083=CARTESIAN_POINT('Ctrl Pts',(-0.203192390045165,-1.,3.7699207159487));
#40084=CARTESIAN_POINT('Ctrl Pts',(-0.203414634707479,-1.,3.76242717936885));
#40085=CARTESIAN_POINT('Ctrl Pts',(-0.203530796848322,-1.,3.75585118707734));
#40086=CARTESIAN_POINT('Ctrl Pts',(-0.203550035479166,-1.,3.75054693397875));
#40087=CARTESIAN_POINT('Ctrl Pts',(-0.203484186269415,-1.,3.74703926501752));
#40088=CARTESIAN_POINT('Ctrl Pts',(-0.203375226874122,-1.,3.74535749969115));
#40089=CARTESIAN_POINT('Ctrl Pts',(-0.203266610110531,-1.,3.74471097893845));
#40090=CARTESIAN_POINT('Ctrl Pts',(-0.203188003946657,-1.,3.74453008995092));
#40091=CARTESIAN_POINT('Ctrl Pts',(-0.203156094896101,-1.,3.74449296983004));
#40092=CARTESIAN_POINT('',(-0.385112848330762,-1.,3.73017266276651));
#40093=CARTESIAN_POINT('Origin',(0.,-1.,0.));
#40094=CARTESIAN_POINT('',(-0.581791163835815,-1.,4.15950947128175));
#40095=CARTESIAN_POINT('Ctrl Pts',(-0.385112848330762,-1.,3.73017266276651));
#40096=CARTESIAN_POINT('Ctrl Pts',(-0.385087139000375,-1.,3.73021431755274));
#40097=CARTESIAN_POINT('Ctrl Pts',(-0.385037797881504,-1.,3.73040527621055));
#40098=CARTESIAN_POINT('Ctrl Pts',(-0.385031656499164,-1.,3.73106082862548));
#40099=CARTESIAN_POINT('Ctrl Pts',(-0.385187124634206,-1.,3.73273893363406));
#40100=CARTESIAN_POINT('Ctrl Pts',(-0.385670806454566,-1.,3.73621371845318));
#40101=CARTESIAN_POINT('Ctrl Pts',(-0.386519576222251,-1.,3.74144965781276));
#40102=CARTESIAN_POINT('Ctrl Pts',(-0.387663020050836,-1.,3.74792651696654));
#40103=CARTESIAN_POINT('Ctrl Pts',(-0.389054775898702,-1.,3.75529302895152));
#40104=CARTESIAN_POINT('Ctrl Pts',(-0.39064207297956,-1.,3.76315635033257));
#40105=CARTESIAN_POINT('Ctrl Pts',(-0.392372786223433,-1.,3.77114011595967));
#40106=CARTESIAN_POINT('Ctrl Pts',(-0.394202481011499,-1.,3.77894173114283));
#40107=CARTESIAN_POINT('Ctrl Pts',(-0.396103205334841,-1.,3.78640521279313));
#40108=CARTESIAN_POINT('Ctrl Pts',(-0.39806481868397,-1.,3.7935288716329));
#40109=CARTESIAN_POINT('Ctrl Pts',(-0.4000883465046,-1.,3.80040370384546));
#40110=CARTESIAN_POINT('Ctrl Pts',(-0.402181320148436,-1.,3.80716881962728));
#40111=CARTESIAN_POINT('Ctrl Pts',(-0.404352694628273,-1.,3.81396374287793));
#40112=CARTESIAN_POINT('Ctrl Pts',(-0.406607038258985,-1.,3.8208730391381));
#40113=CARTESIAN_POINT('Ctrl Pts',(-0.40894237144746,-1.,3.82790724256471));
#40114=CARTESIAN_POINT('Ctrl Pts',(-0.411353038798519,-1.,3.83503345578698));
#40115=CARTESIAN_POINT('Ctrl Pts',(-0.413831367016748,-1.,3.84219403994762));
#40116=CARTESIAN_POINT('Ctrl Pts',(-0.416369678052907,-1.,3.84932864157497));
#40117=CARTESIAN_POINT('Ctrl Pts',(-0.418962468086773,-1.,3.85639825647996));
#40118=CARTESIAN_POINT('Ctrl Pts',(-0.421607423177534,-1.,3.86339652542709));
#40119=CARTESIAN_POINT('Ctrl Pts',(-0.424304173195111,-1.,3.87033643487851));
#40120=CARTESIAN_POINT('Ctrl Pts',(-0.427053541173457,-1.,3.87724240306597));
#40121=CARTESIAN_POINT('Ctrl Pts',(-0.429856640579741,-1.,3.88414070943341));
#40122=CARTESIAN_POINT('Ctrl Pts',(-0.432713929544458,-1.,3.89104947940611));
#40123=CARTESIAN_POINT('Ctrl Pts',(-0.435624629433528,-1.,3.89797256655462));
#40124=CARTESIAN_POINT('Ctrl Pts',(-0.43858723545825,-1.,3.90490512938563));
#40125=CARTESIAN_POINT('Ctrl Pts',(-0.441599824524054,-1.,3.91183704069153));
#40126=CARTESIAN_POINT('Ctrl Pts',(-0.444660430230591,-1.,3.91875701610719));
#40127=CARTESIAN_POINT('Ctrl Pts',(-0.447767416837293,-1.,3.92565674143416));
#40128=CARTESIAN_POINT('Ctrl Pts',(-0.450919768356348,-1.,3.93253407403123));
#40129=CARTESIAN_POINT('Ctrl Pts',(-0.454116879027584,-1.,3.93939080846298));
#40130=CARTESIAN_POINT('Ctrl Pts',(-0.457358410451683,-1.,3.94623117206678));
#40131=CARTESIAN_POINT('Ctrl Pts',(-0.460644124429121,-1.,3.95306005817364));
#40132=CARTESIAN_POINT('Ctrl Pts',(-0.463973722115733,-1.,3.95988133243538));
#40133=CARTESIAN_POINT('Ctrl Pts',(-0.467346690880643,-1.,3.9666962227393));
#40134=CARTESIAN_POINT('Ctrl Pts',(-0.470762379613439,-1.,3.97350414289392));
#40135=CARTESIAN_POINT('Ctrl Pts',(-0.47422006101951,-1.,3.98030338044409));
#40136=CARTESIAN_POINT('Ctrl Pts',(-0.477718999122027,-1.,3.98709184306738));
#40137=CARTESIAN_POINT('Ctrl Pts',(-0.481258512209675,-1.,3.99386775880679));
#40138=CARTESIAN_POINT('Ctrl Pts',(-0.484838042421835,-1.,4.00063045119288));
#40139=CARTESIAN_POINT('Ctrl Pts',(-0.488457130424633,-1.,4.0073800839099));
#40140=CARTESIAN_POINT('Ctrl Pts',(-0.492115383418018,-1.,4.01411733503546));
#40141=CARTESIAN_POINT('Ctrl Pts',(-0.495812444326251,-1.,4.02084308851832));
#40142=CARTESIAN_POINT('Ctrl Pts',(-0.499547962340821,-1.,4.02755813980101));
#40143=CARTESIAN_POINT('Ctrl Pts',(-0.503321556915346,-1.,4.03426284174272));
#40144=CARTESIAN_POINT('Ctrl Pts',(-0.507132823288136,-1.,4.04095715148915));
#40145=CARTESIAN_POINT('Ctrl Pts',(-0.51098134921897,-1.,4.04764078815447));
#40146=CARTESIAN_POINT('Ctrl Pts',(-0.514866728193017,-1.,4.05431335771199));
#40147=CARTESIAN_POINT('Ctrl Pts',(-0.518788572336924,-1.,4.06097448038013));
#40148=CARTESIAN_POINT('Ctrl Pts',(-0.522746528603107,-1.,4.06762394471314));
#40149=CARTESIAN_POINT('Ctrl Pts',(-0.526740277227498,-1.,4.07426172299847));
#40150=CARTESIAN_POINT('Ctrl Pts',(-0.530769518728571,-1.,4.08088789536836));
#40151=CARTESIAN_POINT('Ctrl Pts',(-0.534833963477273,-1.,4.08750259988885));
#40152=CARTESIAN_POINT('Ctrl Pts',(-0.538933321179756,-1.,4.09410597627));
#40153=CARTESIAN_POINT('Ctrl Pts',(-0.543067286877757,-1.,4.10069810243979));
#40154=CARTESIAN_POINT('Ctrl Pts',(-0.547235539485637,-1.,4.10727897027977));
#40155=CARTESIAN_POINT('Ctrl Pts',(-0.551437758497033,-1.,4.11384852024721));
#40156=CARTESIAN_POINT('Ctrl Pts',(-0.555673636129977,-1.,4.12040666195664));
#40157=CARTESIAN_POINT('Ctrl Pts',(-0.559942890594774,-1.,4.12695329951961));
#40158=CARTESIAN_POINT('Ctrl Pts',(-0.564245279537149,-1.,4.13348835727104));
#40159=CARTESIAN_POINT('Ctrl Pts',(-0.568580610189775,-1.,4.14001179830547));
#40160=CARTESIAN_POINT('Ctrl Pts',(-0.572948736069522,-1.,4.14652361068081));
#40161=CARTESIAN_POINT('Ctrl Pts',(-0.576469391676688,-1.,4.151723761217));
#40162=CARTESIAN_POINT('Ctrl Pts',(-0.579124568914235,-1.,4.15561864788576));
#40163=CARTESIAN_POINT('Ctrl Pts',(-0.580901211463535,-1.,4.1582129171283));
#40164=CARTESIAN_POINT('Ctrl Pts',(-0.581791163835815,-1.,4.15950947128175));
#40165=CARTESIAN_POINT('',(-0.73204283740062,-1.,4.13571194405636));
#40166=CARTESIAN_POINT('',(-0.581791163835815,-1.,4.15950947128175));
#40167=CARTESIAN_POINT('',(-0.786422660831985,-1.,3.66661143271685));
#40168=CARTESIAN_POINT('Ctrl Pts',(-0.73204283740062,-1.,4.13571194405636));
#40169=CARTESIAN_POINT('Ctrl Pts',(-0.73248857513516,-1.,4.1342038373684));
#40170=CARTESIAN_POINT('Ctrl Pts',(-0.733376589323546,-1.,4.13118752795207));
#40171=CARTESIAN_POINT('Ctrl Pts',(-0.734698226764092,-1.,4.12666277570844));
#40172=CARTESIAN_POINT('Ctrl Pts',(-0.736439634331345,-1.,4.120629196238));
#40173=CARTESIAN_POINT('Ctrl Pts',(-0.738581708225844,-1.,4.11308626951927));
#40174=CARTESIAN_POINT('Ctrl Pts',(-0.740688998553377,-1.,4.10554241757547));
#40175=CARTESIAN_POINT('Ctrl Pts',(-0.742761369689841,-1.,4.09799769702611));
#40176=CARTESIAN_POINT('Ctrl Pts',(-0.7447986497065,-1.,4.09045220253573));
#40177=CARTESIAN_POINT('Ctrl Pts',(-0.746800631492315,-1.,4.08290608095642));
#40178=CARTESIAN_POINT('Ctrl Pts',(-0.748767076680557,-1.,4.07535951056152));
#40179=CARTESIAN_POINT('Ctrl Pts',(-0.750697720484036,-1.,4.06781267242378));
#40180=CARTESIAN_POINT('Ctrl Pts',(-0.752592276483072,-1.,4.06026572221515));
#40181=CARTESIAN_POINT('Ctrl Pts',(-0.754450441816078,-1.,4.05271876687915));
#40182=CARTESIAN_POINT('Ctrl Pts',(-0.756271902369581,-1.,4.04517182653997));
#40183=CARTESIAN_POINT('Ctrl Pts',(-0.758056338884944,-1.,4.03762485803119));
#40184=CARTESIAN_POINT('Ctrl Pts',(-0.759803433243752,-1.,4.03007781954412));
#40185=CARTESIAN_POINT('Ctrl Pts',(-0.761512875859804,-1.,4.02253072741268));
#40186=CARTESIAN_POINT('Ctrl Pts',(-0.763184371182935,-1.,4.01498370680496));
#40187=CARTESIAN_POINT('Ctrl Pts',(-0.764817648785198,-1.,4.00743706791509));
#40188=CARTESIAN_POINT('Ctrl Pts',(-0.766412457136064,-1.,3.99989129179622));
#40189=CARTESIAN_POINT('Ctrl Pts',(-0.767968531377915,-1.,3.9923468788101));
#40190=CARTESIAN_POINT('Ctrl Pts',(-0.769485566245544,-1.,3.98480422348451));
#40191=CARTESIAN_POINT('Ctrl Pts',(-0.770963190030471,-1.,3.97726349165488));
#40192=CARTESIAN_POINT('Ctrl Pts',(-0.772400931772136,-1.,3.96972446532772));
#40193=CARTESIAN_POINT('Ctrl Pts',(-0.773798212026566,-1.,3.96218649639807));
#40194=CARTESIAN_POINT('Ctrl Pts',(-0.775154418039352,-1.,3.9546488545231));
#40195=CARTESIAN_POINT('Ctrl Pts',(-0.776468966697921,-1.,3.94711101619447));
#40196=CARTESIAN_POINT('Ctrl Pts',(-0.777741370568559,-1.,3.93957296768103));
#40197=CARTESIAN_POINT('Ctrl Pts',(-0.778971308134821,-1.,3.93203552473174));
#40198=CARTESIAN_POINT('Ctrl Pts',(-0.780158678615543,-1.,3.92450058323823));
#40199=CARTESIAN_POINT('Ctrl Pts',(-0.781303428618367,-1.,3.91697036054676));
#40200=CARTESIAN_POINT('Ctrl Pts',(-0.782405395622764,-1.,3.90944671004542));
#40201=CARTESIAN_POINT('Ctrl Pts',(-0.783464141529081,-1.,3.9019303904397));
#40202=CARTESIAN_POINT('Ctrl Pts',(-0.784478799358336,-1.,3.89442039235103));
#40203=CARTESIAN_POINT('Ctrl Pts',(-0.78544789034073,-1.,3.88691313167398));
#40204=CARTESIAN_POINT('Ctrl Pts',(-0.786369675812609,-1.,3.8794040281819));
#40205=CARTESIAN_POINT('Ctrl Pts',(-0.787242527617999,-1.,3.87188916600912));
#40206=CARTESIAN_POINT('Ctrl Pts',(-0.788065315093778,-1.,3.86436702561345));
#40207=CARTESIAN_POINT('Ctrl Pts',(-0.788837734090672,-1.,3.85683995872529));
#40208=CARTESIAN_POINT('Ctrl Pts',(-0.789560798155582,-1.,3.84931637808894));
#40209=CARTESIAN_POINT('Ctrl Pts',(-0.790236124191242,-1.,3.84180762342454));
#40210=CARTESIAN_POINT('Ctrl Pts',(-0.790865012705301,-1.,3.83432392054786));
#40211=CARTESIAN_POINT('Ctrl Pts',(-0.791447528662369,-1.,3.82687033899792));
#40212=CARTESIAN_POINT('Ctrl Pts',(-0.791981740718635,-1.,3.81944345442249));
#40213=CARTESIAN_POINT('Ctrl Pts',(-0.792462483517634,-1.,3.81202588694756));
#40214=CARTESIAN_POINT('Ctrl Pts',(-0.792882695234778,-1.,3.80459229925637));
#40215=CARTESIAN_POINT('Ctrl Pts',(-0.793235612973273,-1.,3.79711921389897));
#40216=CARTESIAN_POINT('Ctrl Pts',(-0.793516871680993,-1.,3.78959439439235));
#40217=CARTESIAN_POINT('Ctrl Pts',(-0.7937262357813,-1.,3.78202460377598));
#40218=CARTESIAN_POINT('Ctrl Pts',(-0.793870523787408,-1.,3.77444863801212));
#40219=CARTESIAN_POINT('Ctrl Pts',(-0.793961083688992,-1.,3.76692626931111));
#40220=CARTESIAN_POINT('Ctrl Pts',(-0.794008429134907,-1.,3.75951468666257));
#40221=CARTESIAN_POINT('Ctrl Pts',(-0.794017347371377,-1.,3.75224692493864));
#40222=CARTESIAN_POINT('Ctrl Pts',(-0.793982700459952,-1.,3.74511357728861));
#40223=CARTESIAN_POINT('Ctrl Pts',(-0.793882700937017,-1.,3.73803280541687));
#40224=CARTESIAN_POINT('Ctrl Pts',(-0.793682750269684,-1.,3.73086914695805));
#40225=CARTESIAN_POINT('Ctrl Pts',(-0.793347023784205,-1.,3.72348797293734));
#40226=CARTESIAN_POINT('Ctrl Pts',(-0.792848377370287,-1.,3.71580242396124));
#40227=CARTESIAN_POINT('Ctrl Pts',(-0.792177688845818,-1.,3.70781724021806));
#40228=CARTESIAN_POINT('Ctrl Pts',(-0.79135657569598,-1.,3.69968940808721));
#40229=CARTESIAN_POINT('Ctrl Pts',(-0.790436284988788,-1.,3.69172044327364));
#40230=CARTESIAN_POINT('Ctrl Pts',(-0.789483546064387,-1.,3.68428439783905));
#40231=CARTESIAN_POINT('Ctrl Pts',(-0.788569566220285,-1.,3.67777119516252));
#40232=CARTESIAN_POINT('Ctrl Pts',(-0.787758799995743,-1.,3.67252923663655));
#40233=CARTESIAN_POINT('Ctrl Pts',(-0.787145041181546,-1.,3.66907505398677));
#40234=CARTESIAN_POINT('Ctrl Pts',(-0.786774337198062,-1.,3.66743103898702));
#40235=CARTESIAN_POINT('Ctrl Pts',(-0.786565919558984,-1.,3.66680946938292));
#40236=CARTESIAN_POINT('Ctrl Pts',(-0.786459983895432,-1.,3.6666431041522));
#40237=CARTESIAN_POINT('Ctrl Pts',(-0.786422660831985,-1.,3.66661143271685));
#40238=CARTESIAN_POINT('',(-0.963899035117249,-1.,3.62400312501245));
#40239=CARTESIAN_POINT('Origin',(0.,-1.,0.));
#40240=CARTESIAN_POINT('',(-1.22531898815164,-1.,4.01728681790024));
#40241=CARTESIAN_POINT('Ctrl Pts',(-0.963899035117249,-1.,3.62400312501245));
#40242=CARTESIAN_POINT('Ctrl Pts',(-0.963880158555582,-1.,3.6240482887845));
#40243=CARTESIAN_POINT('Ctrl Pts',(-0.963861297423241,-1.,3.62424461507588));
#40244=CARTESIAN_POINT('Ctrl Pts',(-0.963957782642843,-1.,3.62489305727662));
#40245=CARTESIAN_POINT('Ctrl Pts',(-0.964373850166458,-1.,3.62652618145335));
#40246=CARTESIAN_POINT('Ctrl Pts',(-0.965395153165293,-1.,3.62988252139846));
#40247=CARTESIAN_POINT('Ctrl Pts',(-0.967052554541386,-1.,3.63492122081143));
#40248=CARTESIAN_POINT('Ctrl Pts',(-0.969195124675866,-1.,3.64113946505766));
#40249=CARTESIAN_POINT('Ctrl Pts',(-0.971722122061341,-1.,3.64819756447455));
#40250=CARTESIAN_POINT('Ctrl Pts',(-0.974519971354848,-1.,3.65571576735126));
#40251=CARTESIAN_POINT('Ctrl Pts',(-0.977478312751618,-1.,3.66333049637475));
#40252=CARTESIAN_POINT('Ctrl Pts',(-0.980505922458267,-1.,3.67074983340361));
#40253=CARTESIAN_POINT('Ctrl Pts',(-0.983550791470419,-1.,3.67782408841715));
#40254=CARTESIAN_POINT('Ctrl Pts',(-0.986602639863838,-1.,3.68455317926068));
#40255=CARTESIAN_POINT('Ctrl Pts',(-0.989676715398558,-1.,3.69102682138846));
#40256=CARTESIAN_POINT('Ctrl Pts',(-0.99280221833201,-1.,3.69738123415662));
#40257=CARTESIAN_POINT('Ctrl Pts',(-0.996009819772518,-1.,3.70375282282138));
#40258=CARTESIAN_POINT('Ctrl Pts',(-0.999317260756531,-1.,3.71022439713938));
#40259=CARTESIAN_POINT('Ctrl Pts',(-1.00272423396822,-1.,3.71680667125118));
#40260=CARTESIAN_POINT('Ctrl Pts',(-1.0062200073571,-1.,3.72346803750595));
#40261=CARTESIAN_POINT('Ctrl Pts',(-1.00978798539496,-1.,3.73015276704426));
#40262=CARTESIAN_POINT('Ctrl Pts',(-1.01341114319903,-1.,3.73680245055734));
#40263=CARTESIAN_POINT('Ctrl Pts',(-1.01707794311079,-1.,3.74337942504959));
#40264=CARTESIAN_POINT('Ctrl Pts',(-1.02078510487428,-1.,3.74987777155834));
#40265=CARTESIAN_POINT('Ctrl Pts',(-1.0245342944466,-1.,3.75631037456194));
#40266=CARTESIAN_POINT('Ctrl Pts',(-1.02833014458181,-1.,3.76270122291232));
#40267=CARTESIAN_POINT('Ctrl Pts',(-1.0321778660492,-1.,3.76907609832522));
#40268=CARTESIAN_POINT('Ctrl Pts',(-1.03608074678013,-1.,3.77545283140445));
#40269=CARTESIAN_POINT('Ctrl Pts',(-1.04003862055804,-1.,3.78183535008192));
#40270=CARTESIAN_POINT('Ctrl Pts',(-1.04404924374426,-1.,3.78821910787195));
#40271=CARTESIAN_POINT('Ctrl Pts',(-1.04810913267641,-1.,3.79459440308793));
#40272=CARTESIAN_POINT('Ctrl Pts',(-1.05221457990015,-1.,3.80095039790678));
#40273=CARTESIAN_POINT('Ctrl Pts',(-1.05636266918643,-1.,3.80727913637784));
#40274=CARTESIAN_POINT('Ctrl Pts',(-1.06055206187298,-1.,3.81357866117485));
#40275=CARTESIAN_POINT('Ctrl Pts',(-1.06478244038931,-1.,3.81985083953012));
#40276=CARTESIAN_POINT('Ctrl Pts',(-1.0690541318036,-1.,3.82609989967278));
#40277=CARTESIAN_POINT('Ctrl Pts',(-1.0733676663346,-1.,3.83233071195145));
#40278=CARTESIAN_POINT('Ctrl Pts',(-1.07772335353856,-1.,3.83854714117486));
#40279=CARTESIAN_POINT('Ctrl Pts',(-1.08212087917986,-1.,3.84475048030615));
#40280=CARTESIAN_POINT('Ctrl Pts',(-1.08655950846377,-1.,3.8509402522269));
#40281=CARTESIAN_POINT('Ctrl Pts',(-1.09103825516288,-1.,3.85711487933911));
#40282=CARTESIAN_POINT('Ctrl Pts',(-1.09555606505012,-1.,3.86327241021242));
#40283=CARTESIAN_POINT('Ctrl Pts',(-1.10011198761202,-1.,3.86941120134872));
#40284=CARTESIAN_POINT('Ctrl Pts',(-1.10470536603303,-1.,3.87553067187566));
#40285=CARTESIAN_POINT('Ctrl Pts',(-1.10933577224029,-1.,3.88163105531791));
#40286=CARTESIAN_POINT('Ctrl Pts',(-1.11400292434447,-1.,3.88771308285229));
#40287=CARTESIAN_POINT('Ctrl Pts',(-1.11870660794609,-1.,3.89377768340362));
#40288=CARTESIAN_POINT('Ctrl Pts',(-1.12344660099029,-1.,3.89982569749978));
#40289=CARTESIAN_POINT('Ctrl Pts',(-1.12822258281518,-1.,3.90585753318622));
#40290=CARTESIAN_POINT('Ctrl Pts',(-1.13303414693849,-1.,3.91187321145495));
#40291=CARTESIAN_POINT('Ctrl Pts',(-1.13788084225511,-1.,3.91787251936688));
#40292=CARTESIAN_POINT('Ctrl Pts',(-1.14276220561575,-1.,3.92385513133937));
#40293=CARTESIAN_POINT('Ctrl Pts',(-1.14767779451147,-1.,3.92982073294334));
#40294=CARTESIAN_POINT('Ctrl Pts',(-1.15262722716391,-1.,3.9357691705651));
#40295=CARTESIAN_POINT('Ctrl Pts',(-1.1576101834106,-1.,3.94170046685542));
#40296=CARTESIAN_POINT('Ctrl Pts',(-1.16262637999261,-1.,3.9476147478092));
#40297=CARTESIAN_POINT('Ctrl Pts',(-1.16767555244495,-1.,3.95351219510062));
#40298=CARTESIAN_POINT('Ctrl Pts',(-1.17275743590327,-1.,3.95939299213164));
#40299=CARTESIAN_POINT('Ctrl Pts',(-1.17787174135445,-1.,3.96525726357682));
#40300=CARTESIAN_POINT('Ctrl Pts',(-1.18301815039596,-1.,3.9711050516465));
#40301=CARTESIAN_POINT('Ctrl Pts',(-1.18819633715285,-1.,3.97693634766926));
#40302=CARTESIAN_POINT('Ctrl Pts',(-1.19340598349307,-1.,3.98275111052015));
#40303=CARTESIAN_POINT('Ctrl Pts',(-1.19864679609596,-1.,3.98854928957287));
#40304=CARTESIAN_POINT('Ctrl Pts',(-1.2039185237544,-1.,3.99433084800649));
#40305=CARTESIAN_POINT('Ctrl Pts',(-1.20922097030107,-1.,4.00009577952534));
#40306=CARTESIAN_POINT('Ctrl Pts',(-1.21455398918813,-1.,4.00584409524937));
#40307=CARTESIAN_POINT('Ctrl Pts',(-1.21884478244983,-1.,4.01042947142681));
#40308=CARTESIAN_POINT('Ctrl Pts',(-1.22207656456199,-1.,4.01386104434674));
#40309=CARTESIAN_POINT('Ctrl Pts',(-1.22423716681447,-1.,4.0161454457032));
#40310=CARTESIAN_POINT('Ctrl Pts',(-1.22531898815164,-1.,4.01728681790024));
#40311=CARTESIAN_POINT('',(-1.36999806084572,-1.,3.97027773754922));
#40312=CARTESIAN_POINT('',(-1.22531898815164,-1.,4.01728681790024));
#40313=CARTESIAN_POINT('',(-1.35032489087101,-1.,3.4984457533445));
#40314=CARTESIAN_POINT('Ctrl Pts',(-1.36999806084572,-1.,3.97027773754922));
#40315=CARTESIAN_POINT('Ctrl Pts',(-1.37020239094614,-1.,3.9687184694131));
#40316=CARTESIAN_POINT('Ctrl Pts',(-1.37060761745635,-1.,3.96560037974645));
#40317=CARTESIAN_POINT('Ctrl Pts',(-1.3712051561502,-1.,3.96092458506535));
#40318=CARTESIAN_POINT('Ctrl Pts',(-1.37198126432386,-1.,3.95469287280914));
#40319=CARTESIAN_POINT('Ctrl Pts',(-1.37291699202807,-1.,3.94690771785133));
#40320=CARTESIAN_POINT('Ctrl Pts',(-1.37381821967165,-1.,3.93912709040818));
#40321=CARTESIAN_POINT('Ctrl Pts',(-1.37468482215751,-1.,3.93135106761844));
#40322=CARTESIAN_POINT('Ctrl Pts',(-1.37551664448242,-1.,3.92357976987672));
#40323=CARTESIAN_POINT('Ctrl Pts',(-1.37631350505797,-1.,3.91581337462644));
#40324=CARTESIAN_POINT('Ctrl Pts',(-1.3770751963402,-1.,3.90805209523486));
#40325=CARTESIAN_POINT('Ctrl Pts',(-1.37780148512792,-1.,3.90029615196727));
#40326=CARTESIAN_POINT('Ctrl Pts',(-1.3784921128802,-1.,3.89254574338496));
#40327=CARTESIAN_POINT('Ctrl Pts',(-1.37914679719383,-1.,3.88480102249277));
#40328=CARTESIAN_POINT('Ctrl Pts',(-1.37976523097073,-1.,3.87706205830532));
#40329=CARTESIAN_POINT('Ctrl Pts',(-1.38034709213014,-1.,3.86932885813068));
#40330=CARTESIAN_POINT('Ctrl Pts',(-1.38089205992989,-1.,3.86160143043959));
#40331=CARTESIAN_POINT('Ctrl Pts',(-1.38139983115049,-1.,3.85387983979481));
#40332=CARTESIAN_POINT('Ctrl Pts',(-1.38187013346109,-1.,3.84616425605764));
#40333=CARTESIAN_POINT('Ctrl Pts',(-1.38230274828822,-1.,3.83845502790746));
#40334=CARTESIAN_POINT('Ctrl Pts',(-1.38269750245138,-1.,3.8307526698229));
#40335=CARTESIAN_POINT('Ctrl Pts',(-1.38305421262763,-1.,3.82305771743829));
#40336=CARTESIAN_POINT('Ctrl Pts',(-1.38337263902782,-1.,3.81537060817811));
#40337=CARTESIAN_POINT('Ctrl Pts',(-1.3836524404622,-1.,3.80769156398411));
#40338=CARTESIAN_POINT('Ctrl Pts',(-1.38389311766682,-1.,3.80002044322111));
#40339=CARTESIAN_POINT('Ctrl Pts',(-1.38409399694566,-1.,3.79235669640841));
#40340=CARTESIAN_POINT('Ctrl Pts',(-1.38425435883756,-1.,3.78469969805082));
#40341=CARTESIAN_POINT('Ctrl Pts',(-1.38437354551428,-1.,3.77704902230418));
#40342=CARTESIAN_POINT('Ctrl Pts',(-1.38445107339518,-1.,3.76940473185779));
#40343=CARTESIAN_POINT('Ctrl Pts',(-1.3844867525335,-1.,3.76176768271367));
#40344=CARTESIAN_POINT('Ctrl Pts',(-1.38448077997163,-1.,3.7541397631875));
#40345=CARTESIAN_POINT('Ctrl Pts',(-1.38443344984394,-1.,3.74652317167876));
#40346=CARTESIAN_POINT('Ctrl Pts',(-1.38434489156458,-1.,3.73891976418104));
#40347=CARTESIAN_POINT('Ctrl Pts',(-1.38421479111531,-1.,3.73133035859282));
#40348=CARTESIAN_POINT('Ctrl Pts',(-1.3840421342895,-1.,3.72375409358803));
#40349=CARTESIAN_POINT('Ctrl Pts',(-1.38382489984586,-1.,3.7161876605181));
#40350=CARTESIAN_POINT('Ctrl Pts',(-1.38356065402124,-1.,3.70862680753347));
#40351=CARTESIAN_POINT('Ctrl Pts',(-1.38324717612865,-1.,3.701067921679));
#40352=CARTESIAN_POINT('Ctrl Pts',(-1.38288311171651,-1.,3.69350967899526));
#40353=CARTESIAN_POINT('Ctrl Pts',(-1.38246852827182,-1.,3.68595444983837));
#40354=CARTESIAN_POINT('Ctrl Pts',(-1.3820057429062,-1.,3.67841038482414));
#40355=CARTESIAN_POINT('Ctrl Pts',(-1.38149812653868,-1.,3.67088843112262));
#40356=CARTESIAN_POINT('Ctrl Pts',(-1.38094856333552,-1.,3.66339848520857));
#40357=CARTESIAN_POINT('Ctrl Pts',(-1.38035791051213,-1.,3.6559455440439));
#40358=CARTESIAN_POINT('Ctrl Pts',(-1.37972372481603,-1.,3.64852652756456));
#40359=CARTESIAN_POINT('Ctrl Pts',(-1.37903818567359,-1.,3.64112507791141));
#40360=CARTESIAN_POINT('Ctrl Pts',(-1.37829035457339,-1.,3.63371727442486));
#40361=CARTESIAN_POINT('Ctrl Pts',(-1.37746987919881,-1.,3.62628098665145));
#40362=CARTESIAN_POINT('Ctrl Pts',(-1.37657053403107,-1.,3.6188048116042));
#40363=CARTESIAN_POINT('Ctrl Pts',(-1.37559314436634,-1.,3.61129546591064));
#40364=CARTESIAN_POINT('Ctrl Pts',(-1.37455051379623,-1.,3.60379020123988));
#40365=CARTESIAN_POINT('Ctrl Pts',(-1.37346320103157,-1.,3.59634627869048));
#40366=CARTESIAN_POINT('Ctrl Pts',(-1.37235053660976,-1.,3.58901853846365));
#40367=CARTESIAN_POINT('Ctrl Pts',(-1.37122241663062,-1.,3.58183885982715));
#40368=CARTESIAN_POINT('Ctrl Pts',(-1.37007229485659,-1.,3.57479875549486));
#40369=CARTESIAN_POINT('Ctrl Pts',(-1.36886584973389,-1.,3.5678208030466));
#40370=CARTESIAN_POINT('Ctrl Pts',(-1.36754771771233,-1.,3.56077662028649));
#40371=CARTESIAN_POINT('Ctrl Pts',(-1.3660614545677,-1.,3.55353883995949));
#40372=CARTESIAN_POINT('Ctrl Pts',(-1.36436666257598,-1.,3.54602591832973));
#40373=CARTESIAN_POINT('Ctrl Pts',(-1.36245507339307,-1.,3.53824396424961));
#40374=CARTESIAN_POINT('Ctrl Pts',(-1.36037259643734,-1.,3.530344649616));
#40375=CARTESIAN_POINT('Ctrl Pts',(-1.35821701528836,-1.,3.52261776116748));
#40376=CARTESIAN_POINT('Ctrl Pts',(-1.35611275237152,-1.,3.51542230699556));
#40377=CARTESIAN_POINT('Ctrl Pts',(-1.35419113575956,-1.,3.50913227059999));
#40378=CARTESIAN_POINT('Ctrl Pts',(-1.35257032843486,-1.,3.50408168106261));
#40379=CARTESIAN_POINT('Ctrl Pts',(-1.35142377279517,-1.,3.5007660381649));
#40380=CARTESIAN_POINT('Ctrl Pts',(-1.35080045218587,-1.,3.49920025459723));
#40381=CARTESIAN_POINT('Ctrl Pts',(-1.35049736560527,-1.,3.49861894124827));
#40382=CARTESIAN_POINT('Ctrl Pts',(-1.35036670892966,-1.,3.49847119623846));
#40383=CARTESIAN_POINT('Ctrl Pts',(-1.35032489087101,-1.,3.4984457533445));
#40384=CARTESIAN_POINT('',(-1.51895082866166,-1.,3.42859860294378));
#40385=CARTESIAN_POINT('Origin',(0.,-1.,0.));
#40386=CARTESIAN_POINT('',(-1.83867539237861,-1.,3.77614523045147));
#40387=CARTESIAN_POINT('Ctrl Pts',(-1.51895082866166,-1.,3.42859860294378));
#40388=CARTESIAN_POINT('Ctrl Pts',(-1.51893924967231,-1.,3.42864616361967));
#40389=CARTESIAN_POINT('Ctrl Pts',(-1.51895133295017,-1.,3.42884302333978));
#40390=CARTESIAN_POINT('Ctrl Pts',(-1.51914806898539,-1.,3.42946838852728));
#40391=CARTESIAN_POINT('Ctrl Pts',(-1.5198144909343,-1.,3.4310163189349));
#40392=CARTESIAN_POINT('Ctrl Pts',(-1.52134826724227,-1.,3.43417156977749));
#40393=CARTESIAN_POINT('Ctrl Pts',(-1.52377348950429,-1.,3.43888895974182));
#40394=CARTESIAN_POINT('Ctrl Pts',(-1.52686242875717,-1.,3.44469547527));
#40395=CARTESIAN_POINT('Ctrl Pts',(-1.530462444618,-1.,3.45127136828667));
#40396=CARTESIAN_POINT('Ctrl Pts',(-1.53440195378902,-1.,3.45825932955273));
#40397=CARTESIAN_POINT('Ctrl Pts',(-1.53851507915533,-1.,3.46531752207222));
#40398=CARTESIAN_POINT('Ctrl Pts',(-1.54266605398152,-1.,3.47217189224576));
#40399=CARTESIAN_POINT('Ctrl Pts',(-1.54678009290207,-1.,3.47868272898599));
#40400=CARTESIAN_POINT('Ctrl Pts',(-1.55084702970382,-1.,3.48485155928414));
#40401=CARTESIAN_POINT('Ctrl Pts',(-1.5548959590107,-1.,3.49076460877317));
#40402=CARTESIAN_POINT('Ctrl Pts',(-1.55897703097859,-1.,3.49655185179623));
#40403=CARTESIAN_POINT('Ctrl Pts',(-1.56314187758689,-1.,3.50234321621607));
#40404=CARTESIAN_POINT('Ctrl Pts',(-1.56742097575041,-1.,3.50821771695427));
#40405=CARTESIAN_POINT('Ctrl Pts',(-1.57181569799774,-1.,3.51418598431733));
#40406=CARTESIAN_POINT('Ctrl Pts',(-1.5763104998818,-1.,3.52021847865961));
#40407=CARTESIAN_POINT('Ctrl Pts',(-1.58088027227856,-1.,3.52626275334899));
#40408=CARTESIAN_POINT('Ctrl Pts',(-1.58549906268083,-1.,3.53226378147068));
#40409=CARTESIAN_POINT('Ctrl Pts',(-1.59014958368725,-1.,3.53818616861045));
#40410=CARTESIAN_POINT('Ctrl Pts',(-1.5948276694975,-1.,3.544024581823));
#40411=CARTESIAN_POINT('Ctrl Pts',(-1.59953698113444,-1.,3.54979148634426));
#40412=CARTESIAN_POINT('Ctrl Pts',(-1.60428584699848,-1.,3.55550985096117));
#40413=CARTESIAN_POINT('Ctrl Pts',(-1.60908344685459,-1.,3.56120432482986));
#40414=CARTESIAN_POINT('Ctrl Pts',(-1.61393581747522,-1.,3.56689200468404));
#40415=CARTESIAN_POINT('Ctrl Pts',(-1.61884340915412,-1.,3.57257679609826));
#40416=CARTESIAN_POINT('Ctrl Pts',(-1.62380329464851,-1.,3.57825455954405));
#40417=CARTESIAN_POINT('Ctrl Pts',(-1.62881051550748,-1.,3.5839162577435));
#40418=CARTESIAN_POINT('Ctrl Pts',(-1.63385971451259,-1.,3.58955176627876));
#40419=CARTESIAN_POINT('Ctrl Pts',(-1.63894676675349,-1.,3.59515368334887));
#40420=CARTESIAN_POINT('Ctrl Pts',(-1.6440700438558,-1.,3.6007202851384));
#40421=CARTESIAN_POINT('Ctrl Pts',(-1.64922952425833,-1.,3.60625346556992));
#40422=CARTESIAN_POINT('Ctrl Pts',(-1.65442619244327,-1.,3.61175734965129));
#40423=CARTESIAN_POINT('Ctrl Pts',(-1.65966133399186,-1.,3.61723666482457));
#40424=CARTESIAN_POINT('Ctrl Pts',(-1.66493585923853,-1.,3.62269517989104));
#40425=CARTESIAN_POINT('Ctrl Pts',(-1.67024966008037,-1.,3.62813422105257));
#40426=CARTESIAN_POINT('Ctrl Pts',(-1.67560193613145,-1.,3.63355343201211));
#40427=CARTESIAN_POINT('Ctrl Pts',(-1.68099146651577,-1.,3.63895140887443));
#40428=CARTESIAN_POINT('Ctrl Pts',(-1.68641690471455,-1.,3.64432638915199));
#40429=CARTESIAN_POINT('Ctrl Pts',(-1.691877054817,-1.,3.64967689827393));
#40430=CARTESIAN_POINT('Ctrl Pts',(-1.69737117722559,-1.,3.65500246526798));
#40431=CARTESIAN_POINT('Ctrl Pts',(-1.70289888566904,-1.,3.6603033877491));
#40432=CARTESIAN_POINT('Ctrl Pts',(-1.70846001610983,-1.,3.6655804319893));
#40433=CARTESIAN_POINT('Ctrl Pts',(-1.71405450210392,-1.,3.67083454901629));
#40434=CARTESIAN_POINT('Ctrl Pts',(-1.71968225581787,-1.,3.67606660374665));
#40435=CARTESIAN_POINT('Ctrl Pts',(-1.72534302437003,-1.,3.68127704936472));
#40436=CARTESIAN_POINT('Ctrl Pts',(-1.73103640956647,-1.,3.68646597019188));
#40437=CARTESIAN_POINT('Ctrl Pts',(-1.73676193254493,-1.,3.69163322647906));
#40438=CARTESIAN_POINT('Ctrl Pts',(-1.74251908492589,-1.,3.6967785691046));
#40439=CARTESIAN_POINT('Ctrl Pts',(-1.74830738046092,-1.,3.70190175673422));
#40440=CARTESIAN_POINT('Ctrl Pts',(-1.75412641804148,-1.,3.70700269736876));
#40441=CARTESIAN_POINT('Ctrl Pts',(-1.75997588499021,-1.,3.71208146346454));
#40442=CARTESIAN_POINT('Ctrl Pts',(-1.76585552124549,-1.,3.71713822377675));
#40443=CARTESIAN_POINT('Ctrl Pts',(-1.77176509401846,-1.,3.72217319911429));
#40444=CARTESIAN_POINT('Ctrl Pts',(-1.77770437039606,-1.,3.72718661205504));
#40445=CARTESIAN_POINT('Ctrl Pts',(-1.78367308442682,-1.,3.73217863095022));
#40446=CARTESIAN_POINT('Ctrl Pts',(-1.78967092823139,-1.,3.73714934729962));
#40447=CARTESIAN_POINT('Ctrl Pts',(-1.79569757859041,-1.,3.74209880351667));
#40448=CARTESIAN_POINT('Ctrl Pts',(-1.80175271485519,-1.,3.74702700874954));
#40449=CARTESIAN_POINT('Ctrl Pts',(-1.80783603939662,-1.,3.75193395888069));
#40450=CARTESIAN_POINT('Ctrl Pts',(-1.81394729834032,-1.,3.75681965683995));
#40451=CARTESIAN_POINT('Ctrl Pts',(-1.82008629694924,-1.,3.76168412709652));
#40452=CARTESIAN_POINT('Ctrl Pts',(-1.82625289221933,-1.,3.76652740355856));
#40453=CARTESIAN_POINT('Ctrl Pts',(-1.83120816956515,-1.,3.77038509819777));
#40454=CARTESIAN_POINT('Ctrl Pts',(-1.83493697935064,-1.,3.77326886065484));
#40455=CARTESIAN_POINT('Ctrl Pts',(-1.83742834010821,-1.,3.77518714458232));
#40456=CARTESIAN_POINT('Ctrl Pts',(-1.83867539237861,-1.,3.77614523045147));
#40457=CARTESIAN_POINT('',(-1.97421938526992,-1.,3.70708211654725));
#40458=CARTESIAN_POINT('',(-1.83867539237861,-1.,3.77614523045147));
#40459=CARTESIAN_POINT('',(-1.88097764062542,-1.,3.24413672884902));
#40460=CARTESIAN_POINT('Ctrl Pts',(-1.97421938526992,-1.,3.70708211654725));
#40461=CARTESIAN_POINT('Ctrl Pts',(-1.974177276451,-1.,3.7055100813194));
#40462=CARTESIAN_POINT('Ctrl Pts',(-1.97408973726149,-1.,3.70236698911837));
#40463=CARTESIAN_POINT('Ctrl Pts',(-1.97394846382289,-1.,3.69765528558292));
#40464=CARTESIAN_POINT('Ctrl Pts',(-1.97374016224397,-1.,3.69137888597855));
#40465=CARTESIAN_POINT('Ctrl Pts',(-1.97344650303631,-1.,3.68354319913416));
#40466=CARTESIAN_POINT('Ctrl Pts',(-1.97311947678035,-1.,3.67571738106175));
#40467=CARTESIAN_POINT('Ctrl Pts',(-1.9727589719863,-1.,3.66790152751984));
#40468=CARTESIAN_POINT('Ctrl Pts',(-1.97236485439317,-1.,3.66009578166865));
#40469=CARTESIAN_POINT('Ctrl Pts',(-1.97193697240645,-1.,3.65230034717364));
#40470=CARTESIAN_POINT('Ctrl Pts',(-1.97147515441539,-1.,3.64451546724221));
#40471=CARTESIAN_POINT('Ctrl Pts',(-1.97097920454698,-1.,3.63674139590853));
#40472=CARTESIAN_POINT('Ctrl Pts',(-1.97044889850518,-1.,3.62897836973397));
#40473=CARTESIAN_POINT('Ctrl Pts',(-1.96988398129888,-1.,3.62122658401722));
#40474=CARTESIAN_POINT('Ctrl Pts',(-1.96928416040712,-1.,3.61348615496393));
#40475=CARTESIAN_POINT('Ctrl Pts',(-1.96864911885775,-1.,3.60575714017676));
#40476=CARTESIAN_POINT('Ctrl Pts',(-1.96797854118257,-1.,3.59803959819725));
#40477=CARTESIAN_POINT('Ctrl Pts',(-1.96727213799507,-1.,3.5903336402273));
#40478=CARTESIAN_POINT('Ctrl Pts',(-1.9665296668894,-1.,3.58263947663884));
#40479=CARTESIAN_POINT('Ctrl Pts',(-1.96575096652857,-1.,3.57495748601088));
#40480=CARTESIAN_POINT('Ctrl Pts',(-1.96493594634643,-1.,3.56728820357933));
#40481=CARTESIAN_POINT('Ctrl Pts',(-1.96408450906868,-1.,3.55963218706201));
#40482=CARTESIAN_POINT('Ctrl Pts',(-1.96319648628667,-1.,3.55198990600929));
#40483=CARTESIAN_POINT('Ctrl Pts',(-1.96227157573058,-1.,3.54436163300425));
#40484=CARTESIAN_POINT('Ctrl Pts',(-1.96130926212661,-1.,3.53674730625759));
#40485=CARTESIAN_POINT('Ctrl Pts',(-1.96030879411534,-1.,3.52914648844289));
#40486=CARTESIAN_POINT('Ctrl Pts',(-1.95926936324436,-1.,3.52155867431438));
#40487=CARTESIAN_POINT('Ctrl Pts',(-1.95819025316768,-1.,3.51398354617772));
#40488=CARTESIAN_POINT('Ctrl Pts',(-1.95707099606514,-1.,3.50642124159913));
#40489=CARTESIAN_POINT('Ctrl Pts',(-1.9559115382367,-1.,3.49887263575602));
#40490=CARTESIAN_POINT('Ctrl Pts',(-1.95471236969653,-1.,3.49133956289154));
#40491=CARTESIAN_POINT('Ctrl Pts',(-1.95347412486316,-1.,3.48382414832648));
#40492=CARTESIAN_POINT('Ctrl Pts',(-1.95219722189878,-1.,3.47632820495926));
#40493=CARTESIAN_POINT('Ctrl Pts',(-1.95088147859876,-1.,3.4688525897419));
#40494=CARTESIAN_POINT('Ctrl Pts',(-1.94952575850196,-1.,3.46139661060959));
#40495=CARTESIAN_POINT('Ctrl Pts',(-1.94812754766524,-1.,3.45395731584051));
#40496=CARTESIAN_POINT('Ctrl Pts',(-1.94668377715332,-1.,3.44653088665685));
#40497=CARTESIAN_POINT('Ctrl Pts',(-1.94519168842883,-1.,3.43911410197693));
#40498=CARTESIAN_POINT('Ctrl Pts',(-1.94364973660285,-1.,3.43170586602436));
#40499=CARTESIAN_POINT('Ctrl Pts',(-1.94205835913692,-1.,3.42430850941497));
#40500=CARTESIAN_POINT('Ctrl Pts',(-1.94042111965237,-1.,3.41692971994082));
#40501=CARTESIAN_POINT('Ctrl Pts',(-1.93874306008132,-1.,3.40957978266622));
#40502=CARTESIAN_POINT('Ctrl Pts',(-1.93702857723089,-1.,3.40226802104093));
#40503=CARTESIAN_POINT('Ctrl Pts',(-1.93527929945982,-1.,3.39499923640789));
#40504=CARTESIAN_POINT('Ctrl Pts',(-1.93349233176794,-1.,3.38777076883267));
#40505=CARTESIAN_POINT('Ctrl Pts',(-1.93165739093292,-1.,3.38056768525577));
#40506=CARTESIAN_POINT('Ctrl Pts',(-1.92975993109897,-1.,3.37336807068078));
#40507=CARTESIAN_POINT('Ctrl Pts',(-1.92778626543803,-1.,3.36615168657597));
#40508=CARTESIAN_POINT('Ctrl Pts',(-1.92572846125763,-1.,3.35890824422976));
#40509=CARTESIAN_POINT('Ctrl Pts',(-1.92358838440518,-1.,3.35164424847206));
#40510=CARTESIAN_POINT('Ctrl Pts',(-1.92138450828378,-1.,3.34439448941915));
#40511=CARTESIAN_POINT('Ctrl Pts',(-1.91914609610173,-1.,3.33721230709948));
#40512=CARTESIAN_POINT('Ctrl Pts',(-1.91690081930297,-1.,3.33014884257812));
#40513=CARTESIAN_POINT('Ctrl Pts',(-1.91466343916612,-1.,3.32323403454507));
#40514=CARTESIAN_POINT('Ctrl Pts',(-1.91242616234459,-1.,3.31646052426395));
#40515=CARTESIAN_POINT('Ctrl Pts',(-1.91014297830502,-1.,3.30975721158694));
#40516=CARTESIAN_POINT('Ctrl Pts',(-1.90773912171424,-1.,3.30300595568341));
#40517=CARTESIAN_POINT('Ctrl Pts',(-1.9051389186417,-1.,3.29608978722258));
#40518=CARTESIAN_POINT('Ctrl Pts',(-1.9022897124757,-1.,3.28893448600364));
#40519=CARTESIAN_POINT('Ctrl Pts',(-1.89918429230425,-1.,3.28154737912287));
#40520=CARTESIAN_POINT('Ctrl Pts',(-1.89589172903662,-1.,3.27407108932908));
#40521=CARTESIAN_POINT('Ctrl Pts',(-1.89255393500769,-1.,3.2667765388833));
#40522=CARTESIAN_POINT('Ctrl Pts',(-1.88934996203508,-1.,3.2599988519361));
#40523=CARTESIAN_POINT('Ctrl Pts',(-1.88646802523372,-1.,3.25408686339298));
#40524=CARTESIAN_POINT('Ctrl Pts',(-1.88407708646435,-1.,3.24935200512055));
#40525=CARTESIAN_POINT('Ctrl Pts',(-1.88242596600422,-1.,3.24625654410705));
#40526=CARTESIAN_POINT('Ctrl Pts',(-1.88156537699118,-1.,3.24480754675942));
#40527=CARTESIAN_POINT('Ctrl Pts',(-1.88117508446657,-1.,3.24428080352952));
#40528=CARTESIAN_POINT('Ctrl Pts',(-1.88102292397987,-1.,3.2441553167131));
#40529=CARTESIAN_POINT('Ctrl Pts',(-1.88097764062542,-1.,3.24413672884902));
#40530=CARTESIAN_POINT('',(-2.03660101169564,-1.,3.14877060440425));
#40531=CARTESIAN_POINT('Origin',(0.,-1.,0.));
#40532=CARTESIAN_POINT('',(-2.40675750623143,-1.,3.44202241512147));
#40533=CARTESIAN_POINT('Ctrl Pts',(-2.03660101169564,-1.,3.14877060440425));
#40534=CARTESIAN_POINT('Ctrl Pts',(-2.03659701539175,-1.,3.1488193908823));
#40535=CARTESIAN_POINT('Ctrl Pts',(-2.03663974554941,-1.,3.14901193669147));
#40536=CARTESIAN_POINT('Ctrl Pts',(-2.03693188810614,-1.,3.14959882629936));
#40537=CARTESIAN_POINT('Ctrl Pts',(-2.03783225496023,-1.,3.15102344775396));
#40538=CARTESIAN_POINT('Ctrl Pts',(-2.03984073791432,-1.,3.1538999167466));
#40539=CARTESIAN_POINT('Ctrl Pts',(-2.04297406404132,-1.,3.15817983946525));
#40540=CARTESIAN_POINT('Ctrl Pts',(-2.0469333124766,-1.,3.16343165059235));
#40541=CARTESIAN_POINT('Ctrl Pts',(-2.05151770247452,-1.,3.16936341689859));
#40542=CARTESIAN_POINT('Ctrl Pts',(-2.05650186773279,-1.,3.17564906975592));
#40543=CARTESIAN_POINT('Ctrl Pts',(-2.06166849827143,-1.,3.18197692964677));
#40544=CARTESIAN_POINT('Ctrl Pts',(-2.06684062744065,-1.,3.18809755562297));
#40545=CARTESIAN_POINT('Ctrl Pts',(-2.07192253497765,-1.,3.19388465568113));
#40546=CARTESIAN_POINT('Ctrl Pts',(-2.0769044187063,-1.,3.19934132835879));
#40547=CARTESIAN_POINT('Ctrl Pts',(-2.08182850370816,-1.,3.20454818630635));
#40548=CARTESIAN_POINT('Ctrl Pts',(-2.08676465517435,-1.,3.20962575845433));
#40549=CARTESIAN_POINT('Ctrl Pts',(-2.0917841946046,-1.,3.2146942960168));
#40550=CARTESIAN_POINT('Ctrl Pts',(-2.09692958434933,-1.,3.21982707347067));
#40551=CARTESIAN_POINT('Ctrl Pts',(-2.10220384298533,-1.,3.22503437553496));
#40552=CARTESIAN_POINT('Ctrl Pts',(-2.1075869964248,-1.,3.23028945793334));
#40553=CARTESIAN_POINT('Ctrl Pts',(-2.11304604021784,-1.,3.23554444767115));
#40554=CARTESIAN_POINT('Ctrl Pts',(-2.11854673326972,-1.,3.24074905517282));
#40555=CARTESIAN_POINT('Ctrl Pts',(-2.12406646410943,-1.,3.24587102613347));
#40556=CARTESIAN_POINT('Ctrl Pts',(-2.1296002839681,-1.,3.25090574493994));
#40557=CARTESIAN_POINT('Ctrl Pts',(-2.13515375878786,-1.,3.25586495065027));
#40558=CARTESIAN_POINT('Ctrl Pts',(-2.14073870754257,-1.,3.26077002641868));
#40559=CARTESIAN_POINT('Ctrl Pts',(-2.14636805295663,-1.,3.26564388189764));
#40560=CARTESIAN_POINT('Ctrl Pts',(-2.15205043199818,-1.,3.27050245897244));
#40561=CARTESIAN_POINT('Ctrl Pts',(-2.15778690038359,-1.,3.27534954469206));
#40562=CARTESIAN_POINT('Ctrl Pts',(-2.16357391934434,-1.,3.28018150841414));
#40563=CARTESIAN_POINT('Ctrl Pts',(-2.16940517773459,-1.,3.2849901997973));
#40564=CARTESIAN_POINT('Ctrl Pts',(-2.17527380048422,-1.,3.28976645712566));
#40565=CARTESIAN_POINT('Ctrl Pts',(-2.18117455557062,-1.,3.29450361500484));
#40566=CARTESIAN_POINT('Ctrl Pts',(-2.18710556500325,-1.,3.29920022557635));
#40567=CARTESIAN_POINT('Ctrl Pts',(-2.19306710376112,-1.,3.30385816281831));
#40568=CARTESIAN_POINT('Ctrl Pts',(-2.19906078949924,-1.,3.30848134694596));
#40569=CARTESIAN_POINT('Ctrl Pts',(-2.20508863150608,-1.,3.3130742460895));
#40570=CARTESIAN_POINT('Ctrl Pts',(-2.21115211847872,-1.,3.31764044024231));
#40571=CARTESIAN_POINT('Ctrl Pts',(-2.21725135110889,-1.,3.32218125618955));
#40572=CARTESIAN_POINT('Ctrl Pts',(-2.22338548312758,-1.,3.32669646722871));
#40573=CARTESIAN_POINT('Ctrl Pts',(-2.22955308907221,-1.,3.33118487773593));
#40574=CARTESIAN_POINT('Ctrl Pts',(-2.2357525632881,-1.,3.33564495756478));
#40575=CARTESIAN_POINT('Ctrl Pts',(-2.24198249391437,-1.,3.34007543738044));
#40576=CARTESIAN_POINT('Ctrl Pts',(-2.24824207678288,-1.,3.34447596770768));
#40577=CARTESIAN_POINT('Ctrl Pts',(-2.25453097693524,-1.,3.34884690292342));
#40578=CARTESIAN_POINT('Ctrl Pts',(-2.26084915222484,-1.,3.35318902552676));
#40579=CARTESIAN_POINT('Ctrl Pts',(-2.26719668579921,-1.,3.35750328523077));
#40580=CARTESIAN_POINT('Ctrl Pts',(-2.27357362620902,-1.,3.36179055004369));
#40581=CARTESIAN_POINT('Ctrl Pts',(-2.27997979457968,-1.,3.36605130712978));
#40582=CARTESIAN_POINT('Ctrl Pts',(-2.28641481081045,-1.,3.37028570206357));
#40583=CARTESIAN_POINT('Ctrl Pts',(-2.2928781800731,-1.,3.37449367172707));
#40584=CARTESIAN_POINT('Ctrl Pts',(-2.29936936127588,-1.,3.37867504959382));
#40585=CARTESIAN_POINT('Ctrl Pts',(-2.30588783640389,-1.,3.38282967336676));
#40586=CARTESIAN_POINT('Ctrl Pts',(-2.31243319489505,-1.,3.38695751492659));
#40587=CARTESIAN_POINT('Ctrl Pts',(-2.31900513925627,-1.,3.39105869475112));
#40588=CARTESIAN_POINT('Ctrl Pts',(-2.32560343902683,-1.,3.39513342020045));
#40589=CARTESIAN_POINT('Ctrl Pts',(-2.33222789882601,-1.,3.39918194578115));
#40590=CARTESIAN_POINT('Ctrl Pts',(-2.33887832342715,-1.,3.40320452776646));
#40591=CARTESIAN_POINT('Ctrl Pts',(-2.34555447648901,-1.,3.40720137403888));
#40592=CARTESIAN_POINT('Ctrl Pts',(-2.35225606823649,-1.,3.41117262313464));
#40593=CARTESIAN_POINT('Ctrl Pts',(-2.35898278606449,-1.,3.4151183675076));
#40594=CARTESIAN_POINT('Ctrl Pts',(-2.36573431470314,-1.,3.41903866635384));
#40595=CARTESIAN_POINT('Ctrl Pts',(-2.37251035954351,-1.,3.42293356216595));
#40596=CARTESIAN_POINT('Ctrl Pts',(-2.37931067029517,-1.,3.42680309755241));
#40597=CARTESIAN_POINT('Ctrl Pts',(-2.38613505844641,-1.,3.43064732714472));
#40598=CARTESIAN_POINT('Ctrl Pts',(-2.39298338805823,-1.,3.43446630680436));
#40599=CARTESIAN_POINT('Ctrl Pts',(-2.39848113411429,-1.,3.43750133066036));
#40600=CARTESIAN_POINT('Ctrl Pts',(-2.40261515590099,-1.,3.43976627485223));
#40601=CARTESIAN_POINT('Ctrl Pts',(-2.40537592959345,-1.,3.44127120683402));
#40602=CARTESIAN_POINT('Ctrl Pts',(-2.40675750623143,-1.,3.44202241512147));
#40603=CARTESIAN_POINT('',(-2.52982887637028,-1.,3.35260583073571));
#40604=CARTESIAN_POINT('',(-2.40675750623143,-1.,3.44202241512147));
#40605=CARTESIAN_POINT('',(-2.36531447826073,-1.,2.90994629141676));
#40606=CARTESIAN_POINT('Ctrl Pts',(-2.52982887637028,-1.,3.35260583073571));
#40607=CARTESIAN_POINT('Ctrl Pts',(-2.5295413654909,-1.,3.35105973714071));
#40608=CARTESIAN_POINT('Ctrl Pts',(-2.52896321610703,-1.,3.34796903576663));
#40609=CARTESIAN_POINT('Ctrl Pts',(-2.52808660915689,-1.,3.34333744115511));
#40610=CARTESIAN_POINT('Ctrl Pts',(-2.52689902690158,-1.,3.33717089999103));
#40611=CARTESIAN_POINT('Ctrl Pts',(-2.52538321164634,-1.,3.32947762187533));
#40612=CARTESIAN_POINT('Ctrl Pts',(-2.5238359839626,-1.,3.32179931078699));
#40613=CARTESIAN_POINT('Ctrl Pts',(-2.52225724871313,-1.,3.31413607874645));
#40614=CARTESIAN_POINT('Ctrl Pts',(-2.52064689568511,-1.,3.30648808815442));
#40615=CARTESIAN_POINT('Ctrl Pts',(-2.51900480701069,-1.,3.29885556388352));
#40616=CARTESIAN_POINT('Ctrl Pts',(-2.51733085123797,-1.,3.2912387729927));
#40617=CARTESIAN_POINT('Ctrl Pts',(-2.51562487464514,-1.,3.28363799702982));
#40618=CARTESIAN_POINT('Ctrl Pts',(-2.513886692704,-1.,3.27605350473142));
#40619=CARTESIAN_POINT('Ctrl Pts',(-2.51211608411423,-1.,3.26848552888115));
#40620=CARTESIAN_POINT('Ctrl Pts',(-2.51031277813486,-1.,3.26093423001434));
#40621=CARTESIAN_POINT('Ctrl Pts',(-2.50847647070723,-1.,3.25339971460982));
#40622=CARTESIAN_POINT('Ctrl Pts',(-2.506606859405,-1.,3.24588208983849));
#40623=CARTESIAN_POINT('Ctrl Pts',(-2.5047036758003,-1.,3.23838151080319));
#40624=CARTESIAN_POINT('Ctrl Pts',(-2.50276671338111,-1.,3.23089822320646));
#40625=CARTESIAN_POINT('Ctrl Pts',(-2.50079587201957,-1.,3.22343262620503));
#40626=CARTESIAN_POINT('Ctrl Pts',(-2.4987911459939,-1.,3.21598526261286));
#40627=CARTESIAN_POINT('Ctrl Pts',(-2.4967525264737,-1.,3.20855669849836));
#40628=CARTESIAN_POINT('Ctrl Pts',(-2.49467992057755,-1.,3.20114742397588));
#40629=CARTESIAN_POINT('Ctrl Pts',(-2.49257307239848,-1.,3.19375775555798));
#40630=CARTESIAN_POINT('Ctrl Pts',(-2.49043146334059,-1.,3.18638771282266));
#40631=CARTESIAN_POINT('Ctrl Pts',(-2.48825428288201,-1.,3.17903698136622));
#40632=CARTESIAN_POINT('Ctrl Pts',(-2.48604065348587,-1.,3.17170518863313));
#40633=CARTESIAN_POINT('Ctrl Pts',(-2.48378981792725,-1.,3.16439213290161));
#40634=CARTESIAN_POINT('Ctrl Pts',(-2.48150133566571,-1.,3.15709802322739));
#40635=CARTESIAN_POINT('Ctrl Pts',(-2.47917529057029,-1.,3.14982373241352));
#40636=CARTESIAN_POINT('Ctrl Pts',(-2.47681245356109,-1.,3.1425709954655));
#40637=CARTESIAN_POINT('Ctrl Pts',(-2.47441378371932,-1.,3.13534181229295));
#40638=CARTESIAN_POINT('Ctrl Pts',(-2.47197997765871,-1.,3.12813790805952));
#40639=CARTESIAN_POINT('Ctrl Pts',(-2.46951098947469,-1.,3.12096015766983));
#40640=CARTESIAN_POINT('Ctrl Pts',(-2.46700558843506,-1.,3.11380805536122));
#40641=CARTESIAN_POINT('Ctrl Pts',(-2.46446082979646,-1.,3.1066790790198));
#40642=CARTESIAN_POINT('Ctrl Pts',(-2.46187308501884,-1.,3.09956993697052));
#40643=CARTESIAN_POINT('Ctrl Pts',(-2.4592391256388,-1.,3.09247787931887));
#40644=CARTESIAN_POINT('Ctrl Pts',(-2.45655725437039,-1.,3.08540206545315));
#40645=CARTESIAN_POINT('Ctrl Pts',(-2.4538282678779,-1.,3.07834472886139));
#40646=CARTESIAN_POINT('Ctrl Pts',(-2.45105688854422,-1.,3.07131290521297));
#40647=CARTESIAN_POINT('Ctrl Pts',(-2.44824970516544,-1.,3.06431596421405));
#40648=CARTESIAN_POINT('Ctrl Pts',(-2.44541251892556,-1.,3.05736242671506));
#40649=CARTESIAN_POINT('Ctrl Pts',(-2.44254768923105,-1.,3.05045678021504));
#40650=CARTESIAN_POINT('Ctrl Pts',(-2.43965194061857,-1.,3.04359685040555));
#40651=CARTESIAN_POINT('Ctrl Pts',(-2.43671278042414,-1.,3.03676949672821));
#40652=CARTESIAN_POINT('Ctrl Pts',(-2.43371241361488,-1.,3.02995534946978));
#40653=CARTESIAN_POINT('Ctrl Pts',(-2.43063415586637,-1.,3.02313656036004));
#40654=CARTESIAN_POINT('Ctrl Pts',(-2.42746856264168,-1.,3.01630420830504));
#40655=CARTESIAN_POINT('Ctrl Pts',(-2.42421849439613,-1.,3.00946442616658));
#40656=CARTESIAN_POINT('Ctrl Pts',(-2.42090763946779,-1.,3.00264868585996));
#40657=CARTESIAN_POINT('Ctrl Pts',(-2.41757324500514,-1.,2.99590509293503));
#40658=CARTESIAN_POINT('Ctrl Pts',(-2.41425064199586,-1.,2.98927983005796));
#40659=CARTESIAN_POINT('Ctrl Pts',(-2.41095909342571,-1.,2.98280015815107));
#40660=CARTESIAN_POINT('Ctrl Pts',(-2.40768975073713,-1.,2.97646002822422));
#40661=CARTESIAN_POINT('Ctrl Pts',(-2.40438604734919,-1.,2.9701964131236));
#40662=CARTESIAN_POINT('Ctrl Pts',(-2.4009556571164,-1.,2.96390432240312));
#40663=CARTESIAN_POINT('Ctrl Pts',(-2.39730553974517,-1.,2.95748006482942));
#40664=CARTESIAN_POINT('Ctrl Pts',(-2.39337207631667,-1.,2.95085857128439));
#40665=CARTESIAN_POINT('Ctrl Pts',(-2.38914929090759,-1.,2.94404820669076));
#40666=CARTESIAN_POINT('Ctrl Pts',(-2.38472771516311,-1.,2.93717903280391));
#40667=CARTESIAN_POINT('Ctrl Pts',(-2.38028989582073,-1.,2.93049643640206));
#40668=CARTESIAN_POINT('Ctrl Pts',(-2.3760651052403,-1.,2.92430340582608));
#40669=CARTESIAN_POINT('Ctrl Pts',(-2.37229381109821,-1.,2.91891503791411));
#40670=CARTESIAN_POINT('Ctrl Pts',(-2.36919161373173,-1.,2.9146124988314));
#40671=CARTESIAN_POINT('Ctrl Pts',(-2.36707658451664,-1.,2.91181344022549));
#40672=CARTESIAN_POINT('Ctrl Pts',(-2.36599991765749,-1.,2.91051690822156));
#40673=CARTESIAN_POINT('Ctrl Pts',(-2.36553202948613,-1.,2.91005770527719));
#40674=CARTESIAN_POINT('Ctrl Pts',(-2.36536211188453,-1.,2.90995756655606));
#40675=CARTESIAN_POINT('Ctrl Pts',(-2.36531447826074,-1.,2.90994629141676));
#40676=CARTESIAN_POINT('',(-2.50410331873042,-1.,2.79140942341378));
#40677=CARTESIAN_POINT('Origin',(0.,-1.,0.));
#40678=CARTESIAN_POINT('',(-2.91557726271063,-1.,3.02314558451372));
#40679=CARTESIAN_POINT('Ctrl Pts',(-2.50410331873042,-1.,2.79140942341378));
#40680=CARTESIAN_POINT('Ctrl Pts',(-2.50410700351426,-1.,2.79145823440899));
#40681=CARTESIAN_POINT('Ctrl Pts',(-2.50417932839343,-1.,2.79164172519039));
#40682=CARTESIAN_POINT('Ctrl Pts',(-2.50455968395235,-1.,2.79217568804874));
#40683=CARTESIAN_POINT('Ctrl Pts',(-2.50567182569153,-1.,2.79344192164204));
#40684=CARTESIAN_POINT('Ctrl Pts',(-2.50810555977564,-1.,2.7959687805717));
#40685=CARTESIAN_POINT('Ctrl Pts',(-2.51186983687947,-1.,2.79970585014308));
#40686=CARTESIAN_POINT('Ctrl Pts',(-2.51660190466067,-1.,2.80427363984939));
#40687=CARTESIAN_POINT('Ctrl Pts',(-2.52205778589922,-1.,2.80941521967234));
#40688=CARTESIAN_POINT('Ctrl Pts',(-2.52796388055457,-1.,2.8148437904867));
#40689=CARTESIAN_POINT('Ctrl Pts',(-2.53405679667463,-1.,2.82028550483744));
#40690=CARTESIAN_POINT('Ctrl Pts',(-2.54012272520141,-1.,2.82552167649157));
#40691=CARTESIAN_POINT('Ctrl Pts',(-2.54604736792542,-1.,2.83044254225794));
#40692=CARTESIAN_POINT('Ctrl Pts',(-2.55182152806964,-1.,2.83505269592412));
#40693=CARTESIAN_POINT('Ctrl Pts',(-2.55749952145165,-1.,2.83942515220699));
#40694=CARTESIAN_POINT('Ctrl Pts',(-2.56316920798489,-1.,2.84366802680211));
#40695=CARTESIAN_POINT('Ctrl Pts',(-2.56891984251743,-1.,2.84788893329091));
#40696=CARTESIAN_POINT('Ctrl Pts',(-2.57480482727128,-1.,2.85215360144483));
#40697=CARTESIAN_POINT('Ctrl Pts',(-2.58082875254407,-1.,2.85647171715147));
#40698=CARTESIAN_POINT('Ctrl Pts',(-2.5869677064356,-1.,2.86081999003668));
#40699=CARTESIAN_POINT('Ctrl Pts',(-2.59318160184921,-1.,2.86515629953528));
#40700=CARTESIAN_POINT('Ctrl Pts',(-2.59942875223202,-1.,2.86943633170712));
#40701=CARTESIAN_POINT('Ctrl Pts',(-2.6056817788128,-1.,2.87363176656475));
#40702=CARTESIAN_POINT('Ctrl Pts',(-2.61193507170928,-1.,2.87773881947885));
#40703=CARTESIAN_POINT('Ctrl Pts',(-2.61819596473087,-1.,2.88176821427502));
#40704=CARTESIAN_POINT('Ctrl Pts',(-2.62447947640253,-1.,2.88573922195049));
#40705=CARTESIAN_POINT('Ctrl Pts',(-2.63080195420771,-1.,2.88967244854243));
#40706=CARTESIAN_POINT('Ctrl Pts',(-2.63717442263944,-1.,2.89358228854557));
#40707=CARTESIAN_POINT('Ctrl Pts',(-2.64359851684146,-1.,2.89747231723361));
#40708=CARTESIAN_POINT('Ctrl Pts',(-2.65007017365576,-1.,2.90133950224879));
#40709=CARTESIAN_POINT('Ctrl Pts',(-2.65658188464287,-1.,2.90517678087467));
#40710=CARTESIAN_POINT('Ctrl Pts',(-2.66312542616809,-1.,2.90897617968921));
#40711=CARTESIAN_POINT('Ctrl Pts',(-2.66969458792627,-1.,2.91273193382876));
#40712=CARTESIAN_POINT('Ctrl Pts',(-2.67628728855309,-1.,2.91644290704281));
#40713=CARTESIAN_POINT('Ctrl Pts',(-2.68290409279689,-1.,2.92011090722152));
#40714=CARTESIAN_POINT('Ctrl Pts',(-2.68954721165342,-1.,2.92373955325876));
#40715=CARTESIAN_POINT('Ctrl Pts',(-2.69621932864302,-1.,2.92733294395268));
#40716=CARTESIAN_POINT('Ctrl Pts',(-2.70292247416881,-1.,2.93089438233746));
#40717=CARTESIAN_POINT('Ctrl Pts',(-2.70965695523776,-1.,2.93442516311168));
#40718=CARTESIAN_POINT('Ctrl Pts',(-2.71642190053575,-1.,2.93792519474955));
#40719=CARTESIAN_POINT('Ctrl Pts',(-2.72321571511322,-1.,2.94139351933882));
#40720=CARTESIAN_POINT('Ctrl Pts',(-2.73003657371613,-1.,2.94482887675139));
#40721=CARTESIAN_POINT('Ctrl Pts',(-2.73688288329825,-1.,2.94823023414381));
#40722=CARTESIAN_POINT('Ctrl Pts',(-2.7437537949221,-1.,2.95159737214305));
#40723=CARTESIAN_POINT('Ctrl Pts',(-2.75064903318996,-1.,2.95493069316211));
#40724=CARTESIAN_POINT('Ctrl Pts',(-2.75756867888393,-1.,2.9582309766594));
#40725=CARTESIAN_POINT('Ctrl Pts',(-2.76451296269571,-1.,2.96149914764832));
#40726=CARTESIAN_POINT('Ctrl Pts',(-2.77148206836464,-1.,2.96473605585548));
#40727=CARTESIAN_POINT('Ctrl Pts',(-2.77847589542767,-1.,2.9679422104295));
#40728=CARTESIAN_POINT('Ctrl Pts',(-2.78549409123657,-1.,2.97111781461349));
#40729=CARTESIAN_POINT('Ctrl Pts',(-2.79253615718147,-1.,2.97426288347475));
#40730=CARTESIAN_POINT('Ctrl Pts',(-2.79960153278186,-1.,2.97737733718242));
#40731=CARTESIAN_POINT('Ctrl Pts',(-2.80668968101162,-1.,2.98046109647299));
#40732=CARTESIAN_POINT('Ctrl Pts',(-2.81380019196454,-1.,2.9835141977994));
#40733=CARTESIAN_POINT('Ctrl Pts',(-2.82093279065704,-1.,2.98653680669434));
#40734=CARTESIAN_POINT('Ctrl Pts',(-2.82808728190402,-1.,2.98952916401699));
#40735=CARTESIAN_POINT('Ctrl Pts',(-2.83526351254383,-1.,2.99249155170479));
#40736=CARTESIAN_POINT('Ctrl Pts',(-2.84246132984334,-1.,2.995424253416));
#40737=CARTESIAN_POINT('Ctrl Pts',(-2.84968053289104,-1.,2.99832751144566));
#40738=CARTESIAN_POINT('Ctrl Pts',(-2.85692085715129,-1.,3.0012015079552));
#40739=CARTESIAN_POINT('Ctrl Pts',(-2.86418200833065,-1.,3.00404638316245));
#40740=CARTESIAN_POINT('Ctrl Pts',(-2.87146368430104,-1.,3.00686224485374));
#40741=CARTESIAN_POINT('Ctrl Pts',(-2.87876560072799,-1.,3.0096491810855));
#40742=CARTESIAN_POINT('Ctrl Pts',(-2.88608751706796,-1.,3.01240727309568));
#40743=CARTESIAN_POINT('Ctrl Pts',(-2.8934292556764,-1.,3.01513660433291));
#40744=CARTESIAN_POINT('Ctrl Pts',(-2.90079069102661,-1.,3.01783725123646));
#40745=CARTESIAN_POINT('Ctrl Pts',(-2.90669553303902,-1.,3.01997487194926));
#40746=CARTESIAN_POINT('Ctrl Pts',(-2.91113297349052,-1.,3.02156522743299));
#40747=CARTESIAN_POINT('Ctrl Pts',(-2.91409518070707,-1.,3.02261975104912));
#40748=CARTESIAN_POINT('Ctrl Pts',(-2.91557726271063,-1.,3.02314558451372));
#40749=CARTESIAN_POINT('',(-3.02314558451372,-1.,2.91557726271063));
#40750=CARTESIAN_POINT('',(-2.91557726271063,-1.,3.02314558451372));
#40751=CARTESIAN_POINT('',(-2.79140942341258,-1.,2.50410331873176));
#40752=CARTESIAN_POINT('Ctrl Pts',(-3.02314558451372,-1.,2.91557726271063));
#40753=CARTESIAN_POINT('Ctrl Pts',(-3.02261975104593,-1.,2.91409518070399));
#40754=CARTESIAN_POINT('Ctrl Pts',(-3.02156522742431,-1.,2.91113297348212));
#40755=CARTESIAN_POINT('Ctrl Pts',(-3.01997487193503,-1.,2.90669553302526));
#40756=CARTESIAN_POINT('Ctrl Pts',(-3.01783725121981,-1.,2.9007906910105));
#40757=CARTESIAN_POINT('Ctrl Pts',(-3.01513660431928,-1.,2.89342925566321));
#40758=CARTESIAN_POINT('Ctrl Pts',(-3.01240727308829,-1.,2.8860875170608));
#40759=CARTESIAN_POINT('Ctrl Pts',(-3.00964918108476,-1.,2.87876560072727));
#40760=CARTESIAN_POINT('Ctrl Pts',(-3.00686224485784,-1.,2.87146368430502));
#40761=CARTESIAN_POINT('Ctrl Pts',(-3.00404638316867,-1.,2.86418200833667));
#40762=CARTESIAN_POINT('Ctrl Pts',(-3.00120150796095,-1.,2.85692085715686));
#40763=CARTESIAN_POINT('Ctrl Pts',(-2.99832751144925,-1.,2.84968053289451));
#40764=CARTESIAN_POINT('Ctrl Pts',(-2.99542425341685,-1.,2.84246132984415));
#40765=CARTESIAN_POINT('Ctrl Pts',(-2.9924915517034,-1.,2.83526351254248));
#40766=CARTESIAN_POINT('Ctrl Pts',(-2.98952916401446,-1.,2.82808728190157));
#40767=CARTESIAN_POINT('Ctrl Pts',(-2.9865368066918,-1.,2.82093279065457));
#40768=CARTESIAN_POINT('Ctrl Pts',(-2.98351419779767,-1.,2.81380019196286));
#40769=CARTESIAN_POINT('Ctrl Pts',(-2.98046109647241,-1.,2.80668968101106));
#40770=CARTESIAN_POINT('Ctrl Pts',(-2.97737733718287,-1.,2.7996015327823));
#40771=CARTESIAN_POINT('Ctrl Pts',(-2.9742628834758,-1.,2.79253615718248));
#40772=CARTESIAN_POINT('Ctrl Pts',(-2.97111781461465,-1.,2.78549409123769));
#40773=CARTESIAN_POINT('Ctrl Pts',(-2.96794221043036,-1.,2.7784758954285));
#40774=CARTESIAN_POINT('Ctrl Pts',(-2.96473605585583,-1.,2.77148206836498));
#40775=CARTESIAN_POINT('Ctrl Pts',(-2.96149914764818,-1.,2.76451296269557));
#40776=CARTESIAN_POINT('Ctrl Pts',(-2.95823097665896,-1.,2.7575686788835));
#40777=CARTESIAN_POINT('Ctrl Pts',(-2.95493069316161,-1.,2.75064903318947));
#40778=CARTESIAN_POINT('Ctrl Pts',(-2.95159737214266,-1.,2.74375379492172));
#40779=CARTESIAN_POINT('Ctrl Pts',(-2.94823023414364,-1.,2.73688288329808));
#40780=CARTESIAN_POINT('Ctrl Pts',(-2.94482887675143,-1.,2.73003657371617));
#40781=CARTESIAN_POINT('Ctrl Pts',(-2.94139351933897,-1.,2.72321571511337));
#40782=CARTESIAN_POINT('Ctrl Pts',(-2.93792519474972,-1.,2.71642190053592));
#40783=CARTESIAN_POINT('Ctrl Pts',(-2.93442516311179,-1.,2.70965695523787));
#40784=CARTESIAN_POINT('Ctrl Pts',(-2.9308943823375,-1.,2.70292247416885));
#40785=CARTESIAN_POINT('Ctrl Pts',(-2.92733294395267,-1.,2.69621932864301));
#40786=CARTESIAN_POINT('Ctrl Pts',(-2.92373955325875,-1.,2.68954721165339));
#40787=CARTESIAN_POINT('Ctrl Pts',(-2.92011090722152,-1.,2.68290409279688));
#40788=CARTESIAN_POINT('Ctrl Pts',(-2.91644290704285,-1.,2.67628728855312));
#40789=CARTESIAN_POINT('Ctrl Pts',(-2.91273193382882,-1.,2.66969458792631));
#40790=CARTESIAN_POINT('Ctrl Pts',(-2.90897617968923,-1.,2.6631254261681));
#40791=CARTESIAN_POINT('Ctrl Pts',(-2.90517678087461,-1.,2.65658188464282));
#40792=CARTESIAN_POINT('Ctrl Pts',(-2.90133950224867,-1.,2.65007017365564));
#40793=CARTESIAN_POINT('Ctrl Pts',(-2.89747231723345,-1.,2.64359851684131));
#40794=CARTESIAN_POINT('Ctrl Pts',(-2.89358228854544,-1.,2.63717442263932));
#40795=CARTESIAN_POINT('Ctrl Pts',(-2.88967244854239,-1.,2.63080195420767));
#40796=CARTESIAN_POINT('Ctrl Pts',(-2.88573922195059,-1.,2.62447947640262));
#40797=CARTESIAN_POINT('Ctrl Pts',(-2.88176821427525,-1.,2.61819596473108));
#40798=CARTESIAN_POINT('Ctrl Pts',(-2.87773881947916,-1.,2.61193507170955));
#40799=CARTESIAN_POINT('Ctrl Pts',(-2.87363176656501,-1.,2.60568177881303));
#40800=CARTESIAN_POINT('Ctrl Pts',(-2.86943633170722,-1.,2.5994287522321));
#40801=CARTESIAN_POINT('Ctrl Pts',(-2.86515629953513,-1.,2.59318160184908));
#40802=CARTESIAN_POINT('Ctrl Pts',(-2.86081999003629,-1.,2.58696770643524));
#40803=CARTESIAN_POINT('Ctrl Pts',(-2.85647171715092,-1.,2.58082875254357));
#40804=CARTESIAN_POINT('Ctrl Pts',(-2.85215360144431,-1.,2.57480482727081));
#40805=CARTESIAN_POINT('Ctrl Pts',(-2.84788893329067,-1.,2.56891984251721));
#40806=CARTESIAN_POINT('Ctrl Pts',(-2.84366802680237,-1.,2.56316920798513));
#40807=CARTESIAN_POINT('Ctrl Pts',(-2.83942515220782,-1.,2.55749952145241));
#40808=CARTESIAN_POINT('Ctrl Pts',(-2.83505269592536,-1.,2.55182152807077));
#40809=CARTESIAN_POINT('Ctrl Pts',(-2.83044254225917,-1.,2.54604736792655));
#40810=CARTESIAN_POINT('Ctrl Pts',(-2.8255216764922,-1.,2.54012272520199));
#40811=CARTESIAN_POINT('Ctrl Pts',(-2.82028550483689,-1.,2.53405679667412));
#40812=CARTESIAN_POINT('Ctrl Pts',(-2.81484379048475,-1.,2.52796388055278));
#40813=CARTESIAN_POINT('Ctrl Pts',(-2.80941521966941,-1.,2.52205778589653));
#40814=CARTESIAN_POINT('Ctrl Pts',(-2.80427363984653,-1.,2.51660190465805));
#40815=CARTESIAN_POINT('Ctrl Pts',(-2.79970585014168,-1.,2.51186983687818));
#40816=CARTESIAN_POINT('Ctrl Pts',(-2.79596878057287,-1.,2.50810555977671));
#40817=CARTESIAN_POINT('Ctrl Pts',(-2.79344192164147,-1.,2.50567182569081));
#40818=CARTESIAN_POINT('Ctrl Pts',(-2.79217568804755,-1.,2.50455968395146));
#40819=CARTESIAN_POINT('Ctrl Pts',(-2.79164172518905,-1.,2.50417932839313));
#40820=CARTESIAN_POINT('Ctrl Pts',(-2.79145823440781,-1.,2.50410700351493));
#40821=CARTESIAN_POINT('Ctrl Pts',(-2.79140942341258,-1.,2.50410331873176));
#40822=CARTESIAN_POINT('',(-2.90994629141562,-1.,2.36531447826213));
#40823=CARTESIAN_POINT('Origin',(0.,-1.,0.));
#40824=CARTESIAN_POINT('',(-3.35260583073571,-1.,2.52982887637028));
#40825=CARTESIAN_POINT('Ctrl Pts',(-2.90994629141562,-1.,2.36531447826213));
#40826=CARTESIAN_POINT('Ctrl Pts',(-2.90995756655558,-1.,2.3653621118858));
#40827=CARTESIAN_POINT('Ctrl Pts',(-2.9100577052777,-1.,2.36553202948741));
#40828=CARTESIAN_POINT('Ctrl Pts',(-2.91051690822262,-1.,2.36599991765853));
#40829=CARTESIAN_POINT('Ctrl Pts',(-2.91181344022628,-1.,2.36707658451709));
#40830=CARTESIAN_POINT('Ctrl Pts',(-2.91461249883016,-1.,2.36919161373074));
#40831=CARTESIAN_POINT('Ctrl Pts',(-2.9189150379156,-1.,2.37229381109939));
#40832=CARTESIAN_POINT('Ctrl Pts',(-2.92430340582912,-1.,2.37606510524271));
#40833=CARTESIAN_POINT('Ctrl Pts',(-2.93049643640517,-1.,2.3802898958232));
#40834=CARTESIAN_POINT('Ctrl Pts',(-2.93717903280599,-1.,2.38472771516476));
#40835=CARTESIAN_POINT('Ctrl Pts',(-2.94404820669135,-1.,2.38914929090806));
#40836=CARTESIAN_POINT('Ctrl Pts',(-2.95085857128372,-1.,2.39337207631613));
#40837=CARTESIAN_POINT('Ctrl Pts',(-2.95748006482811,-1.,2.39730553974412));
#40838=CARTESIAN_POINT('Ctrl Pts',(-2.96390432240181,-1.,2.40095565711535));
#40839=CARTESIAN_POINT('Ctrl Pts',(-2.97019641312272,-1.,2.40438604734848));
#40840=CARTESIAN_POINT('Ctrl Pts',(-2.97646002822395,-1.,2.40768975073691));
#40841=CARTESIAN_POINT('Ctrl Pts',(-2.98280015815132,-1.,2.41095909342591));
#40842=CARTESIAN_POINT('Ctrl Pts',(-2.98927983005851,-1.,2.4142506419963));
#40843=CARTESIAN_POINT('Ctrl Pts',(-2.99590509293561,-1.,2.4175732450056));
#40844=CARTESIAN_POINT('Ctrl Pts',(-3.00264868586038,-1.,2.42090763946812));
#40845=CARTESIAN_POINT('Ctrl Pts',(-3.00946442616674,-1.,2.42421849439625));
#40846=CARTESIAN_POINT('Ctrl Pts',(-3.01630420830494,-1.,2.4274685626416));
#40847=CARTESIAN_POINT('Ctrl Pts',(-3.02313656035977,-1.,2.43063415586615));
#40848=CARTESIAN_POINT('Ctrl Pts',(-3.02995534946946,-1.,2.43371241361462));
#40849=CARTESIAN_POINT('Ctrl Pts',(-3.03676949672797,-1.,2.43671278042394));
#40850=CARTESIAN_POINT('Ctrl Pts',(-3.04359685040545,-1.,2.43965194061849));
#40851=CARTESIAN_POINT('Ctrl Pts',(-3.05045678021509,-1.,2.44254768923109));
#40852=CARTESIAN_POINT('Ctrl Pts',(-3.05736242671521,-1.,2.44541251892568));
#40853=CARTESIAN_POINT('Ctrl Pts',(-3.06431596421422,-1.,2.44824970516558));
#40854=CARTESIAN_POINT('Ctrl Pts',(-3.0713129052131,-1.,2.45105688854432));
#40855=CARTESIAN_POINT('Ctrl Pts',(-3.07834472886145,-1.,2.45382826787795));
#40856=CARTESIAN_POINT('Ctrl Pts',(-3.08540206545313,-1.,2.45655725437037));
#40857=CARTESIAN_POINT('Ctrl Pts',(-3.09247787931881,-1.,2.45923912563875));
#40858=CARTESIAN_POINT('Ctrl Pts',(-3.09956993697048,-1.,2.4618730850188));
#40859=CARTESIAN_POINT('Ctrl Pts',(-3.10667907901981,-1.,2.46446082979645));
#40860=CARTESIAN_POINT('Ctrl Pts',(-3.11380805536124,-1.,2.46700558843507));
#40861=CARTESIAN_POINT('Ctrl Pts',(-3.12096015766984,-1.,2.4695109894747));
#40862=CARTESIAN_POINT('Ctrl Pts',(-3.12813790805948,-1.,2.47197997765868));
#40863=CARTESIAN_POINT('Ctrl Pts',(-3.13534181229282,-1.,2.47441378371923));
#40864=CARTESIAN_POINT('Ctrl Pts',(-3.14257099546531,-1.,2.47681245356095));
#40865=CARTESIAN_POINT('Ctrl Pts',(-3.14982373241335,-1.,2.47917529057016));
#40866=CARTESIAN_POINT('Ctrl Pts',(-3.15709802322735,-1.,2.48150133566568));
#40867=CARTESIAN_POINT('Ctrl Pts',(-3.16439213290181,-1.,2.48378981792739));
#40868=CARTESIAN_POINT('Ctrl Pts',(-3.17170518863357,-1.,2.48604065348619));
#40869=CARTESIAN_POINT('Ctrl Pts',(-3.17903698136679,-1.,2.48825428288243));
#40870=CARTESIAN_POINT('Ctrl Pts',(-3.18638771282315,-1.,2.49043146334095));
#40871=CARTESIAN_POINT('Ctrl Pts',(-3.19375775555814,-1.,2.4925730723986));
#40872=CARTESIAN_POINT('Ctrl Pts',(-3.20114742397549,-1.,2.49467992057726));
#40873=CARTESIAN_POINT('Ctrl Pts',(-3.2085566984974,-1.,2.49675252647298));
#40874=CARTESIAN_POINT('Ctrl Pts',(-3.21598526261157,-1.,2.49879114599293));
#40875=CARTESIAN_POINT('Ctrl Pts',(-3.22343262620387,-1.,2.5007958720187));
#40876=CARTESIAN_POINT('Ctrl Pts',(-3.23089822320596,-1.,2.50276671338074));
#40877=CARTESIAN_POINT('Ctrl Pts',(-3.23838151080383,-1.,2.50470367580078));
#40878=CARTESIAN_POINT('Ctrl Pts',(-3.24588208984042,-1.,2.50660685940645));
#40879=CARTESIAN_POINT('Ctrl Pts',(-3.25339971461265,-1.,2.50847647070936));
#40880=CARTESIAN_POINT('Ctrl Pts',(-3.26093423001716,-1.,2.51031277813697));
#40881=CARTESIAN_POINT('Ctrl Pts',(-3.26848552888271,-1.,2.51211608411539));
#40882=CARTESIAN_POINT('Ctrl Pts',(-3.27605350473048,-1.,2.51388669270329));
#40883=CARTESIAN_POINT('Ctrl Pts',(-3.28363799702583,-1.,2.51562487464215));
#40884=CARTESIAN_POINT('Ctrl Pts',(-3.2912387729863,-1.,2.51733085123316));
#40885=CARTESIAN_POINT('Ctrl Pts',(-3.29885556387661,-1.,2.51900480700548));
#40886=CARTESIAN_POINT('Ctrl Pts',(-3.30648808814986,-1.,2.52064689568167));
#40887=CARTESIAN_POINT('Ctrl Pts',(-3.31413607874727,-1.,2.52225724871375));
#40888=CARTESIAN_POINT('Ctrl Pts',(-3.32179931079521,-1.,2.52383598396878));
#40889=CARTESIAN_POINT('Ctrl Pts',(-3.32947762189049,-1.,2.52538321165774));
#40890=CARTESIAN_POINT('Ctrl Pts',(-3.33717090000955,-1.,2.52689902691551));
#40891=CARTESIAN_POINT('Ctrl Pts',(-3.34333744117093,-1.,2.52808660916879));
#40892=CARTESIAN_POINT('Ctrl Pts',(-3.34796903577628,-1.,2.5289632161143));
#40893=CARTESIAN_POINT('Ctrl Pts',(-3.35105973714426,-1.,2.52954136549357));
#40894=CARTESIAN_POINT('Ctrl Pts',(-3.35260583073571,-1.,2.52982887637028));
#40895=CARTESIAN_POINT('',(-3.44202241512147,-1.,2.40675750623143));
#40896=CARTESIAN_POINT('',(-3.35260583073571,-1.,2.52982887637028));
#40897=CARTESIAN_POINT('',(-3.14877060440327,-1.,2.03660101169715));
#40898=CARTESIAN_POINT('Ctrl Pts',(-3.44202241512147,-1.,2.40675750623143));
#40899=CARTESIAN_POINT('Ctrl Pts',(-3.44127120683039,-1.,2.4053759295909));
#40900=CARTESIAN_POINT('Ctrl Pts',(-3.43976627484234,-1.,2.40261515589405));
#40901=CARTESIAN_POINT('Ctrl Pts',(-3.43750133064416,-1.,2.39848113410292));
#40902=CARTESIAN_POINT('Ctrl Pts',(-3.4344663067854,-1.,2.39298338804493));
#40903=CARTESIAN_POINT('Ctrl Pts',(-3.4306473271292,-1.,2.38613505843552));
#40904=CARTESIAN_POINT('Ctrl Pts',(-3.42680309754399,-1.,2.37931067028926));
#40905=CARTESIAN_POINT('Ctrl Pts',(-3.42293356216511,-1.,2.37251035954292));
#40906=CARTESIAN_POINT('Ctrl Pts',(-3.41903866635852,-1.,2.36573431470642));
#40907=CARTESIAN_POINT('Ctrl Pts',(-3.41511836751469,-1.,2.35898278606946));
#40908=CARTESIAN_POINT('Ctrl Pts',(-3.41117262314119,-1.,2.35225606824109));
#40909=CARTESIAN_POINT('Ctrl Pts',(-3.40720137404297,-1.,2.34555447649188));
#40910=CARTESIAN_POINT('Ctrl Pts',(-3.40320452776743,-1.,2.33887832342782));
#40911=CARTESIAN_POINT('Ctrl Pts',(-3.39918194577956,-1.,2.33222789882489));
#40912=CARTESIAN_POINT('Ctrl Pts',(-3.39513342019756,-1.,2.3256034390248));
#40913=CARTESIAN_POINT('Ctrl Pts',(-3.39105869474822,-1.,2.31900513925424));
#40914=CARTESIAN_POINT('Ctrl Pts',(-3.38695751492462,-1.,2.31243319489367));
#40915=CARTESIAN_POINT('Ctrl Pts',(-3.3828296733661,-1.,2.30588783640343));
#40916=CARTESIAN_POINT('Ctrl Pts',(-3.37867504959433,-1.,2.29936936127624));
#40917=CARTESIAN_POINT('Ctrl Pts',(-3.37449367172826,-1.,2.29287818007393));
#40918=CARTESIAN_POINT('Ctrl Pts',(-3.37028570206488,-1.,2.28641481081137));
#40919=CARTESIAN_POINT('Ctrl Pts',(-3.36605130713076,-1.,2.27997979458037));
#40920=CARTESIAN_POINT('Ctrl Pts',(-3.36179055004409,-1.,2.2735736262093));
#40921=CARTESIAN_POINT('Ctrl Pts',(-3.35750328523061,-1.,2.2671966857991));
#40922=CARTESIAN_POINT('Ctrl Pts',(-3.35318902552626,-1.,2.26084915222449));
#40923=CARTESIAN_POINT('Ctrl Pts',(-3.34884690292285,-1.,2.25453097693483));
#40924=CARTESIAN_POINT('Ctrl Pts',(-3.34447596770723,-1.,2.24824207678256));
#40925=CARTESIAN_POINT('Ctrl Pts',(-3.34007543738025,-1.,2.24198249391422));
#40926=CARTESIAN_POINT('Ctrl Pts',(-3.33564495756482,-1.,2.23575256328812));
#40927=CARTESIAN_POINT('Ctrl Pts',(-3.33118487773611,-1.,2.22955308907233));
#40928=CARTESIAN_POINT('Ctrl Pts',(-3.3266964672289,-1.,2.22338548312772));
#40929=CARTESIAN_POINT('Ctrl Pts',(-3.32218125618968,-1.,2.21725135110898));
#40930=CARTESIAN_POINT('Ctrl Pts',(-3.31764044024235,-1.,2.21115211847875));
#40931=CARTESIAN_POINT('Ctrl Pts',(-3.31307424608949,-1.,2.20508863150607));
#40932=CARTESIAN_POINT('Ctrl Pts',(-3.30848134694595,-1.,2.19906078949923));
#40933=CARTESIAN_POINT('Ctrl Pts',(-3.30385816281831,-1.,2.19306710376111));
#40934=CARTESIAN_POINT('Ctrl Pts',(-3.29920022557639,-1.,2.18710556500327));
#40935=CARTESIAN_POINT('Ctrl Pts',(-3.2945036150049,-1.,2.18117455557065));
#40936=CARTESIAN_POINT('Ctrl Pts',(-3.28976645712568,-1.,2.17527380048423));
#40937=CARTESIAN_POINT('Ctrl Pts',(-3.28499019979724,-1.,2.16940517773455));
#40938=CARTESIAN_POINT('Ctrl Pts',(-3.280181508414,-1.,2.16357391934425));
#40939=CARTESIAN_POINT('Ctrl Pts',(-3.27534954469187,-1.,2.15778690038347));
#40940=CARTESIAN_POINT('Ctrl Pts',(-3.27050245897228,-1.,2.15205043199808));
#40941=CARTESIAN_POINT('Ctrl Pts',(-3.26564388189759,-1.,2.1463680529566));
#40942=CARTESIAN_POINT('Ctrl Pts',(-3.26077002641879,-1.,2.14073870754264));
#40943=CARTESIAN_POINT('Ctrl Pts',(-3.25586495065054,-1.,2.13515375878803));
#40944=CARTESIAN_POINT('Ctrl Pts',(-3.25090574494028,-1.,2.12960028396832));
#40945=CARTESIAN_POINT('Ctrl Pts',(-3.24587102613376,-1.,2.12406646410962));
#40946=CARTESIAN_POINT('Ctrl Pts',(-3.24074905517293,-1.,2.11854673326979));
#40947=CARTESIAN_POINT('Ctrl Pts',(-3.23554444767099,-1.,2.11304604021773));
#40948=CARTESIAN_POINT('Ctrl Pts',(-3.23028945793289,-1.,2.10758699642451));
#40949=CARTESIAN_POINT('Ctrl Pts',(-3.22503437553434,-1.,2.10220384298492));
#40950=CARTESIAN_POINT('Ctrl Pts',(-3.21982707347009,-1.,2.09692958434895));
#40951=CARTESIAN_POINT('Ctrl Pts',(-3.21469429601654,-1.,2.09178419460443));
#40952=CARTESIAN_POINT('Ctrl Pts',(-3.20962575845463,-1.,2.08676465517455));
#40953=CARTESIAN_POINT('Ctrl Pts',(-3.2045481863073,-1.,2.08182850370878));
#40954=CARTESIAN_POINT('Ctrl Pts',(-3.19934132836019,-1.,2.07690441870722));
#40955=CARTESIAN_POINT('Ctrl Pts',(-3.19388465568252,-1.,2.07192253497857));
#40956=CARTESIAN_POINT('Ctrl Pts',(-3.18809755562368,-1.,2.06684062744112));
#40957=CARTESIAN_POINT('Ctrl Pts',(-3.18197692964614,-1.,2.06166849827101));
#40958=CARTESIAN_POINT('Ctrl Pts',(-3.17564906975371,-1.,2.05650186773132));
#40959=CARTESIAN_POINT('Ctrl Pts',(-3.16936341689527,-1.,2.05151770247233));
#40960=CARTESIAN_POINT('Ctrl Pts',(-3.16343165058912,-1.,2.04693331247446));
#40961=CARTESIAN_POINT('Ctrl Pts',(-3.15817983946367,-1.,2.04297406404027));
#40962=CARTESIAN_POINT('Ctrl Pts',(-3.15389991674792,-1.,2.03984073791519));
#40963=CARTESIAN_POINT('Ctrl Pts',(-3.15102344775328,-1.,2.03783225495961));
#40964=CARTESIAN_POINT('Ctrl Pts',(-3.14959882629805,-1.,2.03693188810544));
#40965=CARTESIAN_POINT('Ctrl Pts',(-3.1490119366901,-1.,2.03663974554932));
#40966=CARTESIAN_POINT('Ctrl Pts',(-3.14881939088124,-1.,2.03659701539259));
#40967=CARTESIAN_POINT('Ctrl Pts',(-3.14877060440328,-1.,2.03660101169715));
#40968=CARTESIAN_POINT('',(-3.24413672884812,-1.,1.88097764062697));
#40969=CARTESIAN_POINT('Origin',(0.,-1.,0.));
#40970=CARTESIAN_POINT('',(-3.70708211654725,-1.,1.97421938526992));
#40971=CARTESIAN_POINT('Ctrl Pts',(-3.24413672884812,-1.,1.88097764062697));
#40972=CARTESIAN_POINT('Ctrl Pts',(-3.24415531671284,-1.,1.8810229239812));
#40973=CARTESIAN_POINT('Ctrl Pts',(-3.24428080353022,-1.,1.88117508446775));
#40974=CARTESIAN_POINT('Ctrl Pts',(-3.24480754676064,-1.,1.88156537699203));
#40975=CARTESIAN_POINT('Ctrl Pts',(-3.2462565441079,-1.,1.88242596600454));
#40976=CARTESIAN_POINT('Ctrl Pts',(-3.24935200511918,-1.,1.88407708646357));
#40977=CARTESIAN_POINT('Ctrl Pts',(-3.25408686339463,-1.,1.88646802523466));
#40978=CARTESIAN_POINT('Ctrl Pts',(-3.25999885193947,-1.,1.88934996203698));
#40979=CARTESIAN_POINT('Ctrl Pts',(-3.26677653888676,-1.,1.89255393500965));
#40980=CARTESIAN_POINT('Ctrl Pts',(-3.27407108933139,-1.,1.89589172903793));
#40981=CARTESIAN_POINT('Ctrl Pts',(-3.28154737912352,-1.,1.89918429230462));
#40982=CARTESIAN_POINT('Ctrl Pts',(-3.2889344860029,-1.,1.90228971247527));
#40983=CARTESIAN_POINT('Ctrl Pts',(-3.29608978722113,-1.,1.90513891864087));
#40984=CARTESIAN_POINT('Ctrl Pts',(-3.30300595568195,-1.,1.90773912171341));
#40985=CARTESIAN_POINT('Ctrl Pts',(-3.30975721158596,-1.,1.91014297830446));
#40986=CARTESIAN_POINT('Ctrl Pts',(-3.31646052426364,-1.,1.91242616234442));
#40987=CARTESIAN_POINT('Ctrl Pts',(-3.32323403454535,-1.,1.91466343916628));
#40988=CARTESIAN_POINT('Ctrl Pts',(-3.33014884257873,-1.,1.91690081930331));
#40989=CARTESIAN_POINT('Ctrl Pts',(-3.33721230710012,-1.,1.9191460961021));
#40990=CARTESIAN_POINT('Ctrl Pts',(-3.34439448941961,-1.,1.92138450828404));
#40991=CARTESIAN_POINT('Ctrl Pts',(-3.35164424847223,-1.,1.92358838440528));
#40992=CARTESIAN_POINT('Ctrl Pts',(-3.35890824422965,-1.,1.92572846125756));
#40993=CARTESIAN_POINT('Ctrl Pts',(-3.36615168657567,-1.,1.92778626543786));
#40994=CARTESIAN_POINT('Ctrl Pts',(-3.37336807068043,-1.,1.92975993109877));
#40995=CARTESIAN_POINT('Ctrl Pts',(-3.3805676852555,-1.,1.93165739093276));
#40996=CARTESIAN_POINT('Ctrl Pts',(-3.38777076883256,-1.,1.93349233176788));
#40997=CARTESIAN_POINT('Ctrl Pts',(-3.39499923640795,-1.,1.93527929945985));
#40998=CARTESIAN_POINT('Ctrl Pts',(-3.40226802104109,-1.,1.93702857723098));
#40999=CARTESIAN_POINT('Ctrl Pts',(-3.40957978266642,-1.,1.93874306008143));
#41000=CARTESIAN_POINT('Ctrl Pts',(-3.41692971994096,-1.,1.94042111965246));
#41001=CARTESIAN_POINT('Ctrl Pts',(-3.42430850941503,-1.,1.94205835913696));
#41002=CARTESIAN_POINT('Ctrl Pts',(-3.43170586602434,-1.,1.94364973660284));
#41003=CARTESIAN_POINT('Ctrl Pts',(-3.43911410197687,-1.,1.94519168842879));
#41004=CARTESIAN_POINT('Ctrl Pts',(-3.44653088665681,-1.,1.94668377715329));
#41005=CARTESIAN_POINT('Ctrl Pts',(-3.45395731584051,-1.,1.94812754766524));
#41006=CARTESIAN_POINT('Ctrl Pts',(-3.46139661060962,-1.,1.94952575850197));
#41007=CARTESIAN_POINT('Ctrl Pts',(-3.46885258974191,-1.,1.95088147859876));
#41008=CARTESIAN_POINT('Ctrl Pts',(-3.47632820495921,-1.,1.95219722189876));
#41009=CARTESIAN_POINT('Ctrl Pts',(-3.48382414832634,-1.,1.95347412486308));
#41010=CARTESIAN_POINT('Ctrl Pts',(-3.49133956289133,-1.,1.95471236969643));
#41011=CARTESIAN_POINT('Ctrl Pts',(-3.49887263575583,-1.,1.95591153823661));
#41012=CARTESIAN_POINT('Ctrl Pts',(-3.50642124159909,-1.,1.95707099606511));
#41013=CARTESIAN_POINT('Ctrl Pts',(-3.51398354617794,-1.,1.95819025316779));
#41014=CARTESIAN_POINT('Ctrl Pts',(-3.52155867431486,-1.,1.95926936324461));
#41015=CARTESIAN_POINT('Ctrl Pts',(-3.52914648844351,-1.,1.96030879411566));
#41016=CARTESIAN_POINT('Ctrl Pts',(-3.53674730625813,-1.,1.96130926212689));
#41017=CARTESIAN_POINT('Ctrl Pts',(-3.54436163300443,-1.,1.96227157573067));
#41018=CARTESIAN_POINT('Ctrl Pts',(-3.55198990600886,-1.,1.96319648628644));
#41019=CARTESIAN_POINT('Ctrl Pts',(-3.55963218706096,-1.,1.96408450906812));
#41020=CARTESIAN_POINT('Ctrl Pts',(-3.56728820357791,-1.,1.96493594634567));
#41021=CARTESIAN_POINT('Ctrl Pts',(-3.57495748600959,-1.,1.96575096652789));
#41022=CARTESIAN_POINT('Ctrl Pts',(-3.58263947663829,-1.,1.96652966688911));
#41023=CARTESIAN_POINT('Ctrl Pts',(-3.59033364022801,-1.,1.96727213799544));
#41024=CARTESIAN_POINT('Ctrl Pts',(-3.59803959819938,-1.,1.96797854118369));
#41025=CARTESIAN_POINT('Ctrl Pts',(-3.60575714017989,-1.,1.9686491188594));
#41026=CARTESIAN_POINT('Ctrl Pts',(-3.61348615496704,-1.,1.96928416040877));
#41027=CARTESIAN_POINT('Ctrl Pts',(-3.62122658401893,-1.,1.96988398129978));
#41028=CARTESIAN_POINT('Ctrl Pts',(-3.62897836973293,-1.,1.97044889850463));
#41029=CARTESIAN_POINT('Ctrl Pts',(-3.63674139590412,-1.,1.97097920454464));
#41030=CARTESIAN_POINT('Ctrl Pts',(-3.64451546723514,-1.,1.97147515441164));
#41031=CARTESIAN_POINT('Ctrl Pts',(-3.652300347166,-1.,1.9719369724024));
#41032=CARTESIAN_POINT('Ctrl Pts',(-3.6600957816636,-1.,1.9723648543905));
#41033=CARTESIAN_POINT('Ctrl Pts',(-3.66790152752075,-1.,1.97275897198678));
#41034=CARTESIAN_POINT('Ctrl Pts',(-3.67571738107084,-1.,1.97311947678516));
#41035=CARTESIAN_POINT('Ctrl Pts',(-3.68354319915092,-1.,1.97344650304519));
#41036=CARTESIAN_POINT('Ctrl Pts',(-3.69137888599902,-1.,1.97374016225483));
#41037=CARTESIAN_POINT('Ctrl Pts',(-3.6976552856004,-1.,1.97394846383216));
#41038=CARTESIAN_POINT('Ctrl Pts',(-3.70236698912904,-1.,1.97408973726715));
#41039=CARTESIAN_POINT('Ctrl Pts',(-3.70551008132332,-1.,1.97417727645308));
#41040=CARTESIAN_POINT('Ctrl Pts',(-3.70708211654725,-1.,1.97421938526992));
#41041=CARTESIAN_POINT('',(-3.77614523045147,-1.,1.8386753923786));
#41042=CARTESIAN_POINT('',(-3.70708211654725,-1.,1.97421938526992));
#41043=CARTESIAN_POINT('',(-3.42859860294306,-1.,1.5189508286633));
#41044=CARTESIAN_POINT('Ctrl Pts',(-3.77614523045147,-1.,1.8386753923786));
#41045=CARTESIAN_POINT('Ctrl Pts',(-3.77518714457833,-1.,1.83742834010626));
#41046=CARTESIAN_POINT('Ctrl Pts',(-3.77326886064398,-1.,1.83493697934534));
#41047=CARTESIAN_POINT('Ctrl Pts',(-3.77038509817999,-1.,1.83120816955645));
#41048=CARTESIAN_POINT('Ctrl Pts',(-3.76652740353775,-1.,1.82625289220915));
#41049=CARTESIAN_POINT('Ctrl Pts',(-3.76168412707948,-1.,1.82008629694091));
#41050=CARTESIAN_POINT('Ctrl Pts',(-3.75681965683071,-1.,1.8139472983358));
#41051=CARTESIAN_POINT('Ctrl Pts',(-3.75193395887977,-1.,1.80783603939617));
#41052=CARTESIAN_POINT('Ctrl Pts',(-3.74702700875467,-1.,1.8017527148577));
#41053=CARTESIAN_POINT('Ctrl Pts',(-3.74209880352445,-1.,1.79569757859422));
#41054=CARTESIAN_POINT('Ctrl Pts',(-3.73714934730681,-1.,1.78967092823491));
#41055=CARTESIAN_POINT('Ctrl Pts',(-3.7321786309547,-1.,1.78367308442901));
#41056=CARTESIAN_POINT('Ctrl Pts',(-3.72718661205609,-1.,1.77770437039658));
#41057=CARTESIAN_POINT('Ctrl Pts',(-3.72217319911254,-1.,1.77176509401761));
#41058=CARTESIAN_POINT('Ctrl Pts',(-3.71713822377359,-1.,1.76585552124394));
#41059=CARTESIAN_POINT('Ctrl Pts',(-3.71208146346136,-1.,1.75997588498865));
#41060=CARTESIAN_POINT('Ctrl Pts',(-3.70700269736659,-1.,1.75412641804042));
#41061=CARTESIAN_POINT('Ctrl Pts',(-3.7019017567335,-1.,1.74830738046057));
#41062=CARTESIAN_POINT('Ctrl Pts',(-3.69677856910517,-1.,1.74251908492617));
#41063=CARTESIAN_POINT('Ctrl Pts',(-3.69163322648036,-1.,1.73676193254557));
#41064=CARTESIAN_POINT('Ctrl Pts',(-3.68646597019332,-1.,1.73103640956717));
#41065=CARTESIAN_POINT('Ctrl Pts',(-3.68127704936579,-1.,1.72534302437056));
#41066=CARTESIAN_POINT('Ctrl Pts',(-3.67606660374709,-1.,1.71968225581808));
#41067=CARTESIAN_POINT('Ctrl Pts',(-3.67083454901611,-1.,1.71405450210383));
#41068=CARTESIAN_POINT('Ctrl Pts',(-3.66558043198876,-1.,1.70846001610956));
#41069=CARTESIAN_POINT('Ctrl Pts',(-3.66030338774847,-1.,1.70289888566873));
#41070=CARTESIAN_POINT('Ctrl Pts',(-3.65500246526749,-1.,1.69737117722534));
#41071=CARTESIAN_POINT('Ctrl Pts',(-3.64967689827371,-1.,1.69187705481689));
#41072=CARTESIAN_POINT('Ctrl Pts',(-3.64432638915203,-1.,1.68641690471457));
#41073=CARTESIAN_POINT('Ctrl Pts',(-3.63895140887462,-1.,1.68099146651586));
#41074=CARTESIAN_POINT('Ctrl Pts',(-3.63355343201232,-1.,1.67560193613156));
#41075=CARTESIAN_POINT('Ctrl Pts',(-3.62813422105271,-1.,1.67024966008045));
#41076=CARTESIAN_POINT('Ctrl Pts',(-3.62269517989109,-1.,1.66493585923855));
#41077=CARTESIAN_POINT('Ctrl Pts',(-3.61723666482456,-1.,1.65966133399186));
#41078=CARTESIAN_POINT('Ctrl Pts',(-3.61175734965127,-1.,1.65442619244325));
#41079=CARTESIAN_POINT('Ctrl Pts',(-3.60625346556992,-1.,1.64922952425832));
#41080=CARTESIAN_POINT('Ctrl Pts',(-3.60072028513845,-1.,1.64407004385582));
#41081=CARTESIAN_POINT('Ctrl Pts',(-3.59515368334893,-1.,1.63894676675352));
#41082=CARTESIAN_POINT('Ctrl Pts',(-3.58955176627879,-1.,1.6338597145126));
#41083=CARTESIAN_POINT('Ctrl Pts',(-3.58391625774343,-1.,1.62881051550745));
#41084=CARTESIAN_POINT('Ctrl Pts',(-3.5782545595439,-1.,1.62380329464844));
#41085=CARTESIAN_POINT('Ctrl Pts',(-3.57257679609806,-1.,1.61884340915404));
#41086=CARTESIAN_POINT('Ctrl Pts',(-3.56689200468387,-1.,1.61393581747514));
#41087=CARTESIAN_POINT('Ctrl Pts',(-3.5612043248298,-1.,1.60908344685457));
#41088=CARTESIAN_POINT('Ctrl Pts',(-3.55550985096129,-1.,1.60428584699853));
#41089=CARTESIAN_POINT('Ctrl Pts',(-3.54979148634454,-1.,1.59953698113457));
#41090=CARTESIAN_POINT('Ctrl Pts',(-3.54402458182337,-1.,1.59482766949766));
#41091=CARTESIAN_POINT('Ctrl Pts',(-3.53818616861077,-1.,1.59014958368739));
#41092=CARTESIAN_POINT('Ctrl Pts',(-3.5322637814708,-1.,1.58549906268088));
#41093=CARTESIAN_POINT('Ctrl Pts',(-3.52626275334881,-1.,1.58088027227848));
#41094=CARTESIAN_POINT('Ctrl Pts',(-3.52021847865912,-1.,1.57631049988158));
#41095=CARTESIAN_POINT('Ctrl Pts',(-3.51418598431665,-1.,1.57181569799743));
#41096=CARTESIAN_POINT('Ctrl Pts',(-3.50821771695363,-1.,1.56742097575012));
#41097=CARTESIAN_POINT('Ctrl Pts',(-3.50234321621578,-1.,1.56314187758675));
#41098=CARTESIAN_POINT('Ctrl Pts',(-3.49655185179655,-1.,1.55897703097874));
#41099=CARTESIAN_POINT('Ctrl Pts',(-3.4907646087742,-1.,1.55489595901116));
#41100=CARTESIAN_POINT('Ctrl Pts',(-3.48485155928567,-1.,1.55084702970452));
#41101=CARTESIAN_POINT('Ctrl Pts',(-3.47868272898751,-1.,1.54678009290276));
#41102=CARTESIAN_POINT('Ctrl Pts',(-3.47217189224653,-1.,1.54266605398187));
#41103=CARTESIAN_POINT('Ctrl Pts',(-3.46531752207153,-1.,1.53851507915502));
#41104=CARTESIAN_POINT('Ctrl Pts',(-3.45825932955032,-1.,1.53440195378792));
#41105=CARTESIAN_POINT('Ctrl Pts',(-3.45127136828305,-1.,1.53046244461635));
#41106=CARTESIAN_POINT('Ctrl Pts',(-3.44469547526647,-1.,1.52686242875556));
#41107=CARTESIAN_POINT('Ctrl Pts',(-3.4388889597401,-1.,1.5237734895035));
#41108=CARTESIAN_POINT('Ctrl Pts',(-3.43417156977893,-1.,1.52134826724292));
#41109=CARTESIAN_POINT('Ctrl Pts',(-3.43101631893414,-1.,1.5198144909338));
#41110=CARTESIAN_POINT('Ctrl Pts',(-3.42946838852587,-1.,1.51914806898491));
#41111=CARTESIAN_POINT('Ctrl Pts',(-3.42884302333841,-1.,1.5189513329503));
#41112=CARTESIAN_POINT('Ctrl Pts',(-3.42864616361875,-1.,1.51893924967331));
#41113=CARTESIAN_POINT('Ctrl Pts',(-3.42859860294306,-1.,1.5189508286633));
#41114=CARTESIAN_POINT('',(-3.49844575334386,-1.,1.35032489087269));
#41115=CARTESIAN_POINT('Origin',(0.,-1.,0.));
#41116=CARTESIAN_POINT('',(-3.97027773754922,-1.,1.36999806084572));
#41117=CARTESIAN_POINT('Ctrl Pts',(-3.49844575334386,-1.,1.35032489087269));
#41118=CARTESIAN_POINT('Ctrl Pts',(-3.49847119623841,-1.,1.35036670893102));
#41119=CARTESIAN_POINT('Ctrl Pts',(-3.49861894124915,-1.,1.35049736560633));
#41120=CARTESIAN_POINT('Ctrl Pts',(-3.49920025459856,-1.,1.35080045218652));
#41121=CARTESIAN_POINT('Ctrl Pts',(-3.5007660381658,-1.,1.35142377279535));
#41122=CARTESIAN_POINT('Ctrl Pts',(-3.50408168106113,-1.,1.3525703284343));
#41123=CARTESIAN_POINT('Ctrl Pts',(-3.50913227060177,-1.,1.35419113576022));
#41124=CARTESIAN_POINT('Ctrl Pts',(-3.51542230699919,-1.,1.35611275237288));
#41125=CARTESIAN_POINT('Ctrl Pts',(-3.52261776117121,-1.,1.35821701528975));
#41126=CARTESIAN_POINT('Ctrl Pts',(-3.53034464961849,-1.,1.36037259643827));
#41127=CARTESIAN_POINT('Ctrl Pts',(-3.53824396425032,-1.,1.36245507339334));
#41128=CARTESIAN_POINT('Ctrl Pts',(-3.54602591832893,-1.,1.36436666257567));
#41129=CARTESIAN_POINT('Ctrl Pts',(-3.55353883995793,-1.,1.36606145456711));
#41130=CARTESIAN_POINT('Ctrl Pts',(-3.56077662028492,-1.,1.36754771771174));
#41131=CARTESIAN_POINT('Ctrl Pts',(-3.56782080304554,-1.,1.36886584973349));
#41132=CARTESIAN_POINT('Ctrl Pts',(-3.57479875549453,-1.,1.37007229485646));
#41133=CARTESIAN_POINT('Ctrl Pts',(-3.58183885982745,-1.,1.37122241663073));
#41134=CARTESIAN_POINT('Ctrl Pts',(-3.5890185384643,-1.,1.37235053661));
#41135=CARTESIAN_POINT('Ctrl Pts',(-3.59634627869117,-1.,1.37346320103184));
#41136=CARTESIAN_POINT('Ctrl Pts',(-3.60379020124038,-1.,1.37455051379642));
#41137=CARTESIAN_POINT('Ctrl Pts',(-3.61129546591082,-1.,1.37559314436641));
#41138=CARTESIAN_POINT('Ctrl Pts',(-3.61880481160408,-1.,1.37657053403102));
#41139=CARTESIAN_POINT('Ctrl Pts',(-3.62628098665112,-1.,1.37746987919868));
#41140=CARTESIAN_POINT('Ctrl Pts',(-3.63371727442448,-1.,1.37829035457324));
#41141=CARTESIAN_POINT('Ctrl Pts',(-3.64112507791112,-1.,1.37903818567347));
#41142=CARTESIAN_POINT('Ctrl Pts',(-3.64852652756444,-1.,1.37972372481598));
#41143=CARTESIAN_POINT('Ctrl Pts',(-3.65594554404396,-1.,1.38035791051215));
#41144=CARTESIAN_POINT('Ctrl Pts',(-3.66339848520874,-1.,1.38094856333558));
#41145=CARTESIAN_POINT('Ctrl Pts',(-3.67088843112282,-1.,1.38149812653876));
#41146=CARTESIAN_POINT('Ctrl Pts',(-3.6784103848243,-1.,1.38200574290626));
#41147=CARTESIAN_POINT('Ctrl Pts',(-3.68595444983844,-1.,1.38246852827185));
#41148=CARTESIAN_POINT('Ctrl Pts',(-3.69350967899523,-1.,1.38288311171649));
#41149=CARTESIAN_POINT('Ctrl Pts',(-3.70106792167894,-1.,1.38324717612862));
#41150=CARTESIAN_POINT('Ctrl Pts',(-3.70862680753343,-1.,1.38356065402122));
#41151=CARTESIAN_POINT('Ctrl Pts',(-3.7161876605181,-1.,1.38382489984585));
#41152=CARTESIAN_POINT('Ctrl Pts',(-3.72375409358805,-1.,1.3840421342895));
#41153=CARTESIAN_POINT('Ctrl Pts',(-3.73133035859283,-1.,1.38421479111531));
#41154=CARTESIAN_POINT('Ctrl Pts',(-3.73891976418099,-1.,1.38434489156456));
#41155=CARTESIAN_POINT('Ctrl Pts',(-3.7465231716786,-1.,1.38443344984389));
#41156=CARTESIAN_POINT('Ctrl Pts',(-3.75413976318727,-1.,1.38448077997155));
#41157=CARTESIAN_POINT('Ctrl Pts',(-3.76176768271347,-1.,1.38448675253343));
#41158=CARTESIAN_POINT('Ctrl Pts',(-3.76940473185775,-1.,1.38445107339517));
#41159=CARTESIAN_POINT('Ctrl Pts',(-3.77704902230441,-1.,1.38437354551435));
#41160=CARTESIAN_POINT('Ctrl Pts',(-3.78469969805134,-1.,1.38425435883773));
#41161=CARTESIAN_POINT('Ctrl Pts',(-3.79235669640907,-1.,1.38409399694588));
#41162=CARTESIAN_POINT('Ctrl Pts',(-3.80002044322169,-1.,1.38389311766701));
#41163=CARTESIAN_POINT('Ctrl Pts',(-3.80769156398429,-1.,1.38365244046226));
#41164=CARTESIAN_POINT('Ctrl Pts',(-3.81537060817765,-1.,1.38337263902766));
#41165=CARTESIAN_POINT('Ctrl Pts',(-3.82305771743715,-1.,1.38305421262724));
#41166=CARTESIAN_POINT('Ctrl Pts',(-3.83075266982138,-1.,1.38269750245086));
#41167=CARTESIAN_POINT('Ctrl Pts',(-3.83845502790609,-1.,1.38230274828774));
#41168=CARTESIAN_POINT('Ctrl Pts',(-3.84616425605705,-1.,1.38187013346089));
#41169=CARTESIAN_POINT('Ctrl Pts',(-3.85387983979557,-1.,1.38139983115075));
#41170=CARTESIAN_POINT('Ctrl Pts',(-3.86160143044187,-1.,1.38089205993067));
#41171=CARTESIAN_POINT('Ctrl Pts',(-3.86932885813403,-1.,1.38034709213129));
#41172=CARTESIAN_POINT('Ctrl Pts',(-3.87706205830865,-1.,1.37976523097187));
#41173=CARTESIAN_POINT('Ctrl Pts',(-3.88480102249461,-1.,1.37914679719446));
#41174=CARTESIAN_POINT('Ctrl Pts',(-3.89254574338385,-1.,1.37849211287981));
#41175=CARTESIAN_POINT('Ctrl Pts',(-3.90029615196255,-1.,1.3778014851263));
#41176=CARTESIAN_POINT('Ctrl Pts',(-3.90805209522729,-1.,1.3770751963376));
#41177=CARTESIAN_POINT('Ctrl Pts',(-3.91581337461825,-1.,1.37631350505516));
#41178=CARTESIAN_POINT('Ctrl Pts',(-3.92357976987132,-1.,1.37551664448057));
#41179=CARTESIAN_POINT('Ctrl Pts',(-3.93135106761941,-1.,1.37468482215784));
#41180=CARTESIAN_POINT('Ctrl Pts',(-3.93912709041791,-1.,1.37381821967499));
#41181=CARTESIAN_POINT('Ctrl Pts',(-3.94690771786926,-1.,1.37291699203423));
#41182=CARTESIAN_POINT('Ctrl Pts',(-3.95469287283105,-1.,1.37198126433139));
#41183=CARTESIAN_POINT('Ctrl Pts',(-3.96092458508407,-1.,1.37120515615663));
#41184=CARTESIAN_POINT('Ctrl Pts',(-3.96560037975788,-1.,1.37060761746027));
#41185=CARTESIAN_POINT('Ctrl Pts',(-3.9687184694173,-1.,1.37020239094758));
#41186=CARTESIAN_POINT('Ctrl Pts',(-3.97027773754922,-1.,1.36999806084572));
#41187=CARTESIAN_POINT('',(-4.01728681790024,-1.,1.22531898815164));
#41188=CARTESIAN_POINT('',(-3.97027773754922,-1.,1.36999806084572));
#41189=CARTESIAN_POINT('',(-3.62400312501199,-1.,0.963899035118985));
#41190=CARTESIAN_POINT('Ctrl Pts',(-4.01728681790024,-1.,1.22531898815164));
#41191=CARTESIAN_POINT('Ctrl Pts',(-4.01614544569895,-1.,1.22423716681317));
#41192=CARTESIAN_POINT('Ctrl Pts',(-4.01386104433519,-1.,1.22207656455845));
#41193=CARTESIAN_POINT('Ctrl Pts',(-4.01042947140789,-1.,1.21884478244403));
#41194=CARTESIAN_POINT('Ctrl Pts',(-4.00584409522722,-1.,1.21455398918133));
#41195=CARTESIAN_POINT('Ctrl Pts',(-4.00009577950721,-1.,1.20922097029551));
#41196=CARTESIAN_POINT('Ctrl Pts',(-3.99433084799666,-1.,1.20391852375139));
#41197=CARTESIAN_POINT('Ctrl Pts',(-3.98854928957189,-1.,1.19864679609566));
#41198=CARTESIAN_POINT('Ctrl Pts',(-3.98275111052561,-1.,1.19340598349475));
#41199=CARTESIAN_POINT('Ctrl Pts',(-3.97693634767754,-1.,1.18819633715539));
#41200=CARTESIAN_POINT('Ctrl Pts',(-3.97110505165415,-1.,1.18301815039831));
#41201=CARTESIAN_POINT('Ctrl Pts',(-3.96525726358159,-1.,1.17787174135592));
#41202=CARTESIAN_POINT('Ctrl Pts',(-3.95939299213276,-1.,1.17275743590361));
#41203=CARTESIAN_POINT('Ctrl Pts',(-3.95351219509876,-1.,1.16767555244438));
#41204=CARTESIAN_POINT('Ctrl Pts',(-3.94761474780583,-1.,1.16262637999157));
#41205=CARTESIAN_POINT('Ctrl Pts',(-3.94170046685203,-1.,1.15761018340956));
#41206=CARTESIAN_POINT('Ctrl Pts',(-3.9357691705628,-1.,1.1526272271632));
#41207=CARTESIAN_POINT('Ctrl Pts',(-3.92982073294257,-1.,1.14767779451123));
#41208=CARTESIAN_POINT('Ctrl Pts',(-3.92385513133997,-1.,1.14276220561593));
#41209=CARTESIAN_POINT('Ctrl Pts',(-3.91787251936827,-1.,1.13788084225554));
#41210=CARTESIAN_POINT('Ctrl Pts',(-3.91187321145649,-1.,1.13303414693896));
#41211=CARTESIAN_POINT('Ctrl Pts',(-3.90585753318737,-1.,1.12822258281553));
#41212=CARTESIAN_POINT('Ctrl Pts',(-3.89982569750025,-1.,1.12344660099043));
#41213=CARTESIAN_POINT('Ctrl Pts',(-3.89377768340344,-1.,1.11870660794603));
#41214=CARTESIAN_POINT('Ctrl Pts',(-3.88771308285171,-1.,1.11400292434429));
#41215=CARTESIAN_POINT('Ctrl Pts',(-3.88163105531724,-1.,1.10933577224008));
#41216=CARTESIAN_POINT('Ctrl Pts',(-3.87553067187514,-1.,1.10470536603287));
#41217=CARTESIAN_POINT('Ctrl Pts',(-3.86941120134849,-1.,1.10011198761195));
#41218=CARTESIAN_POINT('Ctrl Pts',(-3.86327241021247,-1.,1.09555606505013));
#41219=CARTESIAN_POINT('Ctrl Pts',(-3.85711487933931,-1.,1.09103825516294));
#41220=CARTESIAN_POINT('Ctrl Pts',(-3.85094025222713,-1.,1.08655950846384));
#41221=CARTESIAN_POINT('Ctrl Pts',(-3.8447504803063,-1.,1.08212087917991));
#41222=CARTESIAN_POINT('Ctrl Pts',(-3.83854714117491,-1.,1.07772335353858));
#41223=CARTESIAN_POINT('Ctrl Pts',(-3.83233071195144,-1.,1.07336766633459));
#41224=CARTESIAN_POINT('Ctrl Pts',(-3.82609989967276,-1.,1.06905413180359));
#41225=CARTESIAN_POINT('Ctrl Pts',(-3.81985083953012,-1.,1.0647824403893));
#41226=CARTESIAN_POINT('Ctrl Pts',(-3.8135786611749,-1.,1.06055206187299));
#41227=CARTESIAN_POINT('Ctrl Pts',(-3.80727913637791,-1.,1.05636266918644));
#41228=CARTESIAN_POINT('Ctrl Pts',(-3.80095039790681,-1.,1.05221457990016));
#41229=CARTESIAN_POINT('Ctrl Pts',(-3.79459440308786,-1.,1.04810913267639));
#41230=CARTESIAN_POINT('Ctrl Pts',(-3.78821910787179,-1.,1.04404924374422));
#41231=CARTESIAN_POINT('Ctrl Pts',(-3.7818353500817,-1.,1.04003862055798));
#41232=CARTESIAN_POINT('Ctrl Pts',(-3.77545283140427,-1.,1.03608074678008));
#41233=CARTESIAN_POINT('Ctrl Pts',(-3.76907609832516,-1.,1.03217786604919));
#41234=CARTESIAN_POINT('Ctrl Pts',(-3.76270122291245,-1.,1.02833014458184));
#41235=CARTESIAN_POINT('Ctrl Pts',(-3.75631037456224,-1.,1.02453429444668));
#41236=CARTESIAN_POINT('Ctrl Pts',(-3.74987777155873,-1.,1.02078510487439));
#41237=CARTESIAN_POINT('Ctrl Pts',(-3.74337942504993,-1.,1.01707794311088));
#41238=CARTESIAN_POINT('Ctrl Pts',(-3.73680245055747,-1.,1.01341114319906));
#41239=CARTESIAN_POINT('Ctrl Pts',(-3.73015276704407,-1.,1.00978798539491));
#41240=CARTESIAN_POINT('Ctrl Pts',(-3.72346803750544,-1.,1.00622000735696));
#41241=CARTESIAN_POINT('Ctrl Pts',(-3.71680667125047,-1.,1.00272423396802));
#41242=CARTESIAN_POINT('Ctrl Pts',(-3.7102243971387,-1.,0.999317260756344));
#41243=CARTESIAN_POINT('Ctrl Pts',(-3.70375282282107,-1.,0.996009819772431));
#41244=CARTESIAN_POINT('Ctrl Pts',(-3.69738123415696,-1.,0.992802218332103));
#41245=CARTESIAN_POINT('Ctrl Pts',(-3.69102682138955,-1.,0.989676715398858));
#41246=CARTESIAN_POINT('Ctrl Pts',(-3.6845531792623,-1.,0.986602639864285));
#41247=CARTESIAN_POINT('Ctrl Pts',(-3.67782408841876,-1.,0.983550791470864));
#41248=CARTESIAN_POINT('Ctrl Pts',(-3.67074983340444,-1.,0.980505922458494));
#41249=CARTESIAN_POINT('Ctrl Pts',(-3.66333049637403,-1.,0.977478312751416));
#41250=CARTESIAN_POINT('Ctrl Pts',(-3.6557157673487,-1.,0.974519971354138));
#41251=CARTESIAN_POINT('Ctrl Pts',(-3.64819756447072,-1.,0.971722122060277));
#41252=CARTESIAN_POINT('Ctrl Pts',(-3.64113946505393,-1.,0.969195124674829));
#41253=CARTESIAN_POINT('Ctrl Pts',(-3.6349212208096,-1.,0.967052554540877));
#41254=CARTESIAN_POINT('Ctrl Pts',(-3.62988252139998,-1.,0.965395153165716));
#41255=CARTESIAN_POINT('Ctrl Pts',(-3.62652618145252,-1.,0.964373850166081));
#41256=CARTESIAN_POINT('Ctrl Pts',(-3.62489305727516,-1.,0.963957782642589));
#41257=CARTESIAN_POINT('Ctrl Pts',(-3.62424461507455,-1.,0.963861297423579));
#41258=CARTESIAN_POINT('Ctrl Pts',(-3.62404828878375,-1.,0.963880158556713));
#41259=CARTESIAN_POINT('Ctrl Pts',(-3.62400312501199,-1.,0.963899035118985));
#41260=CARTESIAN_POINT('',(-3.66661143271648,-1.,0.786422660833743));
#41261=CARTESIAN_POINT('Origin',(0.,-1.,0.));
#41262=CARTESIAN_POINT('',(-4.13571194405636,-1.,0.732042837400619));
#41263=CARTESIAN_POINT('Ctrl Pts',(-3.66661143271648,-1.,0.786422660833743));
#41264=CARTESIAN_POINT('Ctrl Pts',(-3.66664310415236,-1.,0.786459983896781));
#41265=CARTESIAN_POINT('Ctrl Pts',(-3.66680946938396,-1.,0.78656591955989));
#41266=CARTESIAN_POINT('Ctrl Pts',(-3.66743103898844,-1.,0.786774337198499));
#41267=CARTESIAN_POINT('Ctrl Pts',(-3.66907505398769,-1.,0.787145041181588));
#41268=CARTESIAN_POINT('Ctrl Pts',(-3.672529236635,-1.,0.787758799995426));
#41269=CARTESIAN_POINT('Ctrl Pts',(-3.67777119516438,-1.,0.788569566220662));
#41270=CARTESIAN_POINT('Ctrl Pts',(-3.68428439784285,-1.,0.789483546065158));
#41271=CARTESIAN_POINT('Ctrl Pts',(-3.69172044327754,-1.,0.79043628498958));
#41272=CARTESIAN_POINT('Ctrl Pts',(-3.69968940808982,-1.,0.791356575696509));
#41273=CARTESIAN_POINT('Ctrl Pts',(-3.70781724021879,-1.,0.792177688845967));
#41274=CARTESIAN_POINT('Ctrl Pts',(-3.7158024239604,-1.,0.792848377370115));
#41275=CARTESIAN_POINT('Ctrl Pts',(-3.7234879729357,-1.,0.79334702378387));
#41276=CARTESIAN_POINT('Ctrl Pts',(-3.7308691469564,-1.,0.793682750269347));
#41277=CARTESIAN_POINT('Ctrl Pts',(-3.73803280541576,-1.,0.79388270093679));
#41278=CARTESIAN_POINT('Ctrl Pts',(-3.74511357728827,-1.,0.79398270045988));
#41279=CARTESIAN_POINT('Ctrl Pts',(-3.75224692493895,-1.,0.79401734737144));
#41280=CARTESIAN_POINT('Ctrl Pts',(-3.75951468666325,-1.,0.794008429135047));
#41281=CARTESIAN_POINT('Ctrl Pts',(-3.76692626931184,-1.,0.793961083689141));
#41282=CARTESIAN_POINT('Ctrl Pts',(-3.77444863801264,-1.,0.793870523787515));
#41283=CARTESIAN_POINT('Ctrl Pts',(-3.78202460377617,-1.,0.793726235781339));
#41284=CARTESIAN_POINT('Ctrl Pts',(-3.78959439439222,-1.,0.793516871680966));
#41285=CARTESIAN_POINT('Ctrl Pts',(-3.79711921389862,-1.,0.7932356129732));
#41286=CARTESIAN_POINT('Ctrl Pts',(-3.80459229925598,-1.,0.792882695234693));
#41287=CARTESIAN_POINT('Ctrl Pts',(-3.81202588694726,-1.,0.792462483517568));
#41288=CARTESIAN_POINT('Ctrl Pts',(-3.81944345442237,-1.,0.791981740718606));
#41289=CARTESIAN_POINT('Ctrl Pts',(-3.82687033899799,-1.,0.791447528662381));
#41290=CARTESIAN_POINT('Ctrl Pts',(-3.83432392054804,-1.,0.79086501270534));
#41291=CARTESIAN_POINT('Ctrl Pts',(-3.84180762342476,-1.,0.790236124191289));
#41292=CARTESIAN_POINT('Ctrl Pts',(-3.8493163780891,-1.,0.789560798155618));
#41293=CARTESIAN_POINT('Ctrl Pts',(-3.85683995872536,-1.,0.788837734090688));
#41294=CARTESIAN_POINT('Ctrl Pts',(-3.86436702561342,-1.,0.788065315093771));
#41295=CARTESIAN_POINT('Ctrl Pts',(-3.87188916600905,-1.,0.78724252761798));
#41296=CARTESIAN_POINT('Ctrl Pts',(-3.87940402818186,-1.,0.786369675812592));
#41297=CARTESIAN_POINT('Ctrl Pts',(-3.88691313167399,-1.,0.785447890340723));
#41298=CARTESIAN_POINT('Ctrl Pts',(-3.89442039235105,-1.,0.784478799358335));
#41299=CARTESIAN_POINT('Ctrl Pts',(-3.90193039043971,-1.,0.783464141529082));
#41300=CARTESIAN_POINT('Ctrl Pts',(-3.90944671004536,-1.,0.782405395622758));
#41301=CARTESIAN_POINT('Ctrl Pts',(-3.9169703605466,-1.,0.781303428618343));
#41302=CARTESIAN_POINT('Ctrl Pts',(-3.92450058323799,-1.,0.780158678615506));
#41303=CARTESIAN_POINT('Ctrl Pts',(-3.93203552473153,-1.,0.778971308134786));
#41304=CARTESIAN_POINT('Ctrl Pts',(-3.93957296768098,-1.,0.777741370568549));
#41305=CARTESIAN_POINT('Ctrl Pts',(-3.94711101619471,-1.,0.77646896669796));
#41306=CARTESIAN_POINT('Ctrl Pts',(-3.95464885452364,-1.,0.775154418039441));
#41307=CARTESIAN_POINT('Ctrl Pts',(-3.96218649639876,-1.,0.773798212026682));
#41308=CARTESIAN_POINT('Ctrl Pts',(-3.96972446532832,-1.,0.772400931772238));
#41309=CARTESIAN_POINT('Ctrl Pts',(-3.97726349165507,-1.,0.770963190030503));
#41310=CARTESIAN_POINT('Ctrl Pts',(-3.98480422348403,-1.,0.769485566245459));
#41311=CARTESIAN_POINT('Ctrl Pts',(-3.99234687880892,-1.,0.767968531377708));
#41312=CARTESIAN_POINT('Ctrl Pts',(-3.99989129179464,-1.,0.766412457135785));
#41313=CARTESIAN_POINT('Ctrl Pts',(-4.00743706791366,-1.,0.764817648784946));
#41314=CARTESIAN_POINT('Ctrl Pts',(-4.01498370680434,-1.,0.763184371182826));
#41315=CARTESIAN_POINT('Ctrl Pts',(-4.02253072741347,-1.,0.761512875859941));
#41316=CARTESIAN_POINT('Ctrl Pts',(-4.0300778195465,-1.,0.759803433244166));
#41317=CARTESIAN_POINT('Ctrl Pts',(-4.03762485803468,-1.,0.758056338885553));
#41318=CARTESIAN_POINT('Ctrl Pts',(-4.04517182654344,-1.,0.756271902370186));
#41319=CARTESIAN_POINT('Ctrl Pts',(-4.05271876688106,-1.,0.754450441816411));
#41320=CARTESIAN_POINT('Ctrl Pts',(-4.06026572221399,-1.,0.752592276482869));
#41321=CARTESIAN_POINT('Ctrl Pts',(-4.06781267241886,-1.,0.750697720483175));
#41322=CARTESIAN_POINT('Ctrl Pts',(-4.07535951055363,-1.,0.748767076679177));
#41323=CARTESIAN_POINT('Ctrl Pts',(-4.08290608094789,-1.,0.746800631490821));
#41324=CARTESIAN_POINT('Ctrl Pts',(-4.09045220253011,-1.,0.744798649705514));
#41325=CARTESIAN_POINT('Ctrl Pts',(-4.09799769702712,-1.,0.742761369690017));
#41326=CARTESIAN_POINT('Ctrl Pts',(-4.1055424175856,-1.,0.740688998555151));
#41327=CARTESIAN_POINT('Ctrl Pts',(-4.11308626953795,-1.,0.738581708229118));
#41328=CARTESIAN_POINT('Ctrl Pts',(-4.12062919626082,-1.,0.736439634335347));
#41329=CARTESIAN_POINT('Ctrl Pts',(-4.12666277572794,-1.,0.734698226767512));
#41330=CARTESIAN_POINT('Ctrl Pts',(-4.13118752796397,-1.,0.733376589325634));
#41331=CARTESIAN_POINT('Ctrl Pts',(-4.13420383737278,-1.,0.732488575135926));
#41332=CARTESIAN_POINT('Ctrl Pts',(-4.13571194405636,-1.,0.732042837400619));
#41333=CARTESIAN_POINT('',(-4.15950947128175,-1.,0.581791163835814));
#41334=CARTESIAN_POINT('',(-4.13571194405636,-1.,0.732042837400619));
#41335=CARTESIAN_POINT('',(-3.73017266276632,-1.,0.385112848332549));
#41336=CARTESIAN_POINT('Ctrl Pts',(-4.15950947128175,-1.,0.581791163835814));
#41337=CARTESIAN_POINT('Ctrl Pts',(-4.15821291712391,-1.,0.580901211462913));
#41338=CARTESIAN_POINT('Ctrl Pts',(-4.15561864787379,-1.,0.579124568912543));
#41339=CARTESIAN_POINT('Ctrl Pts',(-4.1517237611974,-1.,0.576469391673916));
#41340=CARTESIAN_POINT('Ctrl Pts',(-4.14652361065787,-1.,0.572948736066276));
#41341=CARTESIAN_POINT('Ctrl Pts',(-4.14001179828669,-1.,0.568580610187116));
#41342=CARTESIAN_POINT('Ctrl Pts',(-4.13348835726086,-1.,0.564245279535705));
#41343=CARTESIAN_POINT('Ctrl Pts',(-4.12695329951859,-1.,0.559942890594628));
#41344=CARTESIAN_POINT('Ctrl Pts',(-4.1204066619623,-1.,0.555673636130778));
#41345=CARTESIAN_POINT('Ctrl Pts',(-4.11384852025578,-1.,0.551437758498246));
#41346=CARTESIAN_POINT('Ctrl Pts',(-4.1072789702877,-1.,0.547235539486759));
#41347=CARTESIAN_POINT('Ctrl Pts',(-4.10069810244473,-1.,0.543067286878457));
#41348=CARTESIAN_POINT('Ctrl Pts',(-4.09410597627116,-1.,0.53893332117992));
#41349=CARTESIAN_POINT('Ctrl Pts',(-4.08750259988693,-1.,0.534833963476999));
#41350=CARTESIAN_POINT('Ctrl Pts',(-4.08088789536488,-1.,0.530769518728075));
#41351=CARTESIAN_POINT('Ctrl Pts',(-4.07426172299496,-1.,0.526740277226999));
#41352=CARTESIAN_POINT('Ctrl Pts',(-4.06762394471075,-1.,0.522746528602767));
#41353=CARTESIAN_POINT('Ctrl Pts',(-4.06097448037934,-1.,0.518788572336809));
#41354=CARTESIAN_POINT('Ctrl Pts',(-4.05431335771261,-1.,0.514866728193104));
#41355=CARTESIAN_POINT('Ctrl Pts',(-4.04764078815591,-1.,0.510981349219173));
#41356=CARTESIAN_POINT('Ctrl Pts',(-4.04095715149074,-1.,0.507132823288361));
#41357=CARTESIAN_POINT('Ctrl Pts',(-4.0342628417439,-1.,0.503321556915513));
#41358=CARTESIAN_POINT('Ctrl Pts',(-4.0275581398015,-1.,0.499547962340889));
#41359=CARTESIAN_POINT('Ctrl Pts',(-4.02084308851813,-1.,0.495812444326223));
#41360=CARTESIAN_POINT('Ctrl Pts',(-4.01411733503486,-1.,0.49211538341793));
#41361=CARTESIAN_POINT('Ctrl Pts',(-4.0073800839092,-1.,0.48845713042453));
#41362=CARTESIAN_POINT('Ctrl Pts',(-4.00063045119234,-1.,0.484838042421754));
#41363=CARTESIAN_POINT('Ctrl Pts',(-3.99386775880655,-1.,0.481258512209638));
#41364=CARTESIAN_POINT('Ctrl Pts',(-3.98709184306743,-1.,0.477718999122033));
#41365=CARTESIAN_POINT('Ctrl Pts',(-3.9803033804443,-1.,0.474220061019542));
#41366=CARTESIAN_POINT('Ctrl Pts',(-3.97350414289415,-1.,0.470762379613477));
#41367=CARTESIAN_POINT('Ctrl Pts',(-3.96669622273946,-1.,0.467346690880671));
#41368=CARTESIAN_POINT('Ctrl Pts',(-3.95988133243543,-1.,0.463973722115744));
#41369=CARTESIAN_POINT('Ctrl Pts',(-3.95306005817363,-1.,0.460644124429119));
#41370=CARTESIAN_POINT('Ctrl Pts',(-3.94623117206675,-1.,0.457358410451674));
#41371=CARTESIAN_POINT('Ctrl Pts',(-3.93939080846298,-1.,0.454116879027576));
#41372=CARTESIAN_POINT('Ctrl Pts',(-3.93253407403128,-1.,0.450919768356347));
#41373=CARTESIAN_POINT('Ctrl Pts',(-3.92565674143424,-1.,0.447767416837296));
#41374=CARTESIAN_POINT('Ctrl Pts',(-3.91875701610721,-1.,0.444660430230592));
#41375=CARTESIAN_POINT('Ctrl Pts',(-3.91183704069146,-1.,0.441599824524047));
#41376=CARTESIAN_POINT('Ctrl Pts',(-3.90490512938546,-1.,0.438587235458233));
#41377=CARTESIAN_POINT('Ctrl Pts',(-3.8979725665544,-1.,0.435624629433505));
#41378=CARTESIAN_POINT('Ctrl Pts',(-3.89104947940592,-1.,0.432713929544439));
#41379=CARTESIAN_POINT('Ctrl Pts',(-3.88414070943334,-1.,0.429856640579733));
#41380=CARTESIAN_POINT('Ctrl Pts',(-3.87724240306609,-1.,0.427053541173469));
#41381=CARTESIAN_POINT('Ctrl Pts',(-3.87033643487882,-1.,0.424304173195142));
#41382=CARTESIAN_POINT('Ctrl Pts',(-3.86339652542749,-1.,0.421607423177575));
#41383=CARTESIAN_POINT('Ctrl Pts',(-3.85639825648031,-1.,0.418962468086809));
#41384=CARTESIAN_POINT('Ctrl Pts',(-3.8493286415751,-1.,0.41636967805292));
#41385=CARTESIAN_POINT('Ctrl Pts',(-3.84219403994742,-1.,0.413831367016726));
#41386=CARTESIAN_POINT('Ctrl Pts',(-3.83503345578645,-1.,0.411353038798459));
#41387=CARTESIAN_POINT('Ctrl Pts',(-3.82790724256397,-1.,0.408942371447377));
#41388=CARTESIAN_POINT('Ctrl Pts',(-3.82087303913741,-1.,0.406607038258906));
#41389=CARTESIAN_POINT('Ctrl Pts',(-3.81396374287762,-1.,0.404352694628236));
#41390=CARTESIAN_POINT('Ctrl Pts',(-3.80716881962763,-1.,0.402181320148474));
#41391=CARTESIAN_POINT('Ctrl Pts',(-3.80040370384659,-1.,0.400088346504726));
#41392=CARTESIAN_POINT('Ctrl Pts',(-3.79352887163457,-1.,0.398064818684158));
#41393=CARTESIAN_POINT('Ctrl Pts',(-3.78640521279479,-1.,0.396103205335028));
#41394=CARTESIAN_POINT('Ctrl Pts',(-3.77894173114368,-1.,0.394202481011595));
#41395=CARTESIAN_POINT('Ctrl Pts',(-3.77114011595892,-1.,0.392372786223346));
#41396=CARTESIAN_POINT('Ctrl Pts',(-3.76315635032993,-1.,0.390642072979259));
#41397=CARTESIAN_POINT('Ctrl Pts',(-3.75529302894757,-1.,0.389054775898251));
#41398=CARTESIAN_POINT('Ctrl Pts',(-3.74792651696269,-1.,0.387663020050396));
#41399=CARTESIAN_POINT('Ctrl Pts',(-3.74144965781088,-1.,0.386519576222035));
#41400=CARTESIAN_POINT('Ctrl Pts',(-3.73621371845475,-1.,0.385670806454744));
#41401=CARTESIAN_POINT('Ctrl Pts',(-3.73273893363318,-1.,0.385187124633964));
#41402=CARTESIAN_POINT('Ctrl Pts',(-3.73106082862399,-1.,0.385031656499141));
#41403=CARTESIAN_POINT('Ctrl Pts',(-3.73040527620929,-1.,0.385037797882046));
#41404=CARTESIAN_POINT('Ctrl Pts',(-3.73021431755218,-1.,0.385087139001609));
#41405=CARTESIAN_POINT('Ctrl Pts',(-3.73017266276632,-1.,0.385112848332549));
#41406=CARTESIAN_POINT('',(-3.74449296982994,-1.,0.203156094897895));
#41407=CARTESIAN_POINT('Origin',(0.,-1.,0.));
#41408=CARTESIAN_POINT('',(-4.19931119685982,-1.,0.0760622897878236));
#41409=CARTESIAN_POINT('Ctrl Pts',(-3.74449296982994,-1.,0.203156094897895));
#41410=CARTESIAN_POINT('Ctrl Pts',(-3.74453008995129,-1.,0.203188003947965));
#41411=CARTESIAN_POINT('Ctrl Pts',(-3.74471097893961,-1.,0.203266610111264));
#41412=CARTESIAN_POINT('Ctrl Pts',(-3.74535749969262,-1.,0.203375226874331));
#41413=CARTESIAN_POINT('Ctrl Pts',(-3.74703926501843,-1.,0.203484186269314));
#41414=CARTESIAN_POINT('Ctrl Pts',(-3.75054693397716,-1.,0.203550035479097));
#41415=CARTESIAN_POINT('Ctrl Pts',(-3.75585118707924,-1.,0.203530796848403));
#41416=CARTESIAN_POINT('Ctrl Pts',(-3.76242717937273,-1.,0.203414634707646));
#41417=CARTESIAN_POINT('Ctrl Pts',(-3.76992071595267,-1.,0.203192390045337));
#41418=CARTESIAN_POINT('Ctrl Pts',(-3.77793553476879,-1.,0.202854729699196));
#41419=CARTESIAN_POINT('Ctrl Pts',(-3.78609175019317,-1.,0.202394260512193));
#41420=CARTESIAN_POINT('Ctrl Pts',(-3.79408354187274,-1.,0.201807533800799));
#41421=CARTESIAN_POINT('Ctrl Pts',(-3.80175247447171,-1.,0.201097756307252));
#41422=CARTESIAN_POINT('Ctrl Pts',(-3.80909529318501,-1.,0.20027467943329));
#41423=CARTESIAN_POINT('Ctrl Pts',(-3.81620203429702,-1.,0.199351525297396));
#41424=CARTESIAN_POINT('Ctrl Pts',(-3.82321127348981,-1.,0.19834261690047));
#41425=CARTESIAN_POINT('Ctrl Pts',(-3.83026221776488,-1.,0.197260935827375));
#41426=CARTESIAN_POINT('Ctrl Pts',(-3.83743910616265,-1.,0.196115198971889));
#41427=CARTESIAN_POINT('Ctrl Pts',(-3.84475203347052,-1.,0.194909009460254));
#41428=CARTESIAN_POINT('Ctrl Pts',(-3.85216762264019,-1.,0.193642806777747));
#41429=CARTESIAN_POINT('Ctrl Pts',(-3.85962774407652,-1.,0.192315153044979));
#41430=CARTESIAN_POINT('Ctrl Pts',(-3.8670715862477,-1.,0.190924190418613));
#41431=CARTESIAN_POINT('Ctrl Pts',(-3.87445976418377,-1.,0.189469253358254));
#41432=CARTESIAN_POINT('Ctrl Pts',(-3.88178563496187,-1.,0.187951632512663));
#41433=CARTESIAN_POINT('Ctrl Pts',(-3.88906196725817,-1.,0.186373724985263));
#41434=CARTESIAN_POINT('Ctrl Pts',(-3.89631300742633,-1.,0.184738537728035));
#41435=CARTESIAN_POINT('Ctrl Pts',(-3.90356488555138,-1.,0.183049081993193));
#41436=CARTESIAN_POINT('Ctrl Pts',(-3.91083557557193,-1.,0.181307740731796));
#41437=CARTESIAN_POINT('Ctrl Pts',(-3.91812876180948,-1.,0.179515885822894));
#41438=CARTESIAN_POINT('Ctrl Pts',(-3.92543942697672,-1.,0.177674246152328));
#41439=CARTESIAN_POINT('Ctrl Pts',(-3.93275726771049,-1.,0.175783136893872));
#41440=CARTESIAN_POINT('Ctrl Pts',(-3.94007083096214,-1.,0.173842734974607));
#41441=CARTESIAN_POINT('Ctrl Pts',(-3.94737164900861,-1.,0.171853355369233));
#41442=CARTESIAN_POINT('Ctrl Pts',(-3.95465744665263,-1.,0.16981566637413));
#41443=CARTESIAN_POINT('Ctrl Pts',(-3.96192990160296,-1.,0.167730547023312));
#41444=CARTESIAN_POINT('Ctrl Pts',(-3.9691931362141,-1.,0.165598992851097));
#41445=CARTESIAN_POINT('Ctrl Pts',(-3.97645194630944,-1.,0.163422004609999));
#41446=CARTESIAN_POINT('Ctrl Pts',(-3.98371010319866,-1.,0.161200482186087));
#41447=CARTESIAN_POINT('Ctrl Pts',(-3.99096873945862,-1.,0.158935123982796));
#41448=CARTESIAN_POINT('Ctrl Pts',(-3.99822717425869,-1.,0.156626481393735));
#41449=CARTESIAN_POINT('Ctrl Pts',(-4.00548360245297,-1.,0.15427500487231));
#41450=CARTESIAN_POINT('Ctrl Pts',(-4.01273584234684,-1.,0.151881094022909));
#41451=CARTESIAN_POINT('Ctrl Pts',(-4.01998203715588,-1.,0.149445144968707));
#41452=CARTESIAN_POINT('Ctrl Pts',(-4.02722143147048,-1.,0.146967602878998));
#41453=CARTESIAN_POINT('Ctrl Pts',(-4.03445411510403,-1.,0.144448947038352));
#41454=CARTESIAN_POINT('Ctrl Pts',(-4.04168069633842,-1.,0.141889671485508));
#41455=CARTESIAN_POINT('Ctrl Pts',(-4.04890199238056,-1.,0.139290267180059));
#41456=CARTESIAN_POINT('Ctrl Pts',(-4.05611873400122,-1.,0.136651205046111));
#41457=CARTESIAN_POINT('Ctrl Pts',(-4.06333121018476,-1.,0.133972916144225));
#41458=CARTESIAN_POINT('Ctrl Pts',(-4.07053931528579,-1.,0.131255793548914));
#41459=CARTESIAN_POINT('Ctrl Pts',(-4.07774270738809,-1.,0.128500200484814));
#41460=CARTESIAN_POINT('Ctrl Pts',(-4.08494093372315,-1.,0.125706476822529));
#41461=CARTESIAN_POINT('Ctrl Pts',(-4.09213355850836,-1.,0.122874946249119));
#41462=CARTESIAN_POINT('Ctrl Pts',(-4.09932031767243,-1.,0.120005924388162));
#41463=CARTESIAN_POINT('Ctrl Pts',(-4.10650113382187,-1.,0.117099722731704));
#41464=CARTESIAN_POINT('Ctrl Pts',(-4.11367603925313,-1.,0.114156649609601));
#41465=CARTESIAN_POINT('Ctrl Pts',(-4.12084512502444,-1.,0.111177012683377));
#41466=CARTESIAN_POINT('Ctrl Pts',(-4.12800848371386,-1.,0.10816112052835));
#41467=CARTESIAN_POINT('Ctrl Pts',(-4.13516614458396,-1.,0.105109286538864));
#41468=CARTESIAN_POINT('Ctrl Pts',(-4.14231804938737,-1.,0.102021826577454));
#41469=CARTESIAN_POINT('Ctrl Pts',(-4.1494640891762,-1.,0.0988990478899811));
#41470=CARTESIAN_POINT('Ctrl Pts',(-4.15660412653006,-1.,0.0957412403297067));
#41471=CARTESIAN_POINT('Ctrl Pts',(-4.16373802265942,-1.,0.092548667216769));
#41472=CARTESIAN_POINT('Ctrl Pts',(-4.17086566491823,-1.,0.0893215560850327));
#41473=CARTESIAN_POINT('Ctrl Pts',(-4.17798698669991,-1.,0.0860600915552515));
#41474=CARTESIAN_POINT('Ctrl Pts',(-4.1851019532944,-1.,0.082764416438951));
#41475=CARTESIAN_POINT('Ctrl Pts',(-4.19078883322483,-1.,0.0801005887117603));
#41476=CARTESIAN_POINT('Ctrl Pts',(-4.19505112860624,-1.,0.0780873956244402));
#41477=CARTESIAN_POINT('Ctrl Pts',(-4.19789138621624,-1.,0.0767384596142195));
#41478=CARTESIAN_POINT('Ctrl Pts',(-4.19931119685982,-1.,0.0760622897878236));
#41479=CARTESIAN_POINT('',(-4.19931119685982,-1.,-0.0760622897878246));
#41480=CARTESIAN_POINT('',(-4.19931119685982,-1.,0.0760622897878236));
#41481=CARTESIAN_POINT('',(-3.74449296983004,-1.,-0.203156094896101));
#41482=CARTESIAN_POINT('Ctrl Pts',(-4.19931119685982,-1.,-0.0760622897878246));
#41483=CARTESIAN_POINT('Ctrl Pts',(-4.1978913862118,-1.,-0.0767384596141464));
#41484=CARTESIAN_POINT('Ctrl Pts',(-4.19505112859416,-1.,-0.0780873956242397));
#41485=CARTESIAN_POINT('Ctrl Pts',(-4.19078883320504,-1.,-0.080100588711432));
#41486=CARTESIAN_POINT('Ctrl Pts',(-4.18510195327123,-1.,-0.0827644164385679));
#41487=CARTESIAN_POINT('Ctrl Pts',(-4.17798698668094,-1.,-0.0860600915549397));
#41488=CARTESIAN_POINT('Ctrl Pts',(-4.17086566490794,-1.,-0.0893215560848649));
#41489=CARTESIAN_POINT('Ctrl Pts',(-4.16373802265839,-1.,-0.0925486672167531));
#41490=CARTESIAN_POINT('Ctrl Pts',(-4.15660412653577,-1.,-0.0957412403298007));
#41491=CARTESIAN_POINT('Ctrl Pts',(-4.14946408918485,-1.,-0.0988990478901226));
#41492=CARTESIAN_POINT('Ctrl Pts',(-4.14231804939538,-1.,-0.102021826577584));
#41493=CARTESIAN_POINT('Ctrl Pts',(-4.13516614458895,-1.,-0.105109286538945));
#41494=CARTESIAN_POINT('Ctrl Pts',(-4.12800848371504,-1.,-0.108161120528369));
#41495=CARTESIAN_POINT('Ctrl Pts',(-4.1208451250225,-1.,-0.111177012683347));
#41496=CARTESIAN_POINT('Ctrl Pts',(-4.11367603924961,-1.,-0.114156649609546));
#41497=CARTESIAN_POINT('Ctrl Pts',(-4.10650113381833,-1.,-0.117099722731648));
#41498=CARTESIAN_POINT('Ctrl Pts',(-4.09932031767002,-1.,-0.120005924388124));
#41499=CARTESIAN_POINT('Ctrl Pts',(-4.09213355850756,-1.,-0.122874946249107));
#41500=CARTESIAN_POINT('Ctrl Pts',(-4.08494093372377,-1.,-0.12570647682254));
#41501=CARTESIAN_POINT('Ctrl Pts',(-4.07774270738954,-1.,-0.128500200484838));
#41502=CARTESIAN_POINT('Ctrl Pts',(-4.0705393152874,-1.,-0.13125579354894));
#41503=CARTESIAN_POINT('Ctrl Pts',(-4.06333121018596,-1.,-0.133972916144245));
#41504=CARTESIAN_POINT('Ctrl Pts',(-4.05611873400172,-1.,-0.136651205046119));
#41505=CARTESIAN_POINT('Ctrl Pts',(-4.04890199238036,-1.,-0.139290267180057));
#41506=CARTESIAN_POINT('Ctrl Pts',(-4.04168069633781,-1.,-0.1418896714855));
#41507=CARTESIAN_POINT('Ctrl Pts',(-4.03445411510333,-1.,-0.144448947038345));
#41508=CARTESIAN_POINT('Ctrl Pts',(-4.02722143146994,-1.,-0.146967602878994));
#41509=CARTESIAN_POINT('Ctrl Pts',(-4.01998203715564,-1.,-0.149445144968707));
#41510=CARTESIAN_POINT('Ctrl Pts',(-4.01273584234689,-1.,-0.151881094022911));
#41511=CARTESIAN_POINT('Ctrl Pts',(-4.00548360245319,-1.,-0.154275004872311));
#41512=CARTESIAN_POINT('Ctrl Pts',(-3.99822717425893,-1.,-0.156626481393734));
#41513=CARTESIAN_POINT('Ctrl Pts',(-3.99096873945878,-1.,-0.158935123982793));
#41514=CARTESIAN_POINT('Ctrl Pts',(-3.98371010319872,-1.,-0.161200482186085));
#41515=CARTESIAN_POINT('Ctrl Pts',(-3.97645194630943,-1.,-0.163422004609999));
#41516=CARTESIAN_POINT('Ctrl Pts',(-3.96919313621407,-1.,-0.165598992851102));
#41517=CARTESIAN_POINT('Ctrl Pts',(-3.96192990160296,-1.,-0.167730547023319));
#41518=CARTESIAN_POINT('Ctrl Pts',(-3.95465744665268,-1.,-0.169815666374139));
#41519=CARTESIAN_POINT('Ctrl Pts',(-3.94737164900868,-1.,-0.17185335536924));
#41520=CARTESIAN_POINT('Ctrl Pts',(-3.94007083096217,-1.,-0.17384273497461));
#41521=CARTESIAN_POINT('Ctrl Pts',(-3.93275726771042,-1.,-0.175783136893868));
#41522=CARTESIAN_POINT('Ctrl Pts',(-3.92543942697655,-1.,-0.177674246152317));
#41523=CARTESIAN_POINT('Ctrl Pts',(-3.91812876180926,-1.,-0.179515885822882));
#41524=CARTESIAN_POINT('Ctrl Pts',(-3.91083557557175,-1.,-0.181307740731786));
#41525=CARTESIAN_POINT('Ctrl Pts',(-3.90356488555132,-1.,-0.183049081993191));
#41526=CARTESIAN_POINT('Ctrl Pts',(-3.89631300742646,-1.,-0.184738537728043));
#41527=CARTESIAN_POINT('Ctrl Pts',(-3.88906196725848,-1.,-0.18637372498528));
#41528=CARTESIAN_POINT('Ctrl Pts',(-3.88178563496228,-1.,-0.187951632512685));
#41529=CARTESIAN_POINT('Ctrl Pts',(-3.87445976418412,-1.,-0.189469253358272));
#41530=CARTESIAN_POINT('Ctrl Pts',(-3.86707158624783,-1.,-0.19092419041862));
#41531=CARTESIAN_POINT('Ctrl Pts',(-3.85962774407633,-1.,-0.192315153044971));
#41532=CARTESIAN_POINT('Ctrl Pts',(-3.85216762263966,-1.,-0.193642806777723));
#41533=CARTESIAN_POINT('Ctrl Pts',(-3.84475203346977,-1.,-0.194909009460221));
#41534=CARTESIAN_POINT('Ctrl Pts',(-3.83743910616195,-1.,-0.196115198971859));
#41535=CARTESIAN_POINT('Ctrl Pts',(-3.83026221776456,-1.,-0.197260935827361));
#41536=CARTESIAN_POINT('Ctrl Pts',(-3.82321127349016,-1.,-0.198342616900486));
#41537=CARTESIAN_POINT('Ctrl Pts',(-3.81620203429815,-1.,-0.199351525297447));
#41538=CARTESIAN_POINT('Ctrl Pts',(-3.80909529318669,-1.,-0.200274679433364));
#41539=CARTESIAN_POINT('Ctrl Pts',(-3.80175247447337,-1.,-0.201097756307326));
#41540=CARTESIAN_POINT('Ctrl Pts',(-3.7940835418736,-1.,-0.201807533800837));
#41541=CARTESIAN_POINT('Ctrl Pts',(-3.78609175019242,-1.,-0.20239426051216));
#41542=CARTESIAN_POINT('Ctrl Pts',(-3.77793553476614,-1.,-0.202854729699081));
#41543=CARTESIAN_POINT('Ctrl Pts',(-3.7699207159487,-1.,-0.203192390045164));
#41544=CARTESIAN_POINT('Ctrl Pts',(-3.76242717936885,-1.,-0.203414634707478));
#41545=CARTESIAN_POINT('Ctrl Pts',(-3.75585118707734,-1.,-0.203530796848322));
#41546=CARTESIAN_POINT('Ctrl Pts',(-3.75054693397875,-1.,-0.203550035479166));
#41547=CARTESIAN_POINT('Ctrl Pts',(-3.74703926501752,-1.,-0.203484186269415));
#41548=CARTESIAN_POINT('Ctrl Pts',(-3.74535749969115,-1.,-0.203375226874121));
#41549=CARTESIAN_POINT('Ctrl Pts',(-3.74471097893845,-1.,-0.203266610110531));
#41550=CARTESIAN_POINT('Ctrl Pts',(-3.74453008995092,-1.,-0.203188003946657));
#41551=CARTESIAN_POINT('Ctrl Pts',(-3.74449296983004,-1.,-0.203156094896101));
#41552=CARTESIAN_POINT('',(-3.73017266276651,-1.,-0.385112848330762));
#41553=CARTESIAN_POINT('Origin',(0.,-1.,0.));
#41554=CARTESIAN_POINT('',(-4.15950947128175,-1.,-0.581791163835815));
#41555=CARTESIAN_POINT('Ctrl Pts',(-3.73017266276651,-1.,-0.385112848330762));
#41556=CARTESIAN_POINT('Ctrl Pts',(-3.73021431755274,-1.,-0.385087139000374));
#41557=CARTESIAN_POINT('Ctrl Pts',(-3.73040527621055,-1.,-0.385037797881504));
#41558=CARTESIAN_POINT('Ctrl Pts',(-3.73106082862548,-1.,-0.385031656499164));
#41559=CARTESIAN_POINT('Ctrl Pts',(-3.73273893363406,-1.,-0.385187124634206));
#41560=CARTESIAN_POINT('Ctrl Pts',(-3.73621371845318,-1.,-0.385670806454566));
#41561=CARTESIAN_POINT('Ctrl Pts',(-3.74144965781276,-1.,-0.386519576222251));
#41562=CARTESIAN_POINT('Ctrl Pts',(-3.74792651696654,-1.,-0.387663020050836));
#41563=CARTESIAN_POINT('Ctrl Pts',(-3.75529302895152,-1.,-0.389054775898702));
#41564=CARTESIAN_POINT('Ctrl Pts',(-3.76315635033257,-1.,-0.39064207297956));
#41565=CARTESIAN_POINT('Ctrl Pts',(-3.77114011595967,-1.,-0.392372786223432));
#41566=CARTESIAN_POINT('Ctrl Pts',(-3.77894173114283,-1.,-0.394202481011499));
#41567=CARTESIAN_POINT('Ctrl Pts',(-3.78640521279313,-1.,-0.396103205334841));
#41568=CARTESIAN_POINT('Ctrl Pts',(-3.7935288716329,-1.,-0.398064818683969));
#41569=CARTESIAN_POINT('Ctrl Pts',(-3.80040370384546,-1.,-0.4000883465046));
#41570=CARTESIAN_POINT('Ctrl Pts',(-3.80716881962728,-1.,-0.402181320148436));
#41571=CARTESIAN_POINT('Ctrl Pts',(-3.81396374287793,-1.,-0.404352694628273));
#41572=CARTESIAN_POINT('Ctrl Pts',(-3.8208730391381,-1.,-0.406607038258985));
#41573=CARTESIAN_POINT('Ctrl Pts',(-3.82790724256471,-1.,-0.40894237144746));
#41574=CARTESIAN_POINT('Ctrl Pts',(-3.83503345578698,-1.,-0.411353038798518));
#41575=CARTESIAN_POINT('Ctrl Pts',(-3.84219403994762,-1.,-0.413831367016748));
#41576=CARTESIAN_POINT('Ctrl Pts',(-3.84932864157497,-1.,-0.416369678052907));
#41577=CARTESIAN_POINT('Ctrl Pts',(-3.85639825647996,-1.,-0.418962468086773));
#41578=CARTESIAN_POINT('Ctrl Pts',(-3.86339652542709,-1.,-0.421607423177534));
#41579=CARTESIAN_POINT('Ctrl Pts',(-3.87033643487851,-1.,-0.424304173195111));
#41580=CARTESIAN_POINT('Ctrl Pts',(-3.87724240306597,-1.,-0.427053541173457));
#41581=CARTESIAN_POINT('Ctrl Pts',(-3.88414070943341,-1.,-0.429856640579741));
#41582=CARTESIAN_POINT('Ctrl Pts',(-3.89104947940611,-1.,-0.432713929544458));
#41583=CARTESIAN_POINT('Ctrl Pts',(-3.89797256655462,-1.,-0.435624629433527));
#41584=CARTESIAN_POINT('Ctrl Pts',(-3.90490512938563,-1.,-0.438587235458249));
#41585=CARTESIAN_POINT('Ctrl Pts',(-3.91183704069153,-1.,-0.441599824524054));
#41586=CARTESIAN_POINT('Ctrl Pts',(-3.91875701610719,-1.,-0.444660430230591));
#41587=CARTESIAN_POINT('Ctrl Pts',(-3.92565674143416,-1.,-0.447767416837292));
#41588=CARTESIAN_POINT('Ctrl Pts',(-3.93253407403123,-1.,-0.450919768356348));
#41589=CARTESIAN_POINT('Ctrl Pts',(-3.93939080846298,-1.,-0.454116879027584));
#41590=CARTESIAN_POINT('Ctrl Pts',(-3.94623117206678,-1.,-0.457358410451683));
#41591=CARTESIAN_POINT('Ctrl Pts',(-3.95306005817364,-1.,-0.460644124429121));
#41592=CARTESIAN_POINT('Ctrl Pts',(-3.95988133243538,-1.,-0.463973722115733));
#41593=CARTESIAN_POINT('Ctrl Pts',(-3.9666962227393,-1.,-0.467346690880643));
#41594=CARTESIAN_POINT('Ctrl Pts',(-3.97350414289392,-1.,-0.470762379613439));
#41595=CARTESIAN_POINT('Ctrl Pts',(-3.98030338044409,-1.,-0.47422006101951));
#41596=CARTESIAN_POINT('Ctrl Pts',(-3.98709184306738,-1.,-0.477718999122027));
#41597=CARTESIAN_POINT('Ctrl Pts',(-3.99386775880679,-1.,-0.481258512209675));
#41598=CARTESIAN_POINT('Ctrl Pts',(-4.00063045119288,-1.,-0.484838042421835));
#41599=CARTESIAN_POINT('Ctrl Pts',(-4.0073800839099,-1.,-0.488457130424633));
#41600=CARTESIAN_POINT('Ctrl Pts',(-4.01411733503546,-1.,-0.492115383418018));
#41601=CARTESIAN_POINT('Ctrl Pts',(-4.02084308851832,-1.,-0.495812444326251));
#41602=CARTESIAN_POINT('Ctrl Pts',(-4.02755813980101,-1.,-0.499547962340821));
#41603=CARTESIAN_POINT('Ctrl Pts',(-4.03426284174272,-1.,-0.503321556915346));
#41604=CARTESIAN_POINT('Ctrl Pts',(-4.04095715148915,-1.,-0.507132823288136));
#41605=CARTESIAN_POINT('Ctrl Pts',(-4.04764078815447,-1.,-0.51098134921897));
#41606=CARTESIAN_POINT('Ctrl Pts',(-4.05431335771199,-1.,-0.514866728193017));
#41607=CARTESIAN_POINT('Ctrl Pts',(-4.06097448038013,-1.,-0.518788572336923));
#41608=CARTESIAN_POINT('Ctrl Pts',(-4.06762394471314,-1.,-0.522746528603107));
#41609=CARTESIAN_POINT('Ctrl Pts',(-4.07426172299847,-1.,-0.526740277227498));
#41610=CARTESIAN_POINT('Ctrl Pts',(-4.08088789536836,-1.,-0.530769518728571));
#41611=CARTESIAN_POINT('Ctrl Pts',(-4.08750259988885,-1.,-0.534833963477273));
#41612=CARTESIAN_POINT('Ctrl Pts',(-4.09410597627,-1.,-0.538933321179756));
#41613=CARTESIAN_POINT('Ctrl Pts',(-4.10069810243979,-1.,-0.543067286877757));
#41614=CARTESIAN_POINT('Ctrl Pts',(-4.10727897027977,-1.,-0.547235539485637));
#41615=CARTESIAN_POINT('Ctrl Pts',(-4.11384852024721,-1.,-0.551437758497032));
#41616=CARTESIAN_POINT('Ctrl Pts',(-4.12040666195664,-1.,-0.555673636129977));
#41617=CARTESIAN_POINT('Ctrl Pts',(-4.12695329951961,-1.,-0.559942890594773));
#41618=CARTESIAN_POINT('Ctrl Pts',(-4.13348835727104,-1.,-0.564245279537148));
#41619=CARTESIAN_POINT('Ctrl Pts',(-4.14001179830547,-1.,-0.568580610189774));
#41620=CARTESIAN_POINT('Ctrl Pts',(-4.14652361068081,-1.,-0.572948736069522));
#41621=CARTESIAN_POINT('Ctrl Pts',(-4.151723761217,-1.,-0.576469391676688));
#41622=CARTESIAN_POINT('Ctrl Pts',(-4.15561864788576,-1.,-0.579124568914235));
#41623=CARTESIAN_POINT('Ctrl Pts',(-4.1582129171283,-1.,-0.580901211463535));
#41624=CARTESIAN_POINT('Ctrl Pts',(-4.15950947128175,-1.,-0.581791163835815));
#41625=CARTESIAN_POINT('',(-4.13571194405636,-1.,-0.73204283740062));
#41626=CARTESIAN_POINT('',(-4.15950947128175,-1.,-0.581791163835815));
#41627=CARTESIAN_POINT('',(-3.66661143271685,-1.,-0.786422660831985));
#41628=CARTESIAN_POINT('Ctrl Pts',(-4.13571194405636,-1.,-0.73204283740062));
#41629=CARTESIAN_POINT('Ctrl Pts',(-4.1342038373684,-1.,-0.732488575135159));
#41630=CARTESIAN_POINT('Ctrl Pts',(-4.13118752795207,-1.,-0.733376589323546));
#41631=CARTESIAN_POINT('Ctrl Pts',(-4.12666277570844,-1.,-0.734698226764092));
#41632=CARTESIAN_POINT('Ctrl Pts',(-4.120629196238,-1.,-0.736439634331345));
#41633=CARTESIAN_POINT('Ctrl Pts',(-4.11308626951927,-1.,-0.738581708225844));
#41634=CARTESIAN_POINT('Ctrl Pts',(-4.10554241757547,-1.,-0.740688998553377));
#41635=CARTESIAN_POINT('Ctrl Pts',(-4.09799769702611,-1.,-0.742761369689841));
#41636=CARTESIAN_POINT('Ctrl Pts',(-4.09045220253573,-1.,-0.7447986497065));
#41637=CARTESIAN_POINT('Ctrl Pts',(-4.08290608095642,-1.,-0.746800631492315));
#41638=CARTESIAN_POINT('Ctrl Pts',(-4.07535951056152,-1.,-0.748767076680557));
#41639=CARTESIAN_POINT('Ctrl Pts',(-4.06781267242378,-1.,-0.750697720484036));
#41640=CARTESIAN_POINT('Ctrl Pts',(-4.06026572221515,-1.,-0.752592276483072));
#41641=CARTESIAN_POINT('Ctrl Pts',(-4.05271876687915,-1.,-0.754450441816078));
#41642=CARTESIAN_POINT('Ctrl Pts',(-4.04517182653997,-1.,-0.756271902369581));
#41643=CARTESIAN_POINT('Ctrl Pts',(-4.03762485803119,-1.,-0.758056338884944));
#41644=CARTESIAN_POINT('Ctrl Pts',(-4.03007781954412,-1.,-0.759803433243752));
#41645=CARTESIAN_POINT('Ctrl Pts',(-4.02253072741268,-1.,-0.761512875859804));
#41646=CARTESIAN_POINT('Ctrl Pts',(-4.01498370680496,-1.,-0.763184371182935));
#41647=CARTESIAN_POINT('Ctrl Pts',(-4.00743706791509,-1.,-0.764817648785197));
#41648=CARTESIAN_POINT('Ctrl Pts',(-3.99989129179622,-1.,-0.766412457136064));
#41649=CARTESIAN_POINT('Ctrl Pts',(-3.9923468788101,-1.,-0.767968531377915));
#41650=CARTESIAN_POINT('Ctrl Pts',(-3.98480422348451,-1.,-0.769485566245544));
#41651=CARTESIAN_POINT('Ctrl Pts',(-3.97726349165488,-1.,-0.770963190030471));
#41652=CARTESIAN_POINT('Ctrl Pts',(-3.96972446532772,-1.,-0.772400931772136));
#41653=CARTESIAN_POINT('Ctrl Pts',(-3.96218649639807,-1.,-0.773798212026565));
#41654=CARTESIAN_POINT('Ctrl Pts',(-3.9546488545231,-1.,-0.775154418039351));
#41655=CARTESIAN_POINT('Ctrl Pts',(-3.94711101619447,-1.,-0.776468966697921));
#41656=CARTESIAN_POINT('Ctrl Pts',(-3.93957296768103,-1.,-0.777741370568558));
#41657=CARTESIAN_POINT('Ctrl Pts',(-3.93203552473174,-1.,-0.778971308134821));
#41658=CARTESIAN_POINT('Ctrl Pts',(-3.92450058323823,-1.,-0.780158678615542));
#41659=CARTESIAN_POINT('Ctrl Pts',(-3.91697036054676,-1.,-0.781303428618366));
#41660=CARTESIAN_POINT('Ctrl Pts',(-3.90944671004542,-1.,-0.782405395622764));
#41661=CARTESIAN_POINT('Ctrl Pts',(-3.9019303904397,-1.,-0.783464141529081));
#41662=CARTESIAN_POINT('Ctrl Pts',(-3.89442039235103,-1.,-0.784478799358336));
#41663=CARTESIAN_POINT('Ctrl Pts',(-3.88691313167398,-1.,-0.78544789034073));
#41664=CARTESIAN_POINT('Ctrl Pts',(-3.8794040281819,-1.,-0.786369675812608));
#41665=CARTESIAN_POINT('Ctrl Pts',(-3.87188916600912,-1.,-0.787242527617999));
#41666=CARTESIAN_POINT('Ctrl Pts',(-3.86436702561345,-1.,-0.788065315093777));
#41667=CARTESIAN_POINT('Ctrl Pts',(-3.85683995872529,-1.,-0.788837734090672));
#41668=CARTESIAN_POINT('Ctrl Pts',(-3.84931637808894,-1.,-0.789560798155582));
#41669=CARTESIAN_POINT('Ctrl Pts',(-3.84180762342454,-1.,-0.790236124191242));
#41670=CARTESIAN_POINT('Ctrl Pts',(-3.83432392054786,-1.,-0.790865012705301));
#41671=CARTESIAN_POINT('Ctrl Pts',(-3.82687033899792,-1.,-0.791447528662369));
#41672=CARTESIAN_POINT('Ctrl Pts',(-3.81944345442249,-1.,-0.791981740718635));
#41673=CARTESIAN_POINT('Ctrl Pts',(-3.81202588694756,-1.,-0.792462483517634));
#41674=CARTESIAN_POINT('Ctrl Pts',(-3.80459229925637,-1.,-0.792882695234778));
#41675=CARTESIAN_POINT('Ctrl Pts',(-3.79711921389897,-1.,-0.793235612973273));
#41676=CARTESIAN_POINT('Ctrl Pts',(-3.78959439439235,-1.,-0.793516871680993));
#41677=CARTESIAN_POINT('Ctrl Pts',(-3.78202460377598,-1.,-0.7937262357813));
#41678=CARTESIAN_POINT('Ctrl Pts',(-3.77444863801212,-1.,-0.793870523787408));
#41679=CARTESIAN_POINT('Ctrl Pts',(-3.76692626931111,-1.,-0.793961083688991));
#41680=CARTESIAN_POINT('Ctrl Pts',(-3.75951468666257,-1.,-0.794008429134907));
#41681=CARTESIAN_POINT('Ctrl Pts',(-3.75224692493864,-1.,-0.794017347371377));
#41682=CARTESIAN_POINT('Ctrl Pts',(-3.74511357728861,-1.,-0.793982700459952));
#41683=CARTESIAN_POINT('Ctrl Pts',(-3.73803280541687,-1.,-0.793882700937017));
#41684=CARTESIAN_POINT('Ctrl Pts',(-3.73086914695805,-1.,-0.793682750269684));
#41685=CARTESIAN_POINT('Ctrl Pts',(-3.72348797293734,-1.,-0.793347023784205));
#41686=CARTESIAN_POINT('Ctrl Pts',(-3.71580242396124,-1.,-0.792848377370287));
#41687=CARTESIAN_POINT('Ctrl Pts',(-3.70781724021806,-1.,-0.792177688845818));
#41688=CARTESIAN_POINT('Ctrl Pts',(-3.69968940808721,-1.,-0.79135657569598));
#41689=CARTESIAN_POINT('Ctrl Pts',(-3.69172044327364,-1.,-0.790436284988787));
#41690=CARTESIAN_POINT('Ctrl Pts',(-3.68428439783905,-1.,-0.789483546064387));
#41691=CARTESIAN_POINT('Ctrl Pts',(-3.67777119516252,-1.,-0.788569566220285));
#41692=CARTESIAN_POINT('Ctrl Pts',(-3.67252923663655,-1.,-0.787758799995742));
#41693=CARTESIAN_POINT('Ctrl Pts',(-3.66907505398677,-1.,-0.787145041181545));
#41694=CARTESIAN_POINT('Ctrl Pts',(-3.66743103898702,-1.,-0.786774337198062));
#41695=CARTESIAN_POINT('Ctrl Pts',(-3.66680946938292,-1.,-0.786565919558984));
#41696=CARTESIAN_POINT('Ctrl Pts',(-3.6666431041522,-1.,-0.786459983895432));
#41697=CARTESIAN_POINT('Ctrl Pts',(-3.66661143271685,-1.,-0.786422660831985));
#41698=CARTESIAN_POINT('',(-3.62400312501245,-1.,-0.963899035117249));
#41699=CARTESIAN_POINT('Origin',(0.,-1.,0.));
#41700=CARTESIAN_POINT('',(-4.01728681790024,-1.,-1.22531898815164));
#41701=CARTESIAN_POINT('Ctrl Pts',(-3.62400312501245,-1.,-0.963899035117249));
#41702=CARTESIAN_POINT('Ctrl Pts',(-3.6240482887845,-1.,-0.963880158555582));
#41703=CARTESIAN_POINT('Ctrl Pts',(-3.62424461507588,-1.,-0.963861297423241));
#41704=CARTESIAN_POINT('Ctrl Pts',(-3.62489305727662,-1.,-0.963957782642843));
#41705=CARTESIAN_POINT('Ctrl Pts',(-3.62652618145335,-1.,-0.964373850166457));
#41706=CARTESIAN_POINT('Ctrl Pts',(-3.62988252139846,-1.,-0.965395153165293));
#41707=CARTESIAN_POINT('Ctrl Pts',(-3.63492122081143,-1.,-0.967052554541385));
#41708=CARTESIAN_POINT('Ctrl Pts',(-3.64113946505766,-1.,-0.969195124675865));
#41709=CARTESIAN_POINT('Ctrl Pts',(-3.64819756447455,-1.,-0.971722122061341));
#41710=CARTESIAN_POINT('Ctrl Pts',(-3.65571576735126,-1.,-0.974519971354848));
#41711=CARTESIAN_POINT('Ctrl Pts',(-3.66333049637475,-1.,-0.977478312751618));
#41712=CARTESIAN_POINT('Ctrl Pts',(-3.67074983340361,-1.,-0.980505922458267));
#41713=CARTESIAN_POINT('Ctrl Pts',(-3.67782408841715,-1.,-0.983550791470419));
#41714=CARTESIAN_POINT('Ctrl Pts',(-3.68455317926068,-1.,-0.986602639863837));
#41715=CARTESIAN_POINT('Ctrl Pts',(-3.69102682138846,-1.,-0.989676715398558));
#41716=CARTESIAN_POINT('Ctrl Pts',(-3.69738123415662,-1.,-0.99280221833201));
#41717=CARTESIAN_POINT('Ctrl Pts',(-3.70375282282138,-1.,-0.996009819772518));
#41718=CARTESIAN_POINT('Ctrl Pts',(-3.71022439713938,-1.,-0.99931726075653));
#41719=CARTESIAN_POINT('Ctrl Pts',(-3.71680667125118,-1.,-1.00272423396822));
#41720=CARTESIAN_POINT('Ctrl Pts',(-3.72346803750595,-1.,-1.0062200073571));
#41721=CARTESIAN_POINT('Ctrl Pts',(-3.73015276704426,-1.,-1.00978798539496));
#41722=CARTESIAN_POINT('Ctrl Pts',(-3.73680245055734,-1.,-1.01341114319903));
#41723=CARTESIAN_POINT('Ctrl Pts',(-3.74337942504959,-1.,-1.01707794311079));
#41724=CARTESIAN_POINT('Ctrl Pts',(-3.74987777155834,-1.,-1.02078510487428));
#41725=CARTESIAN_POINT('Ctrl Pts',(-3.75631037456194,-1.,-1.0245342944466));
#41726=CARTESIAN_POINT('Ctrl Pts',(-3.76270122291232,-1.,-1.02833014458181));
#41727=CARTESIAN_POINT('Ctrl Pts',(-3.76907609832522,-1.,-1.0321778660492));
#41728=CARTESIAN_POINT('Ctrl Pts',(-3.77545283140445,-1.,-1.03608074678013));
#41729=CARTESIAN_POINT('Ctrl Pts',(-3.78183535008192,-1.,-1.04003862055804));
#41730=CARTESIAN_POINT('Ctrl Pts',(-3.78821910787195,-1.,-1.04404924374426));
#41731=CARTESIAN_POINT('Ctrl Pts',(-3.79459440308793,-1.,-1.04810913267641));
#41732=CARTESIAN_POINT('Ctrl Pts',(-3.80095039790678,-1.,-1.05221457990015));
#41733=CARTESIAN_POINT('Ctrl Pts',(-3.80727913637784,-1.,-1.05636266918643));
#41734=CARTESIAN_POINT('Ctrl Pts',(-3.81357866117485,-1.,-1.06055206187298));
#41735=CARTESIAN_POINT('Ctrl Pts',(-3.81985083953012,-1.,-1.06478244038931));
#41736=CARTESIAN_POINT('Ctrl Pts',(-3.82609989967278,-1.,-1.0690541318036));
#41737=CARTESIAN_POINT('Ctrl Pts',(-3.83233071195145,-1.,-1.0733676663346));
#41738=CARTESIAN_POINT('Ctrl Pts',(-3.83854714117486,-1.,-1.07772335353856));
#41739=CARTESIAN_POINT('Ctrl Pts',(-3.84475048030615,-1.,-1.08212087917986));
#41740=CARTESIAN_POINT('Ctrl Pts',(-3.8509402522269,-1.,-1.08655950846377));
#41741=CARTESIAN_POINT('Ctrl Pts',(-3.85711487933911,-1.,-1.09103825516288));
#41742=CARTESIAN_POINT('Ctrl Pts',(-3.86327241021242,-1.,-1.09555606505012));
#41743=CARTESIAN_POINT('Ctrl Pts',(-3.86941120134872,-1.,-1.10011198761202));
#41744=CARTESIAN_POINT('Ctrl Pts',(-3.87553067187566,-1.,-1.10470536603303));
#41745=CARTESIAN_POINT('Ctrl Pts',(-3.88163105531791,-1.,-1.10933577224029));
#41746=CARTESIAN_POINT('Ctrl Pts',(-3.88771308285229,-1.,-1.11400292434447));
#41747=CARTESIAN_POINT('Ctrl Pts',(-3.89377768340362,-1.,-1.11870660794609));
#41748=CARTESIAN_POINT('Ctrl Pts',(-3.89982569749978,-1.,-1.12344660099029));
#41749=CARTESIAN_POINT('Ctrl Pts',(-3.90585753318622,-1.,-1.12822258281518));
#41750=CARTESIAN_POINT('Ctrl Pts',(-3.91187321145495,-1.,-1.13303414693849));
#41751=CARTESIAN_POINT('Ctrl Pts',(-3.91787251936688,-1.,-1.13788084225511));
#41752=CARTESIAN_POINT('Ctrl Pts',(-3.92385513133937,-1.,-1.14276220561575));
#41753=CARTESIAN_POINT('Ctrl Pts',(-3.92982073294334,-1.,-1.14767779451147));
#41754=CARTESIAN_POINT('Ctrl Pts',(-3.9357691705651,-1.,-1.1526272271639));
#41755=CARTESIAN_POINT('Ctrl Pts',(-3.94170046685542,-1.,-1.1576101834106));
#41756=CARTESIAN_POINT('Ctrl Pts',(-3.9476147478092,-1.,-1.16262637999261));
#41757=CARTESIAN_POINT('Ctrl Pts',(-3.95351219510062,-1.,-1.16767555244495));
#41758=CARTESIAN_POINT('Ctrl Pts',(-3.95939299213164,-1.,-1.17275743590327));
#41759=CARTESIAN_POINT('Ctrl Pts',(-3.96525726357682,-1.,-1.17787174135445));
#41760=CARTESIAN_POINT('Ctrl Pts',(-3.9711050516465,-1.,-1.18301815039596));
#41761=CARTESIAN_POINT('Ctrl Pts',(-3.97693634766926,-1.,-1.18819633715285));
#41762=CARTESIAN_POINT('Ctrl Pts',(-3.98275111052015,-1.,-1.19340598349307));
#41763=CARTESIAN_POINT('Ctrl Pts',(-3.98854928957287,-1.,-1.19864679609596));
#41764=CARTESIAN_POINT('Ctrl Pts',(-3.99433084800649,-1.,-1.2039185237544));
#41765=CARTESIAN_POINT('Ctrl Pts',(-4.00009577952534,-1.,-1.20922097030107));
#41766=CARTESIAN_POINT('Ctrl Pts',(-4.00584409524937,-1.,-1.21455398918813));
#41767=CARTESIAN_POINT('Ctrl Pts',(-4.01042947142681,-1.,-1.21884478244983));
#41768=CARTESIAN_POINT('Ctrl Pts',(-4.01386104434674,-1.,-1.22207656456199));
#41769=CARTESIAN_POINT('Ctrl Pts',(-4.0161454457032,-1.,-1.22423716681447));
#41770=CARTESIAN_POINT('Ctrl Pts',(-4.01728681790024,-1.,-1.22531898815164));
#41771=CARTESIAN_POINT('',(-3.97027773754922,-1.,-1.36999806084572));
#41772=CARTESIAN_POINT('',(-4.01728681790024,-1.,-1.22531898815164));
#41773=CARTESIAN_POINT('',(-3.4984457533445,-1.,-1.35032489087101));
#41774=CARTESIAN_POINT('Ctrl Pts',(-3.97027773754922,-1.,-1.36999806084572));
#41775=CARTESIAN_POINT('Ctrl Pts',(-3.9687184694131,-1.,-1.37020239094614));
#41776=CARTESIAN_POINT('Ctrl Pts',(-3.96560037974645,-1.,-1.37060761745635));
#41777=CARTESIAN_POINT('Ctrl Pts',(-3.96092458506535,-1.,-1.3712051561502));
#41778=CARTESIAN_POINT('Ctrl Pts',(-3.95469287280914,-1.,-1.37198126432386));
#41779=CARTESIAN_POINT('Ctrl Pts',(-3.94690771785133,-1.,-1.37291699202807));
#41780=CARTESIAN_POINT('Ctrl Pts',(-3.93912709040818,-1.,-1.37381821967165));
#41781=CARTESIAN_POINT('Ctrl Pts',(-3.93135106761844,-1.,-1.37468482215751));
#41782=CARTESIAN_POINT('Ctrl Pts',(-3.92357976987672,-1.,-1.37551664448242));
#41783=CARTESIAN_POINT('Ctrl Pts',(-3.91581337462644,-1.,-1.37631350505797));
#41784=CARTESIAN_POINT('Ctrl Pts',(-3.90805209523486,-1.,-1.3770751963402));
#41785=CARTESIAN_POINT('Ctrl Pts',(-3.90029615196727,-1.,-1.37780148512792));
#41786=CARTESIAN_POINT('Ctrl Pts',(-3.89254574338496,-1.,-1.3784921128802));
#41787=CARTESIAN_POINT('Ctrl Pts',(-3.88480102249277,-1.,-1.37914679719383));
#41788=CARTESIAN_POINT('Ctrl Pts',(-3.87706205830532,-1.,-1.37976523097073));
#41789=CARTESIAN_POINT('Ctrl Pts',(-3.86932885813068,-1.,-1.38034709213014));
#41790=CARTESIAN_POINT('Ctrl Pts',(-3.86160143043959,-1.,-1.38089205992989));
#41791=CARTESIAN_POINT('Ctrl Pts',(-3.85387983979481,-1.,-1.38139983115049));
#41792=CARTESIAN_POINT('Ctrl Pts',(-3.84616425605764,-1.,-1.38187013346109));
#41793=CARTESIAN_POINT('Ctrl Pts',(-3.83845502790746,-1.,-1.38230274828821));
#41794=CARTESIAN_POINT('Ctrl Pts',(-3.8307526698229,-1.,-1.38269750245138));
#41795=CARTESIAN_POINT('Ctrl Pts',(-3.82305771743829,-1.,-1.38305421262763));
#41796=CARTESIAN_POINT('Ctrl Pts',(-3.81537060817811,-1.,-1.38337263902782));
#41797=CARTESIAN_POINT('Ctrl Pts',(-3.80769156398411,-1.,-1.3836524404622));
#41798=CARTESIAN_POINT('Ctrl Pts',(-3.80002044322111,-1.,-1.38389311766682));
#41799=CARTESIAN_POINT('Ctrl Pts',(-3.79235669640841,-1.,-1.38409399694566));
#41800=CARTESIAN_POINT('Ctrl Pts',(-3.78469969805082,-1.,-1.38425435883756));
#41801=CARTESIAN_POINT('Ctrl Pts',(-3.77704902230418,-1.,-1.38437354551428));
#41802=CARTESIAN_POINT('Ctrl Pts',(-3.76940473185779,-1.,-1.38445107339518));
#41803=CARTESIAN_POINT('Ctrl Pts',(-3.76176768271367,-1.,-1.3844867525335));
#41804=CARTESIAN_POINT('Ctrl Pts',(-3.7541397631875,-1.,-1.38448077997163));
#41805=CARTESIAN_POINT('Ctrl Pts',(-3.74652317167876,-1.,-1.38443344984394));
#41806=CARTESIAN_POINT('Ctrl Pts',(-3.73891976418104,-1.,-1.38434489156458));
#41807=CARTESIAN_POINT('Ctrl Pts',(-3.73133035859282,-1.,-1.38421479111531));
#41808=CARTESIAN_POINT('Ctrl Pts',(-3.72375409358803,-1.,-1.3840421342895));
#41809=CARTESIAN_POINT('Ctrl Pts',(-3.7161876605181,-1.,-1.38382489984586));
#41810=CARTESIAN_POINT('Ctrl Pts',(-3.70862680753347,-1.,-1.38356065402124));
#41811=CARTESIAN_POINT('Ctrl Pts',(-3.701067921679,-1.,-1.38324717612865));
#41812=CARTESIAN_POINT('Ctrl Pts',(-3.69350967899526,-1.,-1.3828831117165));
#41813=CARTESIAN_POINT('Ctrl Pts',(-3.68595444983837,-1.,-1.38246852827182));
#41814=CARTESIAN_POINT('Ctrl Pts',(-3.67841038482414,-1.,-1.3820057429062));
#41815=CARTESIAN_POINT('Ctrl Pts',(-3.67088843112262,-1.,-1.38149812653868));
#41816=CARTESIAN_POINT('Ctrl Pts',(-3.66339848520857,-1.,-1.38094856333552));
#41817=CARTESIAN_POINT('Ctrl Pts',(-3.6559455440439,-1.,-1.38035791051212));
#41818=CARTESIAN_POINT('Ctrl Pts',(-3.64852652756456,-1.,-1.37972372481603));
#41819=CARTESIAN_POINT('Ctrl Pts',(-3.64112507791141,-1.,-1.37903818567359));
#41820=CARTESIAN_POINT('Ctrl Pts',(-3.63371727442486,-1.,-1.37829035457339));
#41821=CARTESIAN_POINT('Ctrl Pts',(-3.62628098665145,-1.,-1.37746987919881));
#41822=CARTESIAN_POINT('Ctrl Pts',(-3.6188048116042,-1.,-1.37657053403107));
#41823=CARTESIAN_POINT('Ctrl Pts',(-3.61129546591064,-1.,-1.37559314436634));
#41824=CARTESIAN_POINT('Ctrl Pts',(-3.60379020123988,-1.,-1.37455051379623));
#41825=CARTESIAN_POINT('Ctrl Pts',(-3.59634627869048,-1.,-1.37346320103157));
#41826=CARTESIAN_POINT('Ctrl Pts',(-3.58901853846365,-1.,-1.37235053660976));
#41827=CARTESIAN_POINT('Ctrl Pts',(-3.58183885982715,-1.,-1.37122241663062));
#41828=CARTESIAN_POINT('Ctrl Pts',(-3.57479875549486,-1.,-1.37007229485659));
#41829=CARTESIAN_POINT('Ctrl Pts',(-3.5678208030466,-1.,-1.36886584973389));
#41830=CARTESIAN_POINT('Ctrl Pts',(-3.56077662028649,-1.,-1.36754771771233));
#41831=CARTESIAN_POINT('Ctrl Pts',(-3.55353883995949,-1.,-1.3660614545677));
#41832=CARTESIAN_POINT('Ctrl Pts',(-3.54602591832973,-1.,-1.36436666257597));
#41833=CARTESIAN_POINT('Ctrl Pts',(-3.53824396424961,-1.,-1.36245507339307));
#41834=CARTESIAN_POINT('Ctrl Pts',(-3.530344649616,-1.,-1.36037259643734));
#41835=CARTESIAN_POINT('Ctrl Pts',(-3.52261776116748,-1.,-1.35821701528836));
#41836=CARTESIAN_POINT('Ctrl Pts',(-3.51542230699556,-1.,-1.35611275237152));
#41837=CARTESIAN_POINT('Ctrl Pts',(-3.50913227059999,-1.,-1.35419113575956));
#41838=CARTESIAN_POINT('Ctrl Pts',(-3.50408168106261,-1.,-1.35257032843486));
#41839=CARTESIAN_POINT('Ctrl Pts',(-3.5007660381649,-1.,-1.35142377279517));
#41840=CARTESIAN_POINT('Ctrl Pts',(-3.49920025459723,-1.,-1.35080045218587));
#41841=CARTESIAN_POINT('Ctrl Pts',(-3.49861894124827,-1.,-1.35049736560527));
#41842=CARTESIAN_POINT('Ctrl Pts',(-3.49847119623846,-1.,-1.35036670892966));
#41843=CARTESIAN_POINT('Ctrl Pts',(-3.4984457533445,-1.,-1.35032489087101));
#41844=CARTESIAN_POINT('',(-3.42859860294378,-1.,-1.51895082866166));
#41845=CARTESIAN_POINT('Origin',(0.,-1.,0.));
#41846=CARTESIAN_POINT('',(-3.77614523045147,-1.,-1.83867539237861));
#41847=CARTESIAN_POINT('Ctrl Pts',(-3.42859860294378,-1.,-1.51895082866166));
#41848=CARTESIAN_POINT('Ctrl Pts',(-3.42864616361967,-1.,-1.51893924967231));
#41849=CARTESIAN_POINT('Ctrl Pts',(-3.42884302333978,-1.,-1.51895133295017));
#41850=CARTESIAN_POINT('Ctrl Pts',(-3.42946838852728,-1.,-1.51914806898539));
#41851=CARTESIAN_POINT('Ctrl Pts',(-3.43101631893491,-1.,-1.5198144909343));
#41852=CARTESIAN_POINT('Ctrl Pts',(-3.43417156977749,-1.,-1.52134826724227));
#41853=CARTESIAN_POINT('Ctrl Pts',(-3.43888895974182,-1.,-1.52377348950429));
#41854=CARTESIAN_POINT('Ctrl Pts',(-3.44469547527,-1.,-1.52686242875717));
#41855=CARTESIAN_POINT('Ctrl Pts',(-3.45127136828667,-1.,-1.530462444618));
#41856=CARTESIAN_POINT('Ctrl Pts',(-3.45825932955273,-1.,-1.53440195378902));
#41857=CARTESIAN_POINT('Ctrl Pts',(-3.46531752207222,-1.,-1.53851507915533));
#41858=CARTESIAN_POINT('Ctrl Pts',(-3.47217189224576,-1.,-1.54266605398152));
#41859=CARTESIAN_POINT('Ctrl Pts',(-3.47868272898599,-1.,-1.54678009290206));
#41860=CARTESIAN_POINT('Ctrl Pts',(-3.48485155928414,-1.,-1.55084702970382));
#41861=CARTESIAN_POINT('Ctrl Pts',(-3.49076460877317,-1.,-1.5548959590107));
#41862=CARTESIAN_POINT('Ctrl Pts',(-3.49655185179623,-1.,-1.55897703097859));
#41863=CARTESIAN_POINT('Ctrl Pts',(-3.50234321621607,-1.,-1.56314187758689));
#41864=CARTESIAN_POINT('Ctrl Pts',(-3.50821771695427,-1.,-1.56742097575041));
#41865=CARTESIAN_POINT('Ctrl Pts',(-3.51418598431733,-1.,-1.57181569799774));
#41866=CARTESIAN_POINT('Ctrl Pts',(-3.52021847865961,-1.,-1.5763104998818));
#41867=CARTESIAN_POINT('Ctrl Pts',(-3.52626275334899,-1.,-1.58088027227856));
#41868=CARTESIAN_POINT('Ctrl Pts',(-3.53226378147068,-1.,-1.58549906268083));
#41869=CARTESIAN_POINT('Ctrl Pts',(-3.53818616861045,-1.,-1.59014958368725));
#41870=CARTESIAN_POINT('Ctrl Pts',(-3.544024581823,-1.,-1.5948276694975));
#41871=CARTESIAN_POINT('Ctrl Pts',(-3.54979148634426,-1.,-1.59953698113444));
#41872=CARTESIAN_POINT('Ctrl Pts',(-3.55550985096117,-1.,-1.60428584699848));
#41873=CARTESIAN_POINT('Ctrl Pts',(-3.56120432482986,-1.,-1.60908344685459));
#41874=CARTESIAN_POINT('Ctrl Pts',(-3.56689200468404,-1.,-1.61393581747522));
#41875=CARTESIAN_POINT('Ctrl Pts',(-3.57257679609826,-1.,-1.61884340915412));
#41876=CARTESIAN_POINT('Ctrl Pts',(-3.57825455954405,-1.,-1.62380329464851));
#41877=CARTESIAN_POINT('Ctrl Pts',(-3.5839162577435,-1.,-1.62881051550748));
#41878=CARTESIAN_POINT('Ctrl Pts',(-3.58955176627876,-1.,-1.63385971451259));
#41879=CARTESIAN_POINT('Ctrl Pts',(-3.59515368334887,-1.,-1.63894676675349));
#41880=CARTESIAN_POINT('Ctrl Pts',(-3.6007202851384,-1.,-1.6440700438558));
#41881=CARTESIAN_POINT('Ctrl Pts',(-3.60625346556992,-1.,-1.64922952425833));
#41882=CARTESIAN_POINT('Ctrl Pts',(-3.61175734965129,-1.,-1.65442619244327));
#41883=CARTESIAN_POINT('Ctrl Pts',(-3.61723666482457,-1.,-1.65966133399186));
#41884=CARTESIAN_POINT('Ctrl Pts',(-3.62269517989104,-1.,-1.66493585923853));
#41885=CARTESIAN_POINT('Ctrl Pts',(-3.62813422105257,-1.,-1.67024966008037));
#41886=CARTESIAN_POINT('Ctrl Pts',(-3.63355343201211,-1.,-1.67560193613145));
#41887=CARTESIAN_POINT('Ctrl Pts',(-3.63895140887443,-1.,-1.68099146651577));
#41888=CARTESIAN_POINT('Ctrl Pts',(-3.64432638915199,-1.,-1.68641690471455));
#41889=CARTESIAN_POINT('Ctrl Pts',(-3.64967689827393,-1.,-1.691877054817));
#41890=CARTESIAN_POINT('Ctrl Pts',(-3.65500246526798,-1.,-1.69737117722558));
#41891=CARTESIAN_POINT('Ctrl Pts',(-3.6603033877491,-1.,-1.70289888566904));
#41892=CARTESIAN_POINT('Ctrl Pts',(-3.6655804319893,-1.,-1.70846001610983));
#41893=CARTESIAN_POINT('Ctrl Pts',(-3.67083454901629,-1.,-1.71405450210392));
#41894=CARTESIAN_POINT('Ctrl Pts',(-3.67606660374665,-1.,-1.71968225581787));
#41895=CARTESIAN_POINT('Ctrl Pts',(-3.68127704936472,-1.,-1.72534302437003));
#41896=CARTESIAN_POINT('Ctrl Pts',(-3.68646597019188,-1.,-1.73103640956647));
#41897=CARTESIAN_POINT('Ctrl Pts',(-3.69163322647906,-1.,-1.73676193254493));
#41898=CARTESIAN_POINT('Ctrl Pts',(-3.6967785691046,-1.,-1.74251908492589));
#41899=CARTESIAN_POINT('Ctrl Pts',(-3.70190175673422,-1.,-1.74830738046092));
#41900=CARTESIAN_POINT('Ctrl Pts',(-3.70700269736876,-1.,-1.75412641804148));
#41901=CARTESIAN_POINT('Ctrl Pts',(-3.71208146346454,-1.,-1.75997588499021));
#41902=CARTESIAN_POINT('Ctrl Pts',(-3.71713822377675,-1.,-1.76585552124549));
#41903=CARTESIAN_POINT('Ctrl Pts',(-3.72217319911429,-1.,-1.77176509401846));
#41904=CARTESIAN_POINT('Ctrl Pts',(-3.72718661205504,-1.,-1.77770437039606));
#41905=CARTESIAN_POINT('Ctrl Pts',(-3.73217863095022,-1.,-1.78367308442682));
#41906=CARTESIAN_POINT('Ctrl Pts',(-3.73714934729962,-1.,-1.78967092823139));
#41907=CARTESIAN_POINT('Ctrl Pts',(-3.74209880351667,-1.,-1.79569757859041));
#41908=CARTESIAN_POINT('Ctrl Pts',(-3.74702700874954,-1.,-1.80175271485519));
#41909=CARTESIAN_POINT('Ctrl Pts',(-3.75193395888069,-1.,-1.80783603939662));
#41910=CARTESIAN_POINT('Ctrl Pts',(-3.75681965683995,-1.,-1.81394729834032));
#41911=CARTESIAN_POINT('Ctrl Pts',(-3.76168412709652,-1.,-1.82008629694924));
#41912=CARTESIAN_POINT('Ctrl Pts',(-3.76652740355856,-1.,-1.82625289221933));
#41913=CARTESIAN_POINT('Ctrl Pts',(-3.77038509819777,-1.,-1.83120816956515));
#41914=CARTESIAN_POINT('Ctrl Pts',(-3.77326886065484,-1.,-1.83493697935064));
#41915=CARTESIAN_POINT('Ctrl Pts',(-3.77518714458232,-1.,-1.83742834010821));
#41916=CARTESIAN_POINT('Ctrl Pts',(-3.77614523045147,-1.,-1.83867539237861));
#41917=CARTESIAN_POINT('',(-3.70708211654725,-1.,-1.97421938526992));
#41918=CARTESIAN_POINT('',(-3.77614523045147,-1.,-1.83867539237861));
#41919=CARTESIAN_POINT('',(-3.24413672884902,-1.,-1.88097764062542));
#41920=CARTESIAN_POINT('Ctrl Pts',(-3.70708211654725,-1.,-1.97421938526992));
#41921=CARTESIAN_POINT('Ctrl Pts',(-3.7055100813194,-1.,-1.974177276451));
#41922=CARTESIAN_POINT('Ctrl Pts',(-3.70236698911837,-1.,-1.97408973726149));
#41923=CARTESIAN_POINT('Ctrl Pts',(-3.69765528558292,-1.,-1.97394846382288));
#41924=CARTESIAN_POINT('Ctrl Pts',(-3.69137888597855,-1.,-1.97374016224397));
#41925=CARTESIAN_POINT('Ctrl Pts',(-3.68354319913416,-1.,-1.9734465030363));
#41926=CARTESIAN_POINT('Ctrl Pts',(-3.67571738106175,-1.,-1.97311947678035));
#41927=CARTESIAN_POINT('Ctrl Pts',(-3.66790152751984,-1.,-1.9727589719863));
#41928=CARTESIAN_POINT('Ctrl Pts',(-3.66009578166865,-1.,-1.97236485439317));
#41929=CARTESIAN_POINT('Ctrl Pts',(-3.65230034717364,-1.,-1.97193697240645));
#41930=CARTESIAN_POINT('Ctrl Pts',(-3.64451546724221,-1.,-1.97147515441539));
#41931=CARTESIAN_POINT('Ctrl Pts',(-3.63674139590853,-1.,-1.97097920454698));
#41932=CARTESIAN_POINT('Ctrl Pts',(-3.62897836973397,-1.,-1.97044889850518));
#41933=CARTESIAN_POINT('Ctrl Pts',(-3.62122658401722,-1.,-1.96988398129888));
#41934=CARTESIAN_POINT('Ctrl Pts',(-3.61348615496393,-1.,-1.96928416040712));
#41935=CARTESIAN_POINT('Ctrl Pts',(-3.60575714017676,-1.,-1.96864911885775));
#41936=CARTESIAN_POINT('Ctrl Pts',(-3.59803959819725,-1.,-1.96797854118257));
#41937=CARTESIAN_POINT('Ctrl Pts',(-3.5903336402273,-1.,-1.96727213799507));
#41938=CARTESIAN_POINT('Ctrl Pts',(-3.58263947663884,-1.,-1.9665296668894));
#41939=CARTESIAN_POINT('Ctrl Pts',(-3.57495748601088,-1.,-1.96575096652857));
#41940=CARTESIAN_POINT('Ctrl Pts',(-3.56728820357933,-1.,-1.96493594634643));
#41941=CARTESIAN_POINT('Ctrl Pts',(-3.55963218706201,-1.,-1.96408450906868));
#41942=CARTESIAN_POINT('Ctrl Pts',(-3.55198990600929,-1.,-1.96319648628667));
#41943=CARTESIAN_POINT('Ctrl Pts',(-3.54436163300425,-1.,-1.96227157573058));
#41944=CARTESIAN_POINT('Ctrl Pts',(-3.53674730625759,-1.,-1.96130926212661));
#41945=CARTESIAN_POINT('Ctrl Pts',(-3.52914648844289,-1.,-1.96030879411534));
#41946=CARTESIAN_POINT('Ctrl Pts',(-3.52155867431438,-1.,-1.95926936324436));
#41947=CARTESIAN_POINT('Ctrl Pts',(-3.51398354617772,-1.,-1.95819025316768));
#41948=CARTESIAN_POINT('Ctrl Pts',(-3.50642124159913,-1.,-1.95707099606513));
#41949=CARTESIAN_POINT('Ctrl Pts',(-3.49887263575602,-1.,-1.9559115382367));
#41950=CARTESIAN_POINT('Ctrl Pts',(-3.49133956289154,-1.,-1.95471236969653));
#41951=CARTESIAN_POINT('Ctrl Pts',(-3.48382414832648,-1.,-1.95347412486316));
#41952=CARTESIAN_POINT('Ctrl Pts',(-3.47632820495926,-1.,-1.95219722189878));
#41953=CARTESIAN_POINT('Ctrl Pts',(-3.4688525897419,-1.,-1.95088147859876));
#41954=CARTESIAN_POINT('Ctrl Pts',(-3.46139661060959,-1.,-1.94952575850196));
#41955=CARTESIAN_POINT('Ctrl Pts',(-3.45395731584051,-1.,-1.94812754766524));
#41956=CARTESIAN_POINT('Ctrl Pts',(-3.44653088665685,-1.,-1.94668377715332));
#41957=CARTESIAN_POINT('Ctrl Pts',(-3.43911410197693,-1.,-1.94519168842883));
#41958=CARTESIAN_POINT('Ctrl Pts',(-3.43170586602436,-1.,-1.94364973660285));
#41959=CARTESIAN_POINT('Ctrl Pts',(-3.42430850941497,-1.,-1.94205835913692));
#41960=CARTESIAN_POINT('Ctrl Pts',(-3.41692971994082,-1.,-1.94042111965237));
#41961=CARTESIAN_POINT('Ctrl Pts',(-3.40957978266622,-1.,-1.93874306008132));
#41962=CARTESIAN_POINT('Ctrl Pts',(-3.40226802104093,-1.,-1.93702857723089));
#41963=CARTESIAN_POINT('Ctrl Pts',(-3.39499923640789,-1.,-1.93527929945982));
#41964=CARTESIAN_POINT('Ctrl Pts',(-3.38777076883267,-1.,-1.93349233176794));
#41965=CARTESIAN_POINT('Ctrl Pts',(-3.38056768525577,-1.,-1.93165739093292));
#41966=CARTESIAN_POINT('Ctrl Pts',(-3.37336807068078,-1.,-1.92975993109897));
#41967=CARTESIAN_POINT('Ctrl Pts',(-3.36615168657597,-1.,-1.92778626543803));
#41968=CARTESIAN_POINT('Ctrl Pts',(-3.35890824422976,-1.,-1.92572846125763));
#41969=CARTESIAN_POINT('Ctrl Pts',(-3.35164424847206,-1.,-1.92358838440518));
#41970=CARTESIAN_POINT('Ctrl Pts',(-3.34439448941915,-1.,-1.92138450828378));
#41971=CARTESIAN_POINT('Ctrl Pts',(-3.33721230709948,-1.,-1.91914609610173));
#41972=CARTESIAN_POINT('Ctrl Pts',(-3.33014884257812,-1.,-1.91690081930297));
#41973=CARTESIAN_POINT('Ctrl Pts',(-3.32323403454507,-1.,-1.91466343916612));
#41974=CARTESIAN_POINT('Ctrl Pts',(-3.31646052426395,-1.,-1.91242616234459));
#41975=CARTESIAN_POINT('Ctrl Pts',(-3.30975721158694,-1.,-1.91014297830502));
#41976=CARTESIAN_POINT('Ctrl Pts',(-3.30300595568341,-1.,-1.90773912171424));
#41977=CARTESIAN_POINT('Ctrl Pts',(-3.29608978722258,-1.,-1.9051389186417));
#41978=CARTESIAN_POINT('Ctrl Pts',(-3.28893448600364,-1.,-1.9022897124757));
#41979=CARTESIAN_POINT('Ctrl Pts',(-3.28154737912287,-1.,-1.89918429230424));
#41980=CARTESIAN_POINT('Ctrl Pts',(-3.27407108932908,-1.,-1.89589172903662));
#41981=CARTESIAN_POINT('Ctrl Pts',(-3.2667765388833,-1.,-1.89255393500769));
#41982=CARTESIAN_POINT('Ctrl Pts',(-3.2599988519361,-1.,-1.88934996203508));
#41983=CARTESIAN_POINT('Ctrl Pts',(-3.25408686339298,-1.,-1.88646802523372));
#41984=CARTESIAN_POINT('Ctrl Pts',(-3.24935200512055,-1.,-1.88407708646435));
#41985=CARTESIAN_POINT('Ctrl Pts',(-3.24625654410705,-1.,-1.88242596600422));
#41986=CARTESIAN_POINT('Ctrl Pts',(-3.24480754675942,-1.,-1.88156537699118));
#41987=CARTESIAN_POINT('Ctrl Pts',(-3.24428080352952,-1.,-1.88117508446657));
#41988=CARTESIAN_POINT('Ctrl Pts',(-3.24415531671311,-1.,-1.88102292397987));
#41989=CARTESIAN_POINT('Ctrl Pts',(-3.24413672884902,-1.,-1.88097764062542));
#41990=CARTESIAN_POINT('',(-3.14877060440425,-1.,-2.03660101169564));
#41991=CARTESIAN_POINT('Origin',(0.,-1.,0.));
#41992=CARTESIAN_POINT('',(-3.44202241512147,-1.,-2.40675750623143));
#41993=CARTESIAN_POINT('Ctrl Pts',(-3.14877060440425,-1.,-2.03660101169564));
#41994=CARTESIAN_POINT('Ctrl Pts',(-3.1488193908823,-1.,-2.03659701539175));
#41995=CARTESIAN_POINT('Ctrl Pts',(-3.14901193669147,-1.,-2.03663974554941));
#41996=CARTESIAN_POINT('Ctrl Pts',(-3.14959882629936,-1.,-2.03693188810614));
#41997=CARTESIAN_POINT('Ctrl Pts',(-3.15102344775396,-1.,-2.03783225496023));
#41998=CARTESIAN_POINT('Ctrl Pts',(-3.1538999167466,-1.,-2.03984073791432));
#41999=CARTESIAN_POINT('Ctrl Pts',(-3.15817983946525,-1.,-2.04297406404132));
#42000=CARTESIAN_POINT('Ctrl Pts',(-3.16343165059235,-1.,-2.0469333124766));
#42001=CARTESIAN_POINT('Ctrl Pts',(-3.16936341689859,-1.,-2.05151770247452));
#42002=CARTESIAN_POINT('Ctrl Pts',(-3.17564906975592,-1.,-2.05650186773279));
#42003=CARTESIAN_POINT('Ctrl Pts',(-3.18197692964677,-1.,-2.06166849827143));
#42004=CARTESIAN_POINT('Ctrl Pts',(-3.18809755562297,-1.,-2.06684062744065));
#42005=CARTESIAN_POINT('Ctrl Pts',(-3.19388465568113,-1.,-2.07192253497765));
#42006=CARTESIAN_POINT('Ctrl Pts',(-3.19934132835879,-1.,-2.0769044187063));
#42007=CARTESIAN_POINT('Ctrl Pts',(-3.20454818630635,-1.,-2.08182850370816));
#42008=CARTESIAN_POINT('Ctrl Pts',(-3.20962575845433,-1.,-2.08676465517435));
#42009=CARTESIAN_POINT('Ctrl Pts',(-3.2146942960168,-1.,-2.0917841946046));
#42010=CARTESIAN_POINT('Ctrl Pts',(-3.21982707347067,-1.,-2.09692958434933));
#42011=CARTESIAN_POINT('Ctrl Pts',(-3.22503437553496,-1.,-2.10220384298533));
#42012=CARTESIAN_POINT('Ctrl Pts',(-3.23028945793334,-1.,-2.1075869964248));
#42013=CARTESIAN_POINT('Ctrl Pts',(-3.23554444767115,-1.,-2.11304604021784));
#42014=CARTESIAN_POINT('Ctrl Pts',(-3.24074905517282,-1.,-2.11854673326972));
#42015=CARTESIAN_POINT('Ctrl Pts',(-3.24587102613347,-1.,-2.12406646410943));
#42016=CARTESIAN_POINT('Ctrl Pts',(-3.25090574493994,-1.,-2.1296002839681));
#42017=CARTESIAN_POINT('Ctrl Pts',(-3.25586495065027,-1.,-2.13515375878786));
#42018=CARTESIAN_POINT('Ctrl Pts',(-3.26077002641868,-1.,-2.14073870754257));
#42019=CARTESIAN_POINT('Ctrl Pts',(-3.26564388189764,-1.,-2.14636805295663));
#42020=CARTESIAN_POINT('Ctrl Pts',(-3.27050245897244,-1.,-2.15205043199818));
#42021=CARTESIAN_POINT('Ctrl Pts',(-3.27534954469206,-1.,-2.15778690038359));
#42022=CARTESIAN_POINT('Ctrl Pts',(-3.28018150841414,-1.,-2.16357391934434));
#42023=CARTESIAN_POINT('Ctrl Pts',(-3.2849901997973,-1.,-2.16940517773459));
#42024=CARTESIAN_POINT('Ctrl Pts',(-3.28976645712566,-1.,-2.17527380048422));
#42025=CARTESIAN_POINT('Ctrl Pts',(-3.29450361500484,-1.,-2.18117455557062));
#42026=CARTESIAN_POINT('Ctrl Pts',(-3.29920022557635,-1.,-2.18710556500325));
#42027=CARTESIAN_POINT('Ctrl Pts',(-3.30385816281831,-1.,-2.19306710376112));
#42028=CARTESIAN_POINT('Ctrl Pts',(-3.30848134694596,-1.,-2.19906078949924));
#42029=CARTESIAN_POINT('Ctrl Pts',(-3.3130742460895,-1.,-2.20508863150608));
#42030=CARTESIAN_POINT('Ctrl Pts',(-3.31764044024231,-1.,-2.21115211847872));
#42031=CARTESIAN_POINT('Ctrl Pts',(-3.32218125618955,-1.,-2.21725135110889));
#42032=CARTESIAN_POINT('Ctrl Pts',(-3.32669646722871,-1.,-2.22338548312758));
#42033=CARTESIAN_POINT('Ctrl Pts',(-3.33118487773593,-1.,-2.22955308907221));
#42034=CARTESIAN_POINT('Ctrl Pts',(-3.33564495756478,-1.,-2.2357525632881));
#42035=CARTESIAN_POINT('Ctrl Pts',(-3.34007543738044,-1.,-2.24198249391437));
#42036=CARTESIAN_POINT('Ctrl Pts',(-3.34447596770768,-1.,-2.24824207678288));
#42037=CARTESIAN_POINT('Ctrl Pts',(-3.34884690292342,-1.,-2.25453097693524));
#42038=CARTESIAN_POINT('Ctrl Pts',(-3.35318902552676,-1.,-2.26084915222484));
#42039=CARTESIAN_POINT('Ctrl Pts',(-3.35750328523077,-1.,-2.26719668579921));
#42040=CARTESIAN_POINT('Ctrl Pts',(-3.36179055004369,-1.,-2.27357362620902));
#42041=CARTESIAN_POINT('Ctrl Pts',(-3.36605130712978,-1.,-2.27997979457968));
#42042=CARTESIAN_POINT('Ctrl Pts',(-3.37028570206357,-1.,-2.28641481081045));
#42043=CARTESIAN_POINT('Ctrl Pts',(-3.37449367172707,-1.,-2.2928781800731));
#42044=CARTESIAN_POINT('Ctrl Pts',(-3.37867504959382,-1.,-2.29936936127588));
#42045=CARTESIAN_POINT('Ctrl Pts',(-3.38282967336676,-1.,-2.30588783640389));
#42046=CARTESIAN_POINT('Ctrl Pts',(-3.38695751492659,-1.,-2.31243319489505));
#42047=CARTESIAN_POINT('Ctrl Pts',(-3.39105869475112,-1.,-2.31900513925627));
#42048=CARTESIAN_POINT('Ctrl Pts',(-3.39513342020045,-1.,-2.32560343902683));
#42049=CARTESIAN_POINT('Ctrl Pts',(-3.39918194578115,-1.,-2.33222789882601));
#42050=CARTESIAN_POINT('Ctrl Pts',(-3.40320452776646,-1.,-2.33887832342715));
#42051=CARTESIAN_POINT('Ctrl Pts',(-3.40720137403888,-1.,-2.34555447648901));
#42052=CARTESIAN_POINT('Ctrl Pts',(-3.41117262313464,-1.,-2.35225606823649));
#42053=CARTESIAN_POINT('Ctrl Pts',(-3.4151183675076,-1.,-2.35898278606449));
#42054=CARTESIAN_POINT('Ctrl Pts',(-3.41903866635384,-1.,-2.36573431470314));
#42055=CARTESIAN_POINT('Ctrl Pts',(-3.42293356216595,-1.,-2.37251035954351));
#42056=CARTESIAN_POINT('Ctrl Pts',(-3.42680309755241,-1.,-2.37931067029517));
#42057=CARTESIAN_POINT('Ctrl Pts',(-3.43064732714472,-1.,-2.38613505844641));
#42058=CARTESIAN_POINT('Ctrl Pts',(-3.43446630680436,-1.,-2.39298338805823));
#42059=CARTESIAN_POINT('Ctrl Pts',(-3.43750133066036,-1.,-2.39848113411429));
#42060=CARTESIAN_POINT('Ctrl Pts',(-3.43976627485223,-1.,-2.40261515590099));
#42061=CARTESIAN_POINT('Ctrl Pts',(-3.44127120683402,-1.,-2.40537592959345));
#42062=CARTESIAN_POINT('Ctrl Pts',(-3.44202241512147,-1.,-2.40675750623143));
#42063=CARTESIAN_POINT('',(-3.35260583073571,-1.,-2.52982887637028));
#42064=CARTESIAN_POINT('',(-3.44202241512147,-1.,-2.40675750623143));
#42065=CARTESIAN_POINT('',(-2.90994629141676,-1.,-2.36531447826073));
#42066=CARTESIAN_POINT('Ctrl Pts',(-3.35260583073571,-1.,-2.52982887637028));
#42067=CARTESIAN_POINT('Ctrl Pts',(-3.35105973714071,-1.,-2.5295413654909));
#42068=CARTESIAN_POINT('Ctrl Pts',(-3.34796903576663,-1.,-2.52896321610703));
#42069=CARTESIAN_POINT('Ctrl Pts',(-3.34333744115511,-1.,-2.52808660915689));
#42070=CARTESIAN_POINT('Ctrl Pts',(-3.33717089999103,-1.,-2.52689902690158));
#42071=CARTESIAN_POINT('Ctrl Pts',(-3.32947762187533,-1.,-2.52538321164634));
#42072=CARTESIAN_POINT('Ctrl Pts',(-3.32179931078699,-1.,-2.5238359839626));
#42073=CARTESIAN_POINT('Ctrl Pts',(-3.31413607874645,-1.,-2.52225724871313));
#42074=CARTESIAN_POINT('Ctrl Pts',(-3.30648808815442,-1.,-2.52064689568511));
#42075=CARTESIAN_POINT('Ctrl Pts',(-3.29885556388352,-1.,-2.51900480701069));
#42076=CARTESIAN_POINT('Ctrl Pts',(-3.2912387729927,-1.,-2.51733085123797));
#42077=CARTESIAN_POINT('Ctrl Pts',(-3.28363799702982,-1.,-2.51562487464514));
#42078=CARTESIAN_POINT('Ctrl Pts',(-3.27605350473142,-1.,-2.513886692704));
#42079=CARTESIAN_POINT('Ctrl Pts',(-3.26848552888115,-1.,-2.51211608411423));
#42080=CARTESIAN_POINT('Ctrl Pts',(-3.26093423001434,-1.,-2.51031277813486));
#42081=CARTESIAN_POINT('Ctrl Pts',(-3.25339971460982,-1.,-2.50847647070723));
#42082=CARTESIAN_POINT('Ctrl Pts',(-3.24588208983849,-1.,-2.506606859405));
#42083=CARTESIAN_POINT('Ctrl Pts',(-3.23838151080319,-1.,-2.5047036758003));
#42084=CARTESIAN_POINT('Ctrl Pts',(-3.23089822320646,-1.,-2.50276671338111));
#42085=CARTESIAN_POINT('Ctrl Pts',(-3.22343262620503,-1.,-2.50079587201957));
#42086=CARTESIAN_POINT('Ctrl Pts',(-3.21598526261286,-1.,-2.4987911459939));
#42087=CARTESIAN_POINT('Ctrl Pts',(-3.20855669849836,-1.,-2.4967525264737));
#42088=CARTESIAN_POINT('Ctrl Pts',(-3.20114742397588,-1.,-2.49467992057755));
#42089=CARTESIAN_POINT('Ctrl Pts',(-3.19375775555798,-1.,-2.49257307239848));
#42090=CARTESIAN_POINT('Ctrl Pts',(-3.18638771282266,-1.,-2.49043146334059));
#42091=CARTESIAN_POINT('Ctrl Pts',(-3.17903698136622,-1.,-2.48825428288201));
#42092=CARTESIAN_POINT('Ctrl Pts',(-3.17170518863313,-1.,-2.48604065348587));
#42093=CARTESIAN_POINT('Ctrl Pts',(-3.16439213290161,-1.,-2.48378981792725));
#42094=CARTESIAN_POINT('Ctrl Pts',(-3.15709802322739,-1.,-2.48150133566571));
#42095=CARTESIAN_POINT('Ctrl Pts',(-3.14982373241352,-1.,-2.47917529057029));
#42096=CARTESIAN_POINT('Ctrl Pts',(-3.1425709954655,-1.,-2.47681245356109));
#42097=CARTESIAN_POINT('Ctrl Pts',(-3.13534181229295,-1.,-2.47441378371932));
#42098=CARTESIAN_POINT('Ctrl Pts',(-3.12813790805952,-1.,-2.47197997765871));
#42099=CARTESIAN_POINT('Ctrl Pts',(-3.12096015766983,-1.,-2.46951098947469));
#42100=CARTESIAN_POINT('Ctrl Pts',(-3.11380805536122,-1.,-2.46700558843506));
#42101=CARTESIAN_POINT('Ctrl Pts',(-3.1066790790198,-1.,-2.46446082979646));
#42102=CARTESIAN_POINT('Ctrl Pts',(-3.09956993697052,-1.,-2.46187308501884));
#42103=CARTESIAN_POINT('Ctrl Pts',(-3.09247787931887,-1.,-2.4592391256388));
#42104=CARTESIAN_POINT('Ctrl Pts',(-3.08540206545315,-1.,-2.45655725437039));
#42105=CARTESIAN_POINT('Ctrl Pts',(-3.07834472886139,-1.,-2.4538282678779));
#42106=CARTESIAN_POINT('Ctrl Pts',(-3.07131290521297,-1.,-2.45105688854422));
#42107=CARTESIAN_POINT('Ctrl Pts',(-3.06431596421405,-1.,-2.44824970516544));
#42108=CARTESIAN_POINT('Ctrl Pts',(-3.05736242671506,-1.,-2.44541251892556));
#42109=CARTESIAN_POINT('Ctrl Pts',(-3.05045678021504,-1.,-2.44254768923105));
#42110=CARTESIAN_POINT('Ctrl Pts',(-3.04359685040555,-1.,-2.43965194061857));
#42111=CARTESIAN_POINT('Ctrl Pts',(-3.03676949672821,-1.,-2.43671278042414));
#42112=CARTESIAN_POINT('Ctrl Pts',(-3.02995534946978,-1.,-2.43371241361488));
#42113=CARTESIAN_POINT('Ctrl Pts',(-3.02313656036004,-1.,-2.43063415586637));
#42114=CARTESIAN_POINT('Ctrl Pts',(-3.01630420830504,-1.,-2.42746856264168));
#42115=CARTESIAN_POINT('Ctrl Pts',(-3.00946442616658,-1.,-2.42421849439613));
#42116=CARTESIAN_POINT('Ctrl Pts',(-3.00264868585996,-1.,-2.42090763946779));
#42117=CARTESIAN_POINT('Ctrl Pts',(-2.99590509293503,-1.,-2.41757324500514));
#42118=CARTESIAN_POINT('Ctrl Pts',(-2.98927983005796,-1.,-2.41425064199586));
#42119=CARTESIAN_POINT('Ctrl Pts',(-2.98280015815107,-1.,-2.41095909342571));
#42120=CARTESIAN_POINT('Ctrl Pts',(-2.97646002822422,-1.,-2.40768975073713));
#42121=CARTESIAN_POINT('Ctrl Pts',(-2.9701964131236,-1.,-2.40438604734919));
#42122=CARTESIAN_POINT('Ctrl Pts',(-2.96390432240312,-1.,-2.4009556571164));
#42123=CARTESIAN_POINT('Ctrl Pts',(-2.95748006482942,-1.,-2.39730553974517));
#42124=CARTESIAN_POINT('Ctrl Pts',(-2.95085857128439,-1.,-2.39337207631667));
#42125=CARTESIAN_POINT('Ctrl Pts',(-2.94404820669076,-1.,-2.38914929090759));
#42126=CARTESIAN_POINT('Ctrl Pts',(-2.93717903280391,-1.,-2.38472771516311));
#42127=CARTESIAN_POINT('Ctrl Pts',(-2.93049643640206,-1.,-2.38028989582073));
#42128=CARTESIAN_POINT('Ctrl Pts',(-2.92430340582608,-1.,-2.3760651052403));
#42129=CARTESIAN_POINT('Ctrl Pts',(-2.91891503791411,-1.,-2.37229381109821));
#42130=CARTESIAN_POINT('Ctrl Pts',(-2.9146124988314,-1.,-2.36919161373173));
#42131=CARTESIAN_POINT('Ctrl Pts',(-2.91181344022549,-1.,-2.36707658451664));
#42132=CARTESIAN_POINT('Ctrl Pts',(-2.91051690822156,-1.,-2.36599991765749));
#42133=CARTESIAN_POINT('Ctrl Pts',(-2.91005770527719,-1.,-2.36553202948613));
#42134=CARTESIAN_POINT('Ctrl Pts',(-2.90995756655606,-1.,-2.36536211188453));
#42135=CARTESIAN_POINT('Ctrl Pts',(-2.90994629141676,-1.,-2.36531447826074));
#42136=CARTESIAN_POINT('',(-2.79140942341378,-1.,-2.50410331873042));
#42137=CARTESIAN_POINT('Origin',(0.,-1.,0.));
#42138=CARTESIAN_POINT('',(-3.02314558451372,-1.,-2.91557726271063));
#42139=CARTESIAN_POINT('Ctrl Pts',(-2.79140942341378,-1.,-2.50410331873042));
#42140=CARTESIAN_POINT('Ctrl Pts',(-2.79145823440899,-1.,-2.50410700351426));
#42141=CARTESIAN_POINT('Ctrl Pts',(-2.79164172519039,-1.,-2.50417932839343));
#42142=CARTESIAN_POINT('Ctrl Pts',(-2.79217568804874,-1.,-2.50455968395235));
#42143=CARTESIAN_POINT('Ctrl Pts',(-2.79344192164204,-1.,-2.50567182569153));
#42144=CARTESIAN_POINT('Ctrl Pts',(-2.7959687805717,-1.,-2.50810555977564));
#42145=CARTESIAN_POINT('Ctrl Pts',(-2.79970585014308,-1.,-2.51186983687947));
#42146=CARTESIAN_POINT('Ctrl Pts',(-2.80427363984939,-1.,-2.51660190466067));
#42147=CARTESIAN_POINT('Ctrl Pts',(-2.80941521967234,-1.,-2.52205778589922));
#42148=CARTESIAN_POINT('Ctrl Pts',(-2.8148437904867,-1.,-2.52796388055457));
#42149=CARTESIAN_POINT('Ctrl Pts',(-2.82028550483744,-1.,-2.53405679667463));
#42150=CARTESIAN_POINT('Ctrl Pts',(-2.82552167649157,-1.,-2.54012272520141));
#42151=CARTESIAN_POINT('Ctrl Pts',(-2.83044254225794,-1.,-2.54604736792542));
#42152=CARTESIAN_POINT('Ctrl Pts',(-2.83505269592412,-1.,-2.55182152806964));
#42153=CARTESIAN_POINT('Ctrl Pts',(-2.83942515220699,-1.,-2.55749952145165));
#42154=CARTESIAN_POINT('Ctrl Pts',(-2.84366802680211,-1.,-2.56316920798489));
#42155=CARTESIAN_POINT('Ctrl Pts',(-2.84788893329091,-1.,-2.56891984251743));
#42156=CARTESIAN_POINT('Ctrl Pts',(-2.85215360144483,-1.,-2.57480482727128));
#42157=CARTESIAN_POINT('Ctrl Pts',(-2.85647171715147,-1.,-2.58082875254407));
#42158=CARTESIAN_POINT('Ctrl Pts',(-2.86081999003668,-1.,-2.5869677064356));
#42159=CARTESIAN_POINT('Ctrl Pts',(-2.86515629953528,-1.,-2.59318160184921));
#42160=CARTESIAN_POINT('Ctrl Pts',(-2.86943633170712,-1.,-2.59942875223202));
#42161=CARTESIAN_POINT('Ctrl Pts',(-2.87363176656475,-1.,-2.6056817788128));
#42162=CARTESIAN_POINT('Ctrl Pts',(-2.87773881947885,-1.,-2.61193507170928));
#42163=CARTESIAN_POINT('Ctrl Pts',(-2.88176821427502,-1.,-2.61819596473087));
#42164=CARTESIAN_POINT('Ctrl Pts',(-2.88573922195049,-1.,-2.62447947640253));
#42165=CARTESIAN_POINT('Ctrl Pts',(-2.88967244854243,-1.,-2.63080195420771));
#42166=CARTESIAN_POINT('Ctrl Pts',(-2.89358228854557,-1.,-2.63717442263944));
#42167=CARTESIAN_POINT('Ctrl Pts',(-2.89747231723361,-1.,-2.64359851684146));
#42168=CARTESIAN_POINT('Ctrl Pts',(-2.90133950224879,-1.,-2.65007017365576));
#42169=CARTESIAN_POINT('Ctrl Pts',(-2.90517678087467,-1.,-2.65658188464287));
#42170=CARTESIAN_POINT('Ctrl Pts',(-2.90897617968921,-1.,-2.66312542616808));
#42171=CARTESIAN_POINT('Ctrl Pts',(-2.91273193382876,-1.,-2.66969458792627));
#42172=CARTESIAN_POINT('Ctrl Pts',(-2.91644290704281,-1.,-2.67628728855309));
#42173=CARTESIAN_POINT('Ctrl Pts',(-2.92011090722152,-1.,-2.68290409279689));
#42174=CARTESIAN_POINT('Ctrl Pts',(-2.92373955325876,-1.,-2.68954721165342));
#42175=CARTESIAN_POINT('Ctrl Pts',(-2.92733294395268,-1.,-2.69621932864302));
#42176=CARTESIAN_POINT('Ctrl Pts',(-2.93089438233746,-1.,-2.70292247416881));
#42177=CARTESIAN_POINT('Ctrl Pts',(-2.93442516311168,-1.,-2.70965695523776));
#42178=CARTESIAN_POINT('Ctrl Pts',(-2.93792519474955,-1.,-2.71642190053575));
#42179=CARTESIAN_POINT('Ctrl Pts',(-2.94139351933882,-1.,-2.72321571511322));
#42180=CARTESIAN_POINT('Ctrl Pts',(-2.94482887675139,-1.,-2.73003657371613));
#42181=CARTESIAN_POINT('Ctrl Pts',(-2.94823023414381,-1.,-2.73688288329825));
#42182=CARTESIAN_POINT('Ctrl Pts',(-2.95159737214305,-1.,-2.7437537949221));
#42183=CARTESIAN_POINT('Ctrl Pts',(-2.95493069316211,-1.,-2.75064903318996));
#42184=CARTESIAN_POINT('Ctrl Pts',(-2.9582309766594,-1.,-2.75756867888393));
#42185=CARTESIAN_POINT('Ctrl Pts',(-2.96149914764832,-1.,-2.76451296269571));
#42186=CARTESIAN_POINT('Ctrl Pts',(-2.96473605585548,-1.,-2.77148206836464));
#42187=CARTESIAN_POINT('Ctrl Pts',(-2.9679422104295,-1.,-2.77847589542767));
#42188=CARTESIAN_POINT('Ctrl Pts',(-2.97111781461349,-1.,-2.78549409123657));
#42189=CARTESIAN_POINT('Ctrl Pts',(-2.97426288347475,-1.,-2.79253615718147));
#42190=CARTESIAN_POINT('Ctrl Pts',(-2.97737733718242,-1.,-2.79960153278186));
#42191=CARTESIAN_POINT('Ctrl Pts',(-2.98046109647299,-1.,-2.80668968101162));
#42192=CARTESIAN_POINT('Ctrl Pts',(-2.9835141977994,-1.,-2.81380019196454));
#42193=CARTESIAN_POINT('Ctrl Pts',(-2.98653680669434,-1.,-2.82093279065704));
#42194=CARTESIAN_POINT('Ctrl Pts',(-2.98952916401699,-1.,-2.82808728190402));
#42195=CARTESIAN_POINT('Ctrl Pts',(-2.99249155170479,-1.,-2.83526351254383));
#42196=CARTESIAN_POINT('Ctrl Pts',(-2.995424253416,-1.,-2.84246132984334));
#42197=CARTESIAN_POINT('Ctrl Pts',(-2.99832751144566,-1.,-2.84968053289104));
#42198=CARTESIAN_POINT('Ctrl Pts',(-3.0012015079552,-1.,-2.85692085715129));
#42199=CARTESIAN_POINT('Ctrl Pts',(-3.00404638316245,-1.,-2.86418200833065));
#42200=CARTESIAN_POINT('Ctrl Pts',(-3.00686224485374,-1.,-2.87146368430104));
#42201=CARTESIAN_POINT('Ctrl Pts',(-3.0096491810855,-1.,-2.87876560072799));
#42202=CARTESIAN_POINT('Ctrl Pts',(-3.01240727309568,-1.,-2.88608751706796));
#42203=CARTESIAN_POINT('Ctrl Pts',(-3.01513660433291,-1.,-2.8934292556764));
#42204=CARTESIAN_POINT('Ctrl Pts',(-3.01783725123646,-1.,-2.90079069102661));
#42205=CARTESIAN_POINT('Ctrl Pts',(-3.01997487194926,-1.,-2.90669553303902));
#42206=CARTESIAN_POINT('Ctrl Pts',(-3.02156522743299,-1.,-2.91113297349052));
#42207=CARTESIAN_POINT('Ctrl Pts',(-3.02261975104912,-1.,-2.91409518070707));
#42208=CARTESIAN_POINT('Ctrl Pts',(-3.02314558451372,-1.,-2.91557726271063));
#42209=CARTESIAN_POINT('',(-2.91557726271063,-1.,-3.02314558451372));
#42210=CARTESIAN_POINT('',(-3.02314558451372,-1.,-2.91557726271063));
#42211=CARTESIAN_POINT('',(-2.50410331873176,-1.,-2.79140942341258));
#42212=CARTESIAN_POINT('Ctrl Pts',(-2.91557726271063,-1.,-3.02314558451372));
#42213=CARTESIAN_POINT('Ctrl Pts',(-2.91409518070399,-1.,-3.02261975104593));
#42214=CARTESIAN_POINT('Ctrl Pts',(-2.91113297348212,-1.,-3.02156522742431));
#42215=CARTESIAN_POINT('Ctrl Pts',(-2.90669553302526,-1.,-3.01997487193503));
#42216=CARTESIAN_POINT('Ctrl Pts',(-2.9007906910105,-1.,-3.01783725121981));
#42217=CARTESIAN_POINT('Ctrl Pts',(-2.89342925566321,-1.,-3.01513660431928));
#42218=CARTESIAN_POINT('Ctrl Pts',(-2.8860875170608,-1.,-3.01240727308829));
#42219=CARTESIAN_POINT('Ctrl Pts',(-2.87876560072727,-1.,-3.00964918108476));
#42220=CARTESIAN_POINT('Ctrl Pts',(-2.87146368430502,-1.,-3.00686224485784));
#42221=CARTESIAN_POINT('Ctrl Pts',(-2.86418200833667,-1.,-3.00404638316867));
#42222=CARTESIAN_POINT('Ctrl Pts',(-2.85692085715686,-1.,-3.00120150796095));
#42223=CARTESIAN_POINT('Ctrl Pts',(-2.84968053289451,-1.,-2.99832751144925));
#42224=CARTESIAN_POINT('Ctrl Pts',(-2.84246132984415,-1.,-2.99542425341685));
#42225=CARTESIAN_POINT('Ctrl Pts',(-2.83526351254248,-1.,-2.99249155170339));
#42226=CARTESIAN_POINT('Ctrl Pts',(-2.82808728190157,-1.,-2.98952916401446));
#42227=CARTESIAN_POINT('Ctrl Pts',(-2.82093279065457,-1.,-2.9865368066918));
#42228=CARTESIAN_POINT('Ctrl Pts',(-2.81380019196286,-1.,-2.98351419779767));
#42229=CARTESIAN_POINT('Ctrl Pts',(-2.80668968101106,-1.,-2.98046109647241));
#42230=CARTESIAN_POINT('Ctrl Pts',(-2.7996015327823,-1.,-2.97737733718287));
#42231=CARTESIAN_POINT('Ctrl Pts',(-2.79253615718248,-1.,-2.9742628834758));
#42232=CARTESIAN_POINT('Ctrl Pts',(-2.78549409123769,-1.,-2.97111781461465));
#42233=CARTESIAN_POINT('Ctrl Pts',(-2.7784758954285,-1.,-2.96794221043036));
#42234=CARTESIAN_POINT('Ctrl Pts',(-2.77148206836498,-1.,-2.96473605585583));
#42235=CARTESIAN_POINT('Ctrl Pts',(-2.76451296269557,-1.,-2.96149914764818));
#42236=CARTESIAN_POINT('Ctrl Pts',(-2.7575686788835,-1.,-2.95823097665896));
#42237=CARTESIAN_POINT('Ctrl Pts',(-2.75064903318947,-1.,-2.95493069316161));
#42238=CARTESIAN_POINT('Ctrl Pts',(-2.74375379492172,-1.,-2.95159737214266));
#42239=CARTESIAN_POINT('Ctrl Pts',(-2.73688288329808,-1.,-2.94823023414364));
#42240=CARTESIAN_POINT('Ctrl Pts',(-2.73003657371617,-1.,-2.94482887675143));
#42241=CARTESIAN_POINT('Ctrl Pts',(-2.72321571511337,-1.,-2.94139351933897));
#42242=CARTESIAN_POINT('Ctrl Pts',(-2.71642190053592,-1.,-2.93792519474972));
#42243=CARTESIAN_POINT('Ctrl Pts',(-2.70965695523787,-1.,-2.93442516311179));
#42244=CARTESIAN_POINT('Ctrl Pts',(-2.70292247416885,-1.,-2.93089438233749));
#42245=CARTESIAN_POINT('Ctrl Pts',(-2.69621932864301,-1.,-2.92733294395267));
#42246=CARTESIAN_POINT('Ctrl Pts',(-2.68954721165339,-1.,-2.92373955325875));
#42247=CARTESIAN_POINT('Ctrl Pts',(-2.68290409279688,-1.,-2.92011090722152));
#42248=CARTESIAN_POINT('Ctrl Pts',(-2.67628728855312,-1.,-2.91644290704285));
#42249=CARTESIAN_POINT('Ctrl Pts',(-2.66969458792631,-1.,-2.91273193382882));
#42250=CARTESIAN_POINT('Ctrl Pts',(-2.6631254261681,-1.,-2.90897617968923));
#42251=CARTESIAN_POINT('Ctrl Pts',(-2.65658188464282,-1.,-2.90517678087461));
#42252=CARTESIAN_POINT('Ctrl Pts',(-2.65007017365564,-1.,-2.90133950224867));
#42253=CARTESIAN_POINT('Ctrl Pts',(-2.64359851684131,-1.,-2.89747231723345));
#42254=CARTESIAN_POINT('Ctrl Pts',(-2.63717442263932,-1.,-2.89358228854544));
#42255=CARTESIAN_POINT('Ctrl Pts',(-2.63080195420767,-1.,-2.88967244854239));
#42256=CARTESIAN_POINT('Ctrl Pts',(-2.62447947640262,-1.,-2.88573922195059));
#42257=CARTESIAN_POINT('Ctrl Pts',(-2.61819596473108,-1.,-2.88176821427525));
#42258=CARTESIAN_POINT('Ctrl Pts',(-2.61193507170955,-1.,-2.87773881947915));
#42259=CARTESIAN_POINT('Ctrl Pts',(-2.60568177881303,-1.,-2.87363176656501));
#42260=CARTESIAN_POINT('Ctrl Pts',(-2.5994287522321,-1.,-2.86943633170722));
#42261=CARTESIAN_POINT('Ctrl Pts',(-2.59318160184908,-1.,-2.86515629953513));
#42262=CARTESIAN_POINT('Ctrl Pts',(-2.58696770643524,-1.,-2.86081999003629));
#42263=CARTESIAN_POINT('Ctrl Pts',(-2.58082875254357,-1.,-2.85647171715092));
#42264=CARTESIAN_POINT('Ctrl Pts',(-2.57480482727081,-1.,-2.85215360144431));
#42265=CARTESIAN_POINT('Ctrl Pts',(-2.56891984251721,-1.,-2.84788893329067));
#42266=CARTESIAN_POINT('Ctrl Pts',(-2.56316920798513,-1.,-2.84366802680237));
#42267=CARTESIAN_POINT('Ctrl Pts',(-2.55749952145241,-1.,-2.83942515220782));
#42268=CARTESIAN_POINT('Ctrl Pts',(-2.55182152807077,-1.,-2.83505269592536));
#42269=CARTESIAN_POINT('Ctrl Pts',(-2.54604736792655,-1.,-2.83044254225917));
#42270=CARTESIAN_POINT('Ctrl Pts',(-2.54012272520199,-1.,-2.8255216764922));
#42271=CARTESIAN_POINT('Ctrl Pts',(-2.53405679667412,-1.,-2.82028550483689));
#42272=CARTESIAN_POINT('Ctrl Pts',(-2.52796388055278,-1.,-2.81484379048475));
#42273=CARTESIAN_POINT('Ctrl Pts',(-2.52205778589653,-1.,-2.80941521966941));
#42274=CARTESIAN_POINT('Ctrl Pts',(-2.51660190465805,-1.,-2.80427363984653));
#42275=CARTESIAN_POINT('Ctrl Pts',(-2.51186983687818,-1.,-2.79970585014168));
#42276=CARTESIAN_POINT('Ctrl Pts',(-2.50810555977671,-1.,-2.79596878057287));
#42277=CARTESIAN_POINT('Ctrl Pts',(-2.50567182569081,-1.,-2.79344192164147));
#42278=CARTESIAN_POINT('Ctrl Pts',(-2.50455968395146,-1.,-2.79217568804755));
#42279=CARTESIAN_POINT('Ctrl Pts',(-2.50417932839313,-1.,-2.79164172518905));
#42280=CARTESIAN_POINT('Ctrl Pts',(-2.50410700351493,-1.,-2.79145823440781));
#42281=CARTESIAN_POINT('Ctrl Pts',(-2.50410331873176,-1.,-2.79140942341258));
#42282=CARTESIAN_POINT('',(-2.36531447826213,-1.,-2.90994629141562));
#42283=CARTESIAN_POINT('Origin',(0.,-1.,0.));
#42284=CARTESIAN_POINT('',(-2.52982887637028,-1.,-3.35260583073571));
#42285=CARTESIAN_POINT('Ctrl Pts',(-2.36531447826213,-1.,-2.90994629141562));
#42286=CARTESIAN_POINT('Ctrl Pts',(-2.3653621118858,-1.,-2.90995756655558));
#42287=CARTESIAN_POINT('Ctrl Pts',(-2.36553202948741,-1.,-2.9100577052777));
#42288=CARTESIAN_POINT('Ctrl Pts',(-2.36599991765853,-1.,-2.91051690822262));
#42289=CARTESIAN_POINT('Ctrl Pts',(-2.36707658451709,-1.,-2.91181344022628));
#42290=CARTESIAN_POINT('Ctrl Pts',(-2.36919161373074,-1.,-2.91461249883016));
#42291=CARTESIAN_POINT('Ctrl Pts',(-2.37229381109939,-1.,-2.9189150379156));
#42292=CARTESIAN_POINT('Ctrl Pts',(-2.37606510524271,-1.,-2.92430340582912));
#42293=CARTESIAN_POINT('Ctrl Pts',(-2.3802898958232,-1.,-2.93049643640517));
#42294=CARTESIAN_POINT('Ctrl Pts',(-2.38472771516476,-1.,-2.93717903280599));
#42295=CARTESIAN_POINT('Ctrl Pts',(-2.38914929090806,-1.,-2.94404820669135));
#42296=CARTESIAN_POINT('Ctrl Pts',(-2.39337207631613,-1.,-2.95085857128372));
#42297=CARTESIAN_POINT('Ctrl Pts',(-2.39730553974412,-1.,-2.95748006482811));
#42298=CARTESIAN_POINT('Ctrl Pts',(-2.40095565711535,-1.,-2.96390432240181));
#42299=CARTESIAN_POINT('Ctrl Pts',(-2.40438604734848,-1.,-2.97019641312272));
#42300=CARTESIAN_POINT('Ctrl Pts',(-2.40768975073691,-1.,-2.97646002822395));
#42301=CARTESIAN_POINT('Ctrl Pts',(-2.41095909342591,-1.,-2.98280015815132));
#42302=CARTESIAN_POINT('Ctrl Pts',(-2.4142506419963,-1.,-2.98927983005851));
#42303=CARTESIAN_POINT('Ctrl Pts',(-2.4175732450056,-1.,-2.99590509293561));
#42304=CARTESIAN_POINT('Ctrl Pts',(-2.42090763946812,-1.,-3.00264868586038));
#42305=CARTESIAN_POINT('Ctrl Pts',(-2.42421849439625,-1.,-3.00946442616674));
#42306=CARTESIAN_POINT('Ctrl Pts',(-2.4274685626416,-1.,-3.01630420830494));
#42307=CARTESIAN_POINT('Ctrl Pts',(-2.43063415586615,-1.,-3.02313656035977));
#42308=CARTESIAN_POINT('Ctrl Pts',(-2.43371241361462,-1.,-3.02995534946946));
#42309=CARTESIAN_POINT('Ctrl Pts',(-2.43671278042394,-1.,-3.03676949672797));
#42310=CARTESIAN_POINT('Ctrl Pts',(-2.43965194061849,-1.,-3.04359685040545));
#42311=CARTESIAN_POINT('Ctrl Pts',(-2.44254768923109,-1.,-3.05045678021509));
#42312=CARTESIAN_POINT('Ctrl Pts',(-2.44541251892568,-1.,-3.05736242671521));
#42313=CARTESIAN_POINT('Ctrl Pts',(-2.44824970516558,-1.,-3.06431596421422));
#42314=CARTESIAN_POINT('Ctrl Pts',(-2.45105688854432,-1.,-3.0713129052131));
#42315=CARTESIAN_POINT('Ctrl Pts',(-2.45382826787795,-1.,-3.07834472886145));
#42316=CARTESIAN_POINT('Ctrl Pts',(-2.45655725437037,-1.,-3.08540206545313));
#42317=CARTESIAN_POINT('Ctrl Pts',(-2.45923912563875,-1.,-3.09247787931881));
#42318=CARTESIAN_POINT('Ctrl Pts',(-2.4618730850188,-1.,-3.09956993697048));
#42319=CARTESIAN_POINT('Ctrl Pts',(-2.46446082979645,-1.,-3.10667907901981));
#42320=CARTESIAN_POINT('Ctrl Pts',(-2.46700558843507,-1.,-3.11380805536124));
#42321=CARTESIAN_POINT('Ctrl Pts',(-2.4695109894747,-1.,-3.12096015766984));
#42322=CARTESIAN_POINT('Ctrl Pts',(-2.47197997765868,-1.,-3.12813790805948));
#42323=CARTESIAN_POINT('Ctrl Pts',(-2.47441378371923,-1.,-3.13534181229282));
#42324=CARTESIAN_POINT('Ctrl Pts',(-2.47681245356095,-1.,-3.14257099546531));
#42325=CARTESIAN_POINT('Ctrl Pts',(-2.47917529057016,-1.,-3.14982373241335));
#42326=CARTESIAN_POINT('Ctrl Pts',(-2.48150133566568,-1.,-3.15709802322735));
#42327=CARTESIAN_POINT('Ctrl Pts',(-2.48378981792739,-1.,-3.16439213290181));
#42328=CARTESIAN_POINT('Ctrl Pts',(-2.48604065348619,-1.,-3.17170518863357));
#42329=CARTESIAN_POINT('Ctrl Pts',(-2.48825428288243,-1.,-3.17903698136679));
#42330=CARTESIAN_POINT('Ctrl Pts',(-2.49043146334095,-1.,-3.18638771282315));
#42331=CARTESIAN_POINT('Ctrl Pts',(-2.4925730723986,-1.,-3.19375775555814));
#42332=CARTESIAN_POINT('Ctrl Pts',(-2.49467992057726,-1.,-3.20114742397549));
#42333=CARTESIAN_POINT('Ctrl Pts',(-2.49675252647298,-1.,-3.2085566984974));
#42334=CARTESIAN_POINT('Ctrl Pts',(-2.49879114599293,-1.,-3.21598526261157));
#42335=CARTESIAN_POINT('Ctrl Pts',(-2.5007958720187,-1.,-3.22343262620387));
#42336=CARTESIAN_POINT('Ctrl Pts',(-2.50276671338074,-1.,-3.23089822320596));
#42337=CARTESIAN_POINT('Ctrl Pts',(-2.50470367580078,-1.,-3.23838151080383));
#42338=CARTESIAN_POINT('Ctrl Pts',(-2.50660685940645,-1.,-3.24588208984042));
#42339=CARTESIAN_POINT('Ctrl Pts',(-2.50847647070936,-1.,-3.25339971461265));
#42340=CARTESIAN_POINT('Ctrl Pts',(-2.51031277813697,-1.,-3.26093423001716));
#42341=CARTESIAN_POINT('Ctrl Pts',(-2.51211608411539,-1.,-3.26848552888271));
#42342=CARTESIAN_POINT('Ctrl Pts',(-2.51388669270329,-1.,-3.27605350473048));
#42343=CARTESIAN_POINT('Ctrl Pts',(-2.51562487464215,-1.,-3.28363799702583));
#42344=CARTESIAN_POINT('Ctrl Pts',(-2.51733085123316,-1.,-3.2912387729863));
#42345=CARTESIAN_POINT('Ctrl Pts',(-2.51900480700548,-1.,-3.29885556387661));
#42346=CARTESIAN_POINT('Ctrl Pts',(-2.52064689568167,-1.,-3.30648808814986));
#42347=CARTESIAN_POINT('Ctrl Pts',(-2.52225724871375,-1.,-3.31413607874727));
#42348=CARTESIAN_POINT('Ctrl Pts',(-2.52383598396878,-1.,-3.32179931079521));
#42349=CARTESIAN_POINT('Ctrl Pts',(-2.52538321165774,-1.,-3.32947762189049));
#42350=CARTESIAN_POINT('Ctrl Pts',(-2.52689902691551,-1.,-3.33717090000955));
#42351=CARTESIAN_POINT('Ctrl Pts',(-2.52808660916879,-1.,-3.34333744117093));
#42352=CARTESIAN_POINT('Ctrl Pts',(-2.5289632161143,-1.,-3.34796903577628));
#42353=CARTESIAN_POINT('Ctrl Pts',(-2.52954136549357,-1.,-3.35105973714426));
#42354=CARTESIAN_POINT('Ctrl Pts',(-2.52982887637028,-1.,-3.35260583073571));
#42355=CARTESIAN_POINT('',(-2.40675750623143,-1.,-3.44202241512147));
#42356=CARTESIAN_POINT('',(-2.52982887637028,-1.,-3.35260583073571));
#42357=CARTESIAN_POINT('',(-2.03660101169715,-1.,-3.14877060440327));
#42358=CARTESIAN_POINT('Ctrl Pts',(-2.40675750623143,-1.,-3.44202241512147));
#42359=CARTESIAN_POINT('Ctrl Pts',(-2.4053759295909,-1.,-3.44127120683039));
#42360=CARTESIAN_POINT('Ctrl Pts',(-2.40261515589405,-1.,-3.43976627484234));
#42361=CARTESIAN_POINT('Ctrl Pts',(-2.39848113410292,-1.,-3.43750133064416));
#42362=CARTESIAN_POINT('Ctrl Pts',(-2.39298338804493,-1.,-3.4344663067854));
#42363=CARTESIAN_POINT('Ctrl Pts',(-2.38613505843552,-1.,-3.4306473271292));
#42364=CARTESIAN_POINT('Ctrl Pts',(-2.37931067028926,-1.,-3.42680309754399));
#42365=CARTESIAN_POINT('Ctrl Pts',(-2.37251035954292,-1.,-3.42293356216511));
#42366=CARTESIAN_POINT('Ctrl Pts',(-2.36573431470642,-1.,-3.41903866635852));
#42367=CARTESIAN_POINT('Ctrl Pts',(-2.35898278606946,-1.,-3.41511836751469));
#42368=CARTESIAN_POINT('Ctrl Pts',(-2.35225606824109,-1.,-3.41117262314119));
#42369=CARTESIAN_POINT('Ctrl Pts',(-2.34555447649188,-1.,-3.40720137404297));
#42370=CARTESIAN_POINT('Ctrl Pts',(-2.33887832342782,-1.,-3.40320452776743));
#42371=CARTESIAN_POINT('Ctrl Pts',(-2.33222789882489,-1.,-3.39918194577956));
#42372=CARTESIAN_POINT('Ctrl Pts',(-2.3256034390248,-1.,-3.39513342019756));
#42373=CARTESIAN_POINT('Ctrl Pts',(-2.31900513925424,-1.,-3.39105869474822));
#42374=CARTESIAN_POINT('Ctrl Pts',(-2.31243319489367,-1.,-3.38695751492462));
#42375=CARTESIAN_POINT('Ctrl Pts',(-2.30588783640343,-1.,-3.3828296733661));
#42376=CARTESIAN_POINT('Ctrl Pts',(-2.29936936127624,-1.,-3.37867504959433));
#42377=CARTESIAN_POINT('Ctrl Pts',(-2.29287818007393,-1.,-3.37449367172826));
#42378=CARTESIAN_POINT('Ctrl Pts',(-2.28641481081137,-1.,-3.37028570206488));
#42379=CARTESIAN_POINT('Ctrl Pts',(-2.27997979458037,-1.,-3.36605130713076));
#42380=CARTESIAN_POINT('Ctrl Pts',(-2.2735736262093,-1.,-3.36179055004409));
#42381=CARTESIAN_POINT('Ctrl Pts',(-2.2671966857991,-1.,-3.35750328523061));
#42382=CARTESIAN_POINT('Ctrl Pts',(-2.26084915222449,-1.,-3.35318902552626));
#42383=CARTESIAN_POINT('Ctrl Pts',(-2.25453097693483,-1.,-3.34884690292285));
#42384=CARTESIAN_POINT('Ctrl Pts',(-2.24824207678256,-1.,-3.34447596770723));
#42385=CARTESIAN_POINT('Ctrl Pts',(-2.24198249391422,-1.,-3.34007543738025));
#42386=CARTESIAN_POINT('Ctrl Pts',(-2.23575256328812,-1.,-3.33564495756482));
#42387=CARTESIAN_POINT('Ctrl Pts',(-2.22955308907233,-1.,-3.33118487773611));
#42388=CARTESIAN_POINT('Ctrl Pts',(-2.22338548312772,-1.,-3.3266964672289));
#42389=CARTESIAN_POINT('Ctrl Pts',(-2.21725135110898,-1.,-3.32218125618968));
#42390=CARTESIAN_POINT('Ctrl Pts',(-2.21115211847875,-1.,-3.31764044024235));
#42391=CARTESIAN_POINT('Ctrl Pts',(-2.20508863150607,-1.,-3.31307424608949));
#42392=CARTESIAN_POINT('Ctrl Pts',(-2.19906078949923,-1.,-3.30848134694595));
#42393=CARTESIAN_POINT('Ctrl Pts',(-2.19306710376111,-1.,-3.30385816281831));
#42394=CARTESIAN_POINT('Ctrl Pts',(-2.18710556500327,-1.,-3.29920022557639));
#42395=CARTESIAN_POINT('Ctrl Pts',(-2.18117455557065,-1.,-3.2945036150049));
#42396=CARTESIAN_POINT('Ctrl Pts',(-2.17527380048423,-1.,-3.28976645712568));
#42397=CARTESIAN_POINT('Ctrl Pts',(-2.16940517773455,-1.,-3.28499019979724));
#42398=CARTESIAN_POINT('Ctrl Pts',(-2.16357391934425,-1.,-3.280181508414));
#42399=CARTESIAN_POINT('Ctrl Pts',(-2.15778690038347,-1.,-3.27534954469187));
#42400=CARTESIAN_POINT('Ctrl Pts',(-2.15205043199808,-1.,-3.27050245897228));
#42401=CARTESIAN_POINT('Ctrl Pts',(-2.1463680529566,-1.,-3.26564388189759));
#42402=CARTESIAN_POINT('Ctrl Pts',(-2.14073870754264,-1.,-3.26077002641879));
#42403=CARTESIAN_POINT('Ctrl Pts',(-2.13515375878803,-1.,-3.25586495065054));
#42404=CARTESIAN_POINT('Ctrl Pts',(-2.12960028396832,-1.,-3.25090574494028));
#42405=CARTESIAN_POINT('Ctrl Pts',(-2.12406646410962,-1.,-3.24587102613376));
#42406=CARTESIAN_POINT('Ctrl Pts',(-2.11854673326979,-1.,-3.24074905517293));
#42407=CARTESIAN_POINT('Ctrl Pts',(-2.11304604021773,-1.,-3.23554444767099));
#42408=CARTESIAN_POINT('Ctrl Pts',(-2.10758699642451,-1.,-3.23028945793289));
#42409=CARTESIAN_POINT('Ctrl Pts',(-2.10220384298492,-1.,-3.22503437553434));
#42410=CARTESIAN_POINT('Ctrl Pts',(-2.09692958434895,-1.,-3.21982707347009));
#42411=CARTESIAN_POINT('Ctrl Pts',(-2.09178419460443,-1.,-3.21469429601654));
#42412=CARTESIAN_POINT('Ctrl Pts',(-2.08676465517455,-1.,-3.20962575845463));
#42413=CARTESIAN_POINT('Ctrl Pts',(-2.08182850370878,-1.,-3.2045481863073));
#42414=CARTESIAN_POINT('Ctrl Pts',(-2.07690441870722,-1.,-3.19934132836019));
#42415=CARTESIAN_POINT('Ctrl Pts',(-2.07192253497857,-1.,-3.19388465568252));
#42416=CARTESIAN_POINT('Ctrl Pts',(-2.06684062744112,-1.,-3.18809755562368));
#42417=CARTESIAN_POINT('Ctrl Pts',(-2.06166849827101,-1.,-3.18197692964614));
#42418=CARTESIAN_POINT('Ctrl Pts',(-2.05650186773132,-1.,-3.17564906975371));
#42419=CARTESIAN_POINT('Ctrl Pts',(-2.05151770247233,-1.,-3.16936341689527));
#42420=CARTESIAN_POINT('Ctrl Pts',(-2.04693331247446,-1.,-3.16343165058912));
#42421=CARTESIAN_POINT('Ctrl Pts',(-2.04297406404027,-1.,-3.15817983946367));
#42422=CARTESIAN_POINT('Ctrl Pts',(-2.03984073791519,-1.,-3.15389991674792));
#42423=CARTESIAN_POINT('Ctrl Pts',(-2.03783225495961,-1.,-3.15102344775328));
#42424=CARTESIAN_POINT('Ctrl Pts',(-2.03693188810544,-1.,-3.14959882629805));
#42425=CARTESIAN_POINT('Ctrl Pts',(-2.03663974554932,-1.,-3.1490119366901));
#42426=CARTESIAN_POINT('Ctrl Pts',(-2.03659701539259,-1.,-3.14881939088124));
#42427=CARTESIAN_POINT('Ctrl Pts',(-2.03660101169715,-1.,-3.14877060440328));
#42428=CARTESIAN_POINT('',(-1.88097764062697,-1.,-3.24413672884812));
#42429=CARTESIAN_POINT('Origin',(0.,-1.,0.));
#42430=CARTESIAN_POINT('',(-1.97421938526992,-1.,-3.70708211654725));
#42431=CARTESIAN_POINT('Ctrl Pts',(-1.88097764062697,-1.,-3.24413672884812));
#42432=CARTESIAN_POINT('Ctrl Pts',(-1.8810229239812,-1.,-3.24415531671284));
#42433=CARTESIAN_POINT('Ctrl Pts',(-1.88117508446775,-1.,-3.24428080353022));
#42434=CARTESIAN_POINT('Ctrl Pts',(-1.88156537699203,-1.,-3.24480754676064));
#42435=CARTESIAN_POINT('Ctrl Pts',(-1.88242596600454,-1.,-3.2462565441079));
#42436=CARTESIAN_POINT('Ctrl Pts',(-1.88407708646357,-1.,-3.24935200511918));
#42437=CARTESIAN_POINT('Ctrl Pts',(-1.88646802523466,-1.,-3.25408686339463));
#42438=CARTESIAN_POINT('Ctrl Pts',(-1.88934996203698,-1.,-3.25999885193947));
#42439=CARTESIAN_POINT('Ctrl Pts',(-1.89255393500965,-1.,-3.26677653888676));
#42440=CARTESIAN_POINT('Ctrl Pts',(-1.89589172903793,-1.,-3.27407108933139));
#42441=CARTESIAN_POINT('Ctrl Pts',(-1.89918429230462,-1.,-3.28154737912352));
#42442=CARTESIAN_POINT('Ctrl Pts',(-1.90228971247527,-1.,-3.2889344860029));
#42443=CARTESIAN_POINT('Ctrl Pts',(-1.90513891864087,-1.,-3.29608978722113));
#42444=CARTESIAN_POINT('Ctrl Pts',(-1.90773912171341,-1.,-3.30300595568195));
#42445=CARTESIAN_POINT('Ctrl Pts',(-1.91014297830446,-1.,-3.30975721158596));
#42446=CARTESIAN_POINT('Ctrl Pts',(-1.91242616234442,-1.,-3.31646052426364));
#42447=CARTESIAN_POINT('Ctrl Pts',(-1.91466343916628,-1.,-3.32323403454535));
#42448=CARTESIAN_POINT('Ctrl Pts',(-1.91690081930331,-1.,-3.33014884257873));
#42449=CARTESIAN_POINT('Ctrl Pts',(-1.9191460961021,-1.,-3.33721230710012));
#42450=CARTESIAN_POINT('Ctrl Pts',(-1.92138450828404,-1.,-3.34439448941961));
#42451=CARTESIAN_POINT('Ctrl Pts',(-1.92358838440528,-1.,-3.35164424847223));
#42452=CARTESIAN_POINT('Ctrl Pts',(-1.92572846125756,-1.,-3.35890824422965));
#42453=CARTESIAN_POINT('Ctrl Pts',(-1.92778626543786,-1.,-3.36615168657567));
#42454=CARTESIAN_POINT('Ctrl Pts',(-1.92975993109877,-1.,-3.37336807068043));
#42455=CARTESIAN_POINT('Ctrl Pts',(-1.93165739093276,-1.,-3.3805676852555));
#42456=CARTESIAN_POINT('Ctrl Pts',(-1.93349233176788,-1.,-3.38777076883256));
#42457=CARTESIAN_POINT('Ctrl Pts',(-1.93527929945985,-1.,-3.39499923640795));
#42458=CARTESIAN_POINT('Ctrl Pts',(-1.93702857723098,-1.,-3.40226802104109));
#42459=CARTESIAN_POINT('Ctrl Pts',(-1.93874306008143,-1.,-3.40957978266642));
#42460=CARTESIAN_POINT('Ctrl Pts',(-1.94042111965246,-1.,-3.41692971994096));
#42461=CARTESIAN_POINT('Ctrl Pts',(-1.94205835913696,-1.,-3.42430850941503));
#42462=CARTESIAN_POINT('Ctrl Pts',(-1.94364973660284,-1.,-3.43170586602434));
#42463=CARTESIAN_POINT('Ctrl Pts',(-1.94519168842879,-1.,-3.43911410197687));
#42464=CARTESIAN_POINT('Ctrl Pts',(-1.94668377715329,-1.,-3.44653088665681));
#42465=CARTESIAN_POINT('Ctrl Pts',(-1.94812754766524,-1.,-3.45395731584051));
#42466=CARTESIAN_POINT('Ctrl Pts',(-1.94952575850197,-1.,-3.46139661060962));
#42467=CARTESIAN_POINT('Ctrl Pts',(-1.95088147859877,-1.,-3.46885258974191));
#42468=CARTESIAN_POINT('Ctrl Pts',(-1.95219722189876,-1.,-3.47632820495921));
#42469=CARTESIAN_POINT('Ctrl Pts',(-1.95347412486309,-1.,-3.48382414832634));
#42470=CARTESIAN_POINT('Ctrl Pts',(-1.95471236969643,-1.,-3.49133956289133));
#42471=CARTESIAN_POINT('Ctrl Pts',(-1.95591153823661,-1.,-3.49887263575583));
#42472=CARTESIAN_POINT('Ctrl Pts',(-1.95707099606511,-1.,-3.50642124159909));
#42473=CARTESIAN_POINT('Ctrl Pts',(-1.95819025316779,-1.,-3.51398354617794));
#42474=CARTESIAN_POINT('Ctrl Pts',(-1.95926936324461,-1.,-3.52155867431486));
#42475=CARTESIAN_POINT('Ctrl Pts',(-1.96030879411566,-1.,-3.52914648844351));
#42476=CARTESIAN_POINT('Ctrl Pts',(-1.96130926212689,-1.,-3.53674730625813));
#42477=CARTESIAN_POINT('Ctrl Pts',(-1.96227157573067,-1.,-3.54436163300443));
#42478=CARTESIAN_POINT('Ctrl Pts',(-1.96319648628644,-1.,-3.55198990600886));
#42479=CARTESIAN_POINT('Ctrl Pts',(-1.96408450906812,-1.,-3.55963218706096));
#42480=CARTESIAN_POINT('Ctrl Pts',(-1.96493594634567,-1.,-3.56728820357791));
#42481=CARTESIAN_POINT('Ctrl Pts',(-1.96575096652789,-1.,-3.57495748600959));
#42482=CARTESIAN_POINT('Ctrl Pts',(-1.96652966688911,-1.,-3.58263947663829));
#42483=CARTESIAN_POINT('Ctrl Pts',(-1.96727213799544,-1.,-3.59033364022801));
#42484=CARTESIAN_POINT('Ctrl Pts',(-1.96797854118369,-1.,-3.59803959819938));
#42485=CARTESIAN_POINT('Ctrl Pts',(-1.9686491188594,-1.,-3.60575714017989));
#42486=CARTESIAN_POINT('Ctrl Pts',(-1.96928416040877,-1.,-3.61348615496704));
#42487=CARTESIAN_POINT('Ctrl Pts',(-1.96988398129978,-1.,-3.62122658401893));
#42488=CARTESIAN_POINT('Ctrl Pts',(-1.97044889850463,-1.,-3.62897836973293));
#42489=CARTESIAN_POINT('Ctrl Pts',(-1.97097920454464,-1.,-3.63674139590412));
#42490=CARTESIAN_POINT('Ctrl Pts',(-1.97147515441164,-1.,-3.64451546723514));
#42491=CARTESIAN_POINT('Ctrl Pts',(-1.9719369724024,-1.,-3.652300347166));
#42492=CARTESIAN_POINT('Ctrl Pts',(-1.9723648543905,-1.,-3.6600957816636));
#42493=CARTESIAN_POINT('Ctrl Pts',(-1.97275897198678,-1.,-3.66790152752075));
#42494=CARTESIAN_POINT('Ctrl Pts',(-1.97311947678517,-1.,-3.67571738107084));
#42495=CARTESIAN_POINT('Ctrl Pts',(-1.97344650304519,-1.,-3.68354319915092));
#42496=CARTESIAN_POINT('Ctrl Pts',(-1.97374016225483,-1.,-3.69137888599902));
#42497=CARTESIAN_POINT('Ctrl Pts',(-1.97394846383216,-1.,-3.6976552856004));
#42498=CARTESIAN_POINT('Ctrl Pts',(-1.97408973726715,-1.,-3.70236698912904));
#42499=CARTESIAN_POINT('Ctrl Pts',(-1.97417727645308,-1.,-3.70551008132332));
#42500=CARTESIAN_POINT('Ctrl Pts',(-1.97421938526992,-1.,-3.70708211654725));
#42501=CARTESIAN_POINT('',(-1.83867539237861,-1.,-3.77614523045147));
#42502=CARTESIAN_POINT('',(-1.97421938526992,-1.,-3.70708211654725));
#42503=CARTESIAN_POINT('',(-1.5189508286633,-1.,-3.42859860294306));
#42504=CARTESIAN_POINT('Ctrl Pts',(-1.83867539237861,-1.,-3.77614523045147));
#42505=CARTESIAN_POINT('Ctrl Pts',(-1.83742834010626,-1.,-3.77518714457833));
#42506=CARTESIAN_POINT('Ctrl Pts',(-1.83493697934534,-1.,-3.77326886064398));
#42507=CARTESIAN_POINT('Ctrl Pts',(-1.83120816955645,-1.,-3.77038509817999));
#42508=CARTESIAN_POINT('Ctrl Pts',(-1.82625289220915,-1.,-3.76652740353775));
#42509=CARTESIAN_POINT('Ctrl Pts',(-1.82008629694091,-1.,-3.76168412707948));
#42510=CARTESIAN_POINT('Ctrl Pts',(-1.8139472983358,-1.,-3.75681965683071));
#42511=CARTESIAN_POINT('Ctrl Pts',(-1.80783603939617,-1.,-3.75193395887977));
#42512=CARTESIAN_POINT('Ctrl Pts',(-1.8017527148577,-1.,-3.74702700875467));
#42513=CARTESIAN_POINT('Ctrl Pts',(-1.79569757859422,-1.,-3.74209880352445));
#42514=CARTESIAN_POINT('Ctrl Pts',(-1.78967092823491,-1.,-3.73714934730681));
#42515=CARTESIAN_POINT('Ctrl Pts',(-1.78367308442901,-1.,-3.7321786309547));
#42516=CARTESIAN_POINT('Ctrl Pts',(-1.77770437039658,-1.,-3.72718661205609));
#42517=CARTESIAN_POINT('Ctrl Pts',(-1.77176509401761,-1.,-3.72217319911254));
#42518=CARTESIAN_POINT('Ctrl Pts',(-1.76585552124394,-1.,-3.71713822377359));
#42519=CARTESIAN_POINT('Ctrl Pts',(-1.75997588498865,-1.,-3.71208146346136));
#42520=CARTESIAN_POINT('Ctrl Pts',(-1.75412641804042,-1.,-3.70700269736659));
#42521=CARTESIAN_POINT('Ctrl Pts',(-1.74830738046057,-1.,-3.7019017567335));
#42522=CARTESIAN_POINT('Ctrl Pts',(-1.74251908492617,-1.,-3.69677856910517));
#42523=CARTESIAN_POINT('Ctrl Pts',(-1.73676193254557,-1.,-3.69163322648036));
#42524=CARTESIAN_POINT('Ctrl Pts',(-1.73103640956717,-1.,-3.68646597019332));
#42525=CARTESIAN_POINT('Ctrl Pts',(-1.72534302437056,-1.,-3.68127704936579));
#42526=CARTESIAN_POINT('Ctrl Pts',(-1.71968225581808,-1.,-3.67606660374709));
#42527=CARTESIAN_POINT('Ctrl Pts',(-1.71405450210384,-1.,-3.67083454901611));
#42528=CARTESIAN_POINT('Ctrl Pts',(-1.70846001610956,-1.,-3.66558043198876));
#42529=CARTESIAN_POINT('Ctrl Pts',(-1.70289888566873,-1.,-3.66030338774847));
#42530=CARTESIAN_POINT('Ctrl Pts',(-1.69737117722534,-1.,-3.65500246526749));
#42531=CARTESIAN_POINT('Ctrl Pts',(-1.69187705481689,-1.,-3.64967689827371));
#42532=CARTESIAN_POINT('Ctrl Pts',(-1.68641690471457,-1.,-3.64432638915203));
#42533=CARTESIAN_POINT('Ctrl Pts',(-1.68099146651586,-1.,-3.63895140887462));
#42534=CARTESIAN_POINT('Ctrl Pts',(-1.67560193613156,-1.,-3.63355343201232));
#42535=CARTESIAN_POINT('Ctrl Pts',(-1.67024966008045,-1.,-3.62813422105271));
#42536=CARTESIAN_POINT('Ctrl Pts',(-1.66493585923855,-1.,-3.62269517989109));
#42537=CARTESIAN_POINT('Ctrl Pts',(-1.65966133399186,-1.,-3.61723666482456));
#42538=CARTESIAN_POINT('Ctrl Pts',(-1.65442619244325,-1.,-3.61175734965127));
#42539=CARTESIAN_POINT('Ctrl Pts',(-1.64922952425832,-1.,-3.60625346556992));
#42540=CARTESIAN_POINT('Ctrl Pts',(-1.64407004385582,-1.,-3.60072028513845));
#42541=CARTESIAN_POINT('Ctrl Pts',(-1.63894676675352,-1.,-3.59515368334893));
#42542=CARTESIAN_POINT('Ctrl Pts',(-1.6338597145126,-1.,-3.58955176627879));
#42543=CARTESIAN_POINT('Ctrl Pts',(-1.62881051550745,-1.,-3.58391625774343));
#42544=CARTESIAN_POINT('Ctrl Pts',(-1.62380329464844,-1.,-3.5782545595439));
#42545=CARTESIAN_POINT('Ctrl Pts',(-1.61884340915404,-1.,-3.57257679609806));
#42546=CARTESIAN_POINT('Ctrl Pts',(-1.61393581747514,-1.,-3.56689200468387));
#42547=CARTESIAN_POINT('Ctrl Pts',(-1.60908344685457,-1.,-3.5612043248298));
#42548=CARTESIAN_POINT('Ctrl Pts',(-1.60428584699853,-1.,-3.55550985096129));
#42549=CARTESIAN_POINT('Ctrl Pts',(-1.59953698113457,-1.,-3.54979148634454));
#42550=CARTESIAN_POINT('Ctrl Pts',(-1.59482766949766,-1.,-3.54402458182337));
#42551=CARTESIAN_POINT('Ctrl Pts',(-1.59014958368739,-1.,-3.53818616861077));
#42552=CARTESIAN_POINT('Ctrl Pts',(-1.58549906268088,-1.,-3.5322637814708));
#42553=CARTESIAN_POINT('Ctrl Pts',(-1.58088027227848,-1.,-3.52626275334881));
#42554=CARTESIAN_POINT('Ctrl Pts',(-1.57631049988158,-1.,-3.52021847865912));
#42555=CARTESIAN_POINT('Ctrl Pts',(-1.57181569799743,-1.,-3.51418598431665));
#42556=CARTESIAN_POINT('Ctrl Pts',(-1.56742097575012,-1.,-3.50821771695363));
#42557=CARTESIAN_POINT('Ctrl Pts',(-1.56314187758675,-1.,-3.50234321621578));
#42558=CARTESIAN_POINT('Ctrl Pts',(-1.55897703097874,-1.,-3.49655185179655));
#42559=CARTESIAN_POINT('Ctrl Pts',(-1.55489595901116,-1.,-3.4907646087742));
#42560=CARTESIAN_POINT('Ctrl Pts',(-1.55084702970452,-1.,-3.48485155928567));
#42561=CARTESIAN_POINT('Ctrl Pts',(-1.54678009290276,-1.,-3.47868272898751));
#42562=CARTESIAN_POINT('Ctrl Pts',(-1.54266605398187,-1.,-3.47217189224653));
#42563=CARTESIAN_POINT('Ctrl Pts',(-1.53851507915502,-1.,-3.46531752207153));
#42564=CARTESIAN_POINT('Ctrl Pts',(-1.53440195378792,-1.,-3.45825932955032));
#42565=CARTESIAN_POINT('Ctrl Pts',(-1.53046244461635,-1.,-3.45127136828305));
#42566=CARTESIAN_POINT('Ctrl Pts',(-1.52686242875556,-1.,-3.44469547526647));
#42567=CARTESIAN_POINT('Ctrl Pts',(-1.5237734895035,-1.,-3.4388889597401));
#42568=CARTESIAN_POINT('Ctrl Pts',(-1.52134826724293,-1.,-3.43417156977893));
#42569=CARTESIAN_POINT('Ctrl Pts',(-1.5198144909338,-1.,-3.43101631893414));
#42570=CARTESIAN_POINT('Ctrl Pts',(-1.51914806898491,-1.,-3.42946838852587));
#42571=CARTESIAN_POINT('Ctrl Pts',(-1.5189513329503,-1.,-3.42884302333841));
#42572=CARTESIAN_POINT('Ctrl Pts',(-1.51893924967331,-1.,-3.42864616361875));
#42573=CARTESIAN_POINT('Ctrl Pts',(-1.5189508286633,-1.,-3.42859860294306));
#42574=CARTESIAN_POINT('',(-1.35032489087269,-1.,-3.49844575334386));
#42575=CARTESIAN_POINT('Origin',(0.,-1.,0.));
#42576=CARTESIAN_POINT('',(-1.36999806084572,-1.,-3.97027773754922));
#42577=CARTESIAN_POINT('Ctrl Pts',(-1.35032489087269,-1.,-3.49844575334386));
#42578=CARTESIAN_POINT('Ctrl Pts',(-1.35036670893102,-1.,-3.49847119623841));
#42579=CARTESIAN_POINT('Ctrl Pts',(-1.35049736560633,-1.,-3.49861894124915));
#42580=CARTESIAN_POINT('Ctrl Pts',(-1.35080045218652,-1.,-3.49920025459856));
#42581=CARTESIAN_POINT('Ctrl Pts',(-1.35142377279535,-1.,-3.5007660381658));
#42582=CARTESIAN_POINT('Ctrl Pts',(-1.3525703284343,-1.,-3.50408168106113));
#42583=CARTESIAN_POINT('Ctrl Pts',(-1.35419113576022,-1.,-3.50913227060177));
#42584=CARTESIAN_POINT('Ctrl Pts',(-1.35611275237288,-1.,-3.51542230699919));
#42585=CARTESIAN_POINT('Ctrl Pts',(-1.35821701528975,-1.,-3.52261776117121));
#42586=CARTESIAN_POINT('Ctrl Pts',(-1.36037259643827,-1.,-3.53034464961849));
#42587=CARTESIAN_POINT('Ctrl Pts',(-1.36245507339334,-1.,-3.53824396425032));
#42588=CARTESIAN_POINT('Ctrl Pts',(-1.36436666257567,-1.,-3.54602591832893));
#42589=CARTESIAN_POINT('Ctrl Pts',(-1.36606145456711,-1.,-3.55353883995793));
#42590=CARTESIAN_POINT('Ctrl Pts',(-1.36754771771174,-1.,-3.56077662028492));
#42591=CARTESIAN_POINT('Ctrl Pts',(-1.36886584973349,-1.,-3.56782080304554));
#42592=CARTESIAN_POINT('Ctrl Pts',(-1.37007229485646,-1.,-3.57479875549453));
#42593=CARTESIAN_POINT('Ctrl Pts',(-1.37122241663073,-1.,-3.58183885982745));
#42594=CARTESIAN_POINT('Ctrl Pts',(-1.37235053661,-1.,-3.5890185384643));
#42595=CARTESIAN_POINT('Ctrl Pts',(-1.37346320103184,-1.,-3.59634627869117));
#42596=CARTESIAN_POINT('Ctrl Pts',(-1.37455051379642,-1.,-3.60379020124038));
#42597=CARTESIAN_POINT('Ctrl Pts',(-1.37559314436641,-1.,-3.61129546591082));
#42598=CARTESIAN_POINT('Ctrl Pts',(-1.37657053403102,-1.,-3.61880481160408));
#42599=CARTESIAN_POINT('Ctrl Pts',(-1.37746987919868,-1.,-3.62628098665112));
#42600=CARTESIAN_POINT('Ctrl Pts',(-1.37829035457324,-1.,-3.63371727442448));
#42601=CARTESIAN_POINT('Ctrl Pts',(-1.37903818567347,-1.,-3.64112507791112));
#42602=CARTESIAN_POINT('Ctrl Pts',(-1.37972372481598,-1.,-3.64852652756444));
#42603=CARTESIAN_POINT('Ctrl Pts',(-1.38035791051215,-1.,-3.65594554404396));
#42604=CARTESIAN_POINT('Ctrl Pts',(-1.38094856333558,-1.,-3.66339848520874));
#42605=CARTESIAN_POINT('Ctrl Pts',(-1.38149812653876,-1.,-3.67088843112282));
#42606=CARTESIAN_POINT('Ctrl Pts',(-1.38200574290626,-1.,-3.6784103848243));
#42607=CARTESIAN_POINT('Ctrl Pts',(-1.38246852827185,-1.,-3.68595444983844));
#42608=CARTESIAN_POINT('Ctrl Pts',(-1.38288311171649,-1.,-3.69350967899523));
#42609=CARTESIAN_POINT('Ctrl Pts',(-1.38324717612862,-1.,-3.70106792167894));
#42610=CARTESIAN_POINT('Ctrl Pts',(-1.38356065402122,-1.,-3.70862680753343));
#42611=CARTESIAN_POINT('Ctrl Pts',(-1.38382489984585,-1.,-3.7161876605181));
#42612=CARTESIAN_POINT('Ctrl Pts',(-1.3840421342895,-1.,-3.72375409358805));
#42613=CARTESIAN_POINT('Ctrl Pts',(-1.38421479111531,-1.,-3.73133035859283));
#42614=CARTESIAN_POINT('Ctrl Pts',(-1.38434489156456,-1.,-3.73891976418099));
#42615=CARTESIAN_POINT('Ctrl Pts',(-1.38443344984389,-1.,-3.7465231716786));
#42616=CARTESIAN_POINT('Ctrl Pts',(-1.38448077997155,-1.,-3.75413976318727));
#42617=CARTESIAN_POINT('Ctrl Pts',(-1.38448675253343,-1.,-3.76176768271347));
#42618=CARTESIAN_POINT('Ctrl Pts',(-1.38445107339517,-1.,-3.76940473185775));
#42619=CARTESIAN_POINT('Ctrl Pts',(-1.38437354551435,-1.,-3.77704902230441));
#42620=CARTESIAN_POINT('Ctrl Pts',(-1.38425435883773,-1.,-3.78469969805134));
#42621=CARTESIAN_POINT('Ctrl Pts',(-1.38409399694589,-1.,-3.79235669640907));
#42622=CARTESIAN_POINT('Ctrl Pts',(-1.38389311766701,-1.,-3.80002044322169));
#42623=CARTESIAN_POINT('Ctrl Pts',(-1.38365244046226,-1.,-3.80769156398429));
#42624=CARTESIAN_POINT('Ctrl Pts',(-1.38337263902766,-1.,-3.81537060817765));
#42625=CARTESIAN_POINT('Ctrl Pts',(-1.38305421262724,-1.,-3.82305771743715));
#42626=CARTESIAN_POINT('Ctrl Pts',(-1.38269750245086,-1.,-3.83075266982138));
#42627=CARTESIAN_POINT('Ctrl Pts',(-1.38230274828774,-1.,-3.83845502790609));
#42628=CARTESIAN_POINT('Ctrl Pts',(-1.38187013346089,-1.,-3.84616425605705));
#42629=CARTESIAN_POINT('Ctrl Pts',(-1.38139983115075,-1.,-3.85387983979557));
#42630=CARTESIAN_POINT('Ctrl Pts',(-1.38089205993067,-1.,-3.86160143044187));
#42631=CARTESIAN_POINT('Ctrl Pts',(-1.38034709213129,-1.,-3.86932885813403));
#42632=CARTESIAN_POINT('Ctrl Pts',(-1.37976523097187,-1.,-3.87706205830865));
#42633=CARTESIAN_POINT('Ctrl Pts',(-1.37914679719446,-1.,-3.88480102249461));
#42634=CARTESIAN_POINT('Ctrl Pts',(-1.37849211287981,-1.,-3.89254574338385));
#42635=CARTESIAN_POINT('Ctrl Pts',(-1.3778014851263,-1.,-3.90029615196255));
#42636=CARTESIAN_POINT('Ctrl Pts',(-1.3770751963376,-1.,-3.90805209522729));
#42637=CARTESIAN_POINT('Ctrl Pts',(-1.37631350505516,-1.,-3.91581337461825));
#42638=CARTESIAN_POINT('Ctrl Pts',(-1.37551664448057,-1.,-3.92357976987132));
#42639=CARTESIAN_POINT('Ctrl Pts',(-1.37468482215784,-1.,-3.93135106761941));
#42640=CARTESIAN_POINT('Ctrl Pts',(-1.37381821967499,-1.,-3.93912709041791));
#42641=CARTESIAN_POINT('Ctrl Pts',(-1.37291699203423,-1.,-3.94690771786926));
#42642=CARTESIAN_POINT('Ctrl Pts',(-1.37198126433139,-1.,-3.95469287283105));
#42643=CARTESIAN_POINT('Ctrl Pts',(-1.37120515615663,-1.,-3.96092458508407));
#42644=CARTESIAN_POINT('Ctrl Pts',(-1.37060761746027,-1.,-3.96560037975788));
#42645=CARTESIAN_POINT('Ctrl Pts',(-1.37020239094758,-1.,-3.9687184694173));
#42646=CARTESIAN_POINT('Ctrl Pts',(-1.36999806084572,-1.,-3.97027773754922));
#42647=CARTESIAN_POINT('',(-1.22531898815164,-1.,-4.01728681790024));
#42648=CARTESIAN_POINT('',(-1.36999806084572,-1.,-3.97027773754922));
#42649=CARTESIAN_POINT('',(-0.963899035118986,-1.,-3.62400312501199));
#42650=CARTESIAN_POINT('Ctrl Pts',(-1.22531898815164,-1.,-4.01728681790024));
#42651=CARTESIAN_POINT('Ctrl Pts',(-1.22423716681317,-1.,-4.01614544569895));
#42652=CARTESIAN_POINT('Ctrl Pts',(-1.22207656455845,-1.,-4.01386104433519));
#42653=CARTESIAN_POINT('Ctrl Pts',(-1.21884478244403,-1.,-4.01042947140789));
#42654=CARTESIAN_POINT('Ctrl Pts',(-1.21455398918133,-1.,-4.00584409522722));
#42655=CARTESIAN_POINT('Ctrl Pts',(-1.20922097029551,-1.,-4.00009577950721));
#42656=CARTESIAN_POINT('Ctrl Pts',(-1.20391852375139,-1.,-3.99433084799666));
#42657=CARTESIAN_POINT('Ctrl Pts',(-1.19864679609566,-1.,-3.98854928957189));
#42658=CARTESIAN_POINT('Ctrl Pts',(-1.19340598349475,-1.,-3.98275111052561));
#42659=CARTESIAN_POINT('Ctrl Pts',(-1.18819633715539,-1.,-3.97693634767754));
#42660=CARTESIAN_POINT('Ctrl Pts',(-1.18301815039831,-1.,-3.97110505165415));
#42661=CARTESIAN_POINT('Ctrl Pts',(-1.17787174135592,-1.,-3.96525726358159));
#42662=CARTESIAN_POINT('Ctrl Pts',(-1.17275743590361,-1.,-3.95939299213276));
#42663=CARTESIAN_POINT('Ctrl Pts',(-1.16767555244438,-1.,-3.95351219509876));
#42664=CARTESIAN_POINT('Ctrl Pts',(-1.16262637999157,-1.,-3.94761474780583));
#42665=CARTESIAN_POINT('Ctrl Pts',(-1.15761018340956,-1.,-3.94170046685203));
#42666=CARTESIAN_POINT('Ctrl Pts',(-1.1526272271632,-1.,-3.9357691705628));
#42667=CARTESIAN_POINT('Ctrl Pts',(-1.14767779451123,-1.,-3.92982073294257));
#42668=CARTESIAN_POINT('Ctrl Pts',(-1.14276220561593,-1.,-3.92385513133997));
#42669=CARTESIAN_POINT('Ctrl Pts',(-1.13788084225554,-1.,-3.91787251936827));
#42670=CARTESIAN_POINT('Ctrl Pts',(-1.13303414693896,-1.,-3.91187321145649));
#42671=CARTESIAN_POINT('Ctrl Pts',(-1.12822258281553,-1.,-3.90585753318737));
#42672=CARTESIAN_POINT('Ctrl Pts',(-1.12344660099043,-1.,-3.89982569750025));
#42673=CARTESIAN_POINT('Ctrl Pts',(-1.11870660794603,-1.,-3.89377768340344));
#42674=CARTESIAN_POINT('Ctrl Pts',(-1.11400292434429,-1.,-3.88771308285171));
#42675=CARTESIAN_POINT('Ctrl Pts',(-1.10933577224008,-1.,-3.88163105531724));
#42676=CARTESIAN_POINT('Ctrl Pts',(-1.10470536603287,-1.,-3.87553067187514));
#42677=CARTESIAN_POINT('Ctrl Pts',(-1.10011198761195,-1.,-3.86941120134849));
#42678=CARTESIAN_POINT('Ctrl Pts',(-1.09555606505013,-1.,-3.86327241021247));
#42679=CARTESIAN_POINT('Ctrl Pts',(-1.09103825516294,-1.,-3.85711487933931));
#42680=CARTESIAN_POINT('Ctrl Pts',(-1.08655950846384,-1.,-3.85094025222713));
#42681=CARTESIAN_POINT('Ctrl Pts',(-1.08212087917991,-1.,-3.8447504803063));
#42682=CARTESIAN_POINT('Ctrl Pts',(-1.07772335353858,-1.,-3.83854714117491));
#42683=CARTESIAN_POINT('Ctrl Pts',(-1.07336766633459,-1.,-3.83233071195144));
#42684=CARTESIAN_POINT('Ctrl Pts',(-1.06905413180359,-1.,-3.82609989967276));
#42685=CARTESIAN_POINT('Ctrl Pts',(-1.0647824403893,-1.,-3.81985083953012));
#42686=CARTESIAN_POINT('Ctrl Pts',(-1.06055206187299,-1.,-3.8135786611749));
#42687=CARTESIAN_POINT('Ctrl Pts',(-1.05636266918644,-1.,-3.80727913637791));
#42688=CARTESIAN_POINT('Ctrl Pts',(-1.05221457990016,-1.,-3.80095039790681));
#42689=CARTESIAN_POINT('Ctrl Pts',(-1.04810913267639,-1.,-3.79459440308786));
#42690=CARTESIAN_POINT('Ctrl Pts',(-1.04404924374422,-1.,-3.78821910787179));
#42691=CARTESIAN_POINT('Ctrl Pts',(-1.04003862055798,-1.,-3.7818353500817));
#42692=CARTESIAN_POINT('Ctrl Pts',(-1.03608074678008,-1.,-3.77545283140427));
#42693=CARTESIAN_POINT('Ctrl Pts',(-1.03217786604919,-1.,-3.76907609832516));
#42694=CARTESIAN_POINT('Ctrl Pts',(-1.02833014458184,-1.,-3.76270122291245));
#42695=CARTESIAN_POINT('Ctrl Pts',(-1.02453429444668,-1.,-3.75631037456224));
#42696=CARTESIAN_POINT('Ctrl Pts',(-1.02078510487439,-1.,-3.74987777155873));
#42697=CARTESIAN_POINT('Ctrl Pts',(-1.01707794311088,-1.,-3.74337942504993));
#42698=CARTESIAN_POINT('Ctrl Pts',(-1.01341114319906,-1.,-3.73680245055747));
#42699=CARTESIAN_POINT('Ctrl Pts',(-1.00978798539491,-1.,-3.73015276704407));
#42700=CARTESIAN_POINT('Ctrl Pts',(-1.00622000735696,-1.,-3.72346803750544));
#42701=CARTESIAN_POINT('Ctrl Pts',(-1.00272423396802,-1.,-3.71680667125047));
#42702=CARTESIAN_POINT('Ctrl Pts',(-0.999317260756344,-1.,-3.7102243971387));
#42703=CARTESIAN_POINT('Ctrl Pts',(-0.996009819772432,-1.,-3.70375282282107));
#42704=CARTESIAN_POINT('Ctrl Pts',(-0.992802218332104,-1.,-3.69738123415696));
#42705=CARTESIAN_POINT('Ctrl Pts',(-0.989676715398858,-1.,-3.69102682138955));
#42706=CARTESIAN_POINT('Ctrl Pts',(-0.986602639864286,-1.,-3.6845531792623));
#42707=CARTESIAN_POINT('Ctrl Pts',(-0.983550791470864,-1.,-3.67782408841876));
#42708=CARTESIAN_POINT('Ctrl Pts',(-0.980505922458494,-1.,-3.67074983340444));
#42709=CARTESIAN_POINT('Ctrl Pts',(-0.977478312751416,-1.,-3.66333049637403));
#42710=CARTESIAN_POINT('Ctrl Pts',(-0.974519971354139,-1.,-3.6557157673487));
#42711=CARTESIAN_POINT('Ctrl Pts',(-0.971722122060277,-1.,-3.64819756447072));
#42712=CARTESIAN_POINT('Ctrl Pts',(-0.969195124674829,-1.,-3.64113946505393));
#42713=CARTESIAN_POINT('Ctrl Pts',(-0.967052554540877,-1.,-3.6349212208096));
#42714=CARTESIAN_POINT('Ctrl Pts',(-0.965395153165716,-1.,-3.62988252139998));
#42715=CARTESIAN_POINT('Ctrl Pts',(-0.964373850166081,-1.,-3.62652618145252));
#42716=CARTESIAN_POINT('Ctrl Pts',(-0.963957782642589,-1.,-3.62489305727516));
#42717=CARTESIAN_POINT('Ctrl Pts',(-0.963861297423579,-1.,-3.62424461507455));
#42718=CARTESIAN_POINT('Ctrl Pts',(-0.963880158556713,-1.,-3.62404828878374));
#42719=CARTESIAN_POINT('Ctrl Pts',(-0.963899035118986,-1.,-3.62400312501199));
#42720=CARTESIAN_POINT('',(-0.786422660833743,-1.,-3.66661143271648));
#42721=CARTESIAN_POINT('Origin',(0.,-1.,0.));
#42722=CARTESIAN_POINT('',(-0.732042837400619,-1.,-4.13571194405636));
#42723=CARTESIAN_POINT('Ctrl Pts',(-0.786422660833743,-1.,-3.66661143271648));
#42724=CARTESIAN_POINT('Ctrl Pts',(-0.786459983896781,-1.,-3.66664310415236));
#42725=CARTESIAN_POINT('Ctrl Pts',(-0.78656591955989,-1.,-3.66680946938396));
#42726=CARTESIAN_POINT('Ctrl Pts',(-0.786774337198499,-1.,-3.66743103898844));
#42727=CARTESIAN_POINT('Ctrl Pts',(-0.787145041181589,-1.,-3.66907505398769));
#42728=CARTESIAN_POINT('Ctrl Pts',(-0.787758799995426,-1.,-3.672529236635));
#42729=CARTESIAN_POINT('Ctrl Pts',(-0.788569566220662,-1.,-3.67777119516438));
#42730=CARTESIAN_POINT('Ctrl Pts',(-0.789483546065158,-1.,-3.68428439784285));
#42731=CARTESIAN_POINT('Ctrl Pts',(-0.79043628498958,-1.,-3.69172044327754));
#42732=CARTESIAN_POINT('Ctrl Pts',(-0.791356575696509,-1.,-3.69968940808982));
#42733=CARTESIAN_POINT('Ctrl Pts',(-0.792177688845968,-1.,-3.70781724021879));
#42734=CARTESIAN_POINT('Ctrl Pts',(-0.792848377370115,-1.,-3.7158024239604));
#42735=CARTESIAN_POINT('Ctrl Pts',(-0.79334702378387,-1.,-3.7234879729357));
#42736=CARTESIAN_POINT('Ctrl Pts',(-0.793682750269347,-1.,-3.7308691469564));
#42737=CARTESIAN_POINT('Ctrl Pts',(-0.79388270093679,-1.,-3.73803280541576));
#42738=CARTESIAN_POINT('Ctrl Pts',(-0.79398270045988,-1.,-3.74511357728827));
#42739=CARTESIAN_POINT('Ctrl Pts',(-0.794017347371441,-1.,-3.75224692493895));
#42740=CARTESIAN_POINT('Ctrl Pts',(-0.794008429135047,-1.,-3.75951468666325));
#42741=CARTESIAN_POINT('Ctrl Pts',(-0.793961083689141,-1.,-3.76692626931184));
#42742=CARTESIAN_POINT('Ctrl Pts',(-0.793870523787515,-1.,-3.77444863801264));
#42743=CARTESIAN_POINT('Ctrl Pts',(-0.793726235781339,-1.,-3.78202460377617));
#42744=CARTESIAN_POINT('Ctrl Pts',(-0.793516871680966,-1.,-3.78959439439222));
#42745=CARTESIAN_POINT('Ctrl Pts',(-0.7932356129732,-1.,-3.79711921389862));
#42746=CARTESIAN_POINT('Ctrl Pts',(-0.792882695234693,-1.,-3.80459229925598));
#42747=CARTESIAN_POINT('Ctrl Pts',(-0.792462483517568,-1.,-3.81202588694726));
#42748=CARTESIAN_POINT('Ctrl Pts',(-0.791981740718606,-1.,-3.81944345442237));
#42749=CARTESIAN_POINT('Ctrl Pts',(-0.791447528662381,-1.,-3.82687033899799));
#42750=CARTESIAN_POINT('Ctrl Pts',(-0.79086501270534,-1.,-3.83432392054804));
#42751=CARTESIAN_POINT('Ctrl Pts',(-0.790236124191289,-1.,-3.84180762342476));
#42752=CARTESIAN_POINT('Ctrl Pts',(-0.789560798155619,-1.,-3.8493163780891));
#42753=CARTESIAN_POINT('Ctrl Pts',(-0.788837734090688,-1.,-3.85683995872536));
#42754=CARTESIAN_POINT('Ctrl Pts',(-0.788065315093771,-1.,-3.86436702561342));
#42755=CARTESIAN_POINT('Ctrl Pts',(-0.78724252761798,-1.,-3.87188916600905));
#42756=CARTESIAN_POINT('Ctrl Pts',(-0.786369675812592,-1.,-3.87940402818186));
#42757=CARTESIAN_POINT('Ctrl Pts',(-0.785447890340723,-1.,-3.88691313167399));
#42758=CARTESIAN_POINT('Ctrl Pts',(-0.784478799358336,-1.,-3.89442039235105));
#42759=CARTESIAN_POINT('Ctrl Pts',(-0.783464141529082,-1.,-3.90193039043971));
#42760=CARTESIAN_POINT('Ctrl Pts',(-0.782405395622759,-1.,-3.90944671004536));
#42761=CARTESIAN_POINT('Ctrl Pts',(-0.781303428618344,-1.,-3.9169703605466));
#42762=CARTESIAN_POINT('Ctrl Pts',(-0.780158678615507,-1.,-3.92450058323799));
#42763=CARTESIAN_POINT('Ctrl Pts',(-0.778971308134786,-1.,-3.93203552473153));
#42764=CARTESIAN_POINT('Ctrl Pts',(-0.77774137056855,-1.,-3.93957296768098));
#42765=CARTESIAN_POINT('Ctrl Pts',(-0.77646896669796,-1.,-3.94711101619471));
#42766=CARTESIAN_POINT('Ctrl Pts',(-0.775154418039441,-1.,-3.95464885452364));
#42767=CARTESIAN_POINT('Ctrl Pts',(-0.773798212026683,-1.,-3.96218649639876));
#42768=CARTESIAN_POINT('Ctrl Pts',(-0.772400931772239,-1.,-3.96972446532832));
#42769=CARTESIAN_POINT('Ctrl Pts',(-0.770963190030504,-1.,-3.97726349165507));
#42770=CARTESIAN_POINT('Ctrl Pts',(-0.769485566245459,-1.,-3.98480422348403));
#42771=CARTESIAN_POINT('Ctrl Pts',(-0.767968531377708,-1.,-3.99234687880892));
#42772=CARTESIAN_POINT('Ctrl Pts',(-0.766412457135786,-1.,-3.99989129179464));
#42773=CARTESIAN_POINT('Ctrl Pts',(-0.764817648784946,-1.,-4.00743706791366));
#42774=CARTESIAN_POINT('Ctrl Pts',(-0.763184371182827,-1.,-4.01498370680434));
#42775=CARTESIAN_POINT('Ctrl Pts',(-0.761512875859942,-1.,-4.02253072741347));
#42776=CARTESIAN_POINT('Ctrl Pts',(-0.759803433244166,-1.,-4.0300778195465));
#42777=CARTESIAN_POINT('Ctrl Pts',(-0.758056338885554,-1.,-4.03762485803468));
#42778=CARTESIAN_POINT('Ctrl Pts',(-0.756271902370187,-1.,-4.04517182654344));
#42779=CARTESIAN_POINT('Ctrl Pts',(-0.754450441816412,-1.,-4.05271876688106));
#42780=CARTESIAN_POINT('Ctrl Pts',(-0.752592276482869,-1.,-4.06026572221399));
#42781=CARTESIAN_POINT('Ctrl Pts',(-0.750697720483176,-1.,-4.06781267241886));
#42782=CARTESIAN_POINT('Ctrl Pts',(-0.748767076679177,-1.,-4.07535951055363));
#42783=CARTESIAN_POINT('Ctrl Pts',(-0.746800631490822,-1.,-4.08290608094789));
#42784=CARTESIAN_POINT('Ctrl Pts',(-0.744798649705514,-1.,-4.09045220253011));
#42785=CARTESIAN_POINT('Ctrl Pts',(-0.742761369690018,-1.,-4.09799769702712));
#42786=CARTESIAN_POINT('Ctrl Pts',(-0.740688998555152,-1.,-4.1055424175856));
#42787=CARTESIAN_POINT('Ctrl Pts',(-0.738581708229119,-1.,-4.11308626953795));
#42788=CARTESIAN_POINT('Ctrl Pts',(-0.736439634335347,-1.,-4.12062919626082));
#42789=CARTESIAN_POINT('Ctrl Pts',(-0.734698226767512,-1.,-4.12666277572794));
#42790=CARTESIAN_POINT('Ctrl Pts',(-0.733376589325634,-1.,-4.13118752796397));
#42791=CARTESIAN_POINT('Ctrl Pts',(-0.732488575135926,-1.,-4.13420383737278));
#42792=CARTESIAN_POINT('Ctrl Pts',(-0.732042837400619,-1.,-4.13571194405636));
#42793=CARTESIAN_POINT('',(-0.581791163835814,-1.,-4.15950947128175));
#42794=CARTESIAN_POINT('',(-0.732042837400619,-1.,-4.13571194405636));
#42795=CARTESIAN_POINT('',(-0.385112848332549,-1.,-3.73017266276632));
#42796=CARTESIAN_POINT('Ctrl Pts',(-0.581791163835814,-1.,-4.15950947128175));
#42797=CARTESIAN_POINT('Ctrl Pts',(-0.580901211462913,-1.,-4.15821291712391));
#42798=CARTESIAN_POINT('Ctrl Pts',(-0.579124568912543,-1.,-4.15561864787379));
#42799=CARTESIAN_POINT('Ctrl Pts',(-0.576469391673917,-1.,-4.1517237611974));
#42800=CARTESIAN_POINT('Ctrl Pts',(-0.572948736066277,-1.,-4.14652361065787));
#42801=CARTESIAN_POINT('Ctrl Pts',(-0.568580610187116,-1.,-4.14001179828669));
#42802=CARTESIAN_POINT('Ctrl Pts',(-0.564245279535705,-1.,-4.13348835726086));
#42803=CARTESIAN_POINT('Ctrl Pts',(-0.559942890594628,-1.,-4.12695329951859));
#42804=CARTESIAN_POINT('Ctrl Pts',(-0.555673636130778,-1.,-4.1204066619623));
#42805=CARTESIAN_POINT('Ctrl Pts',(-0.551437758498247,-1.,-4.11384852025578));
#42806=CARTESIAN_POINT('Ctrl Pts',(-0.54723553948676,-1.,-4.1072789702877));
#42807=CARTESIAN_POINT('Ctrl Pts',(-0.543067286878457,-1.,-4.10069810244473));
#42808=CARTESIAN_POINT('Ctrl Pts',(-0.538933321179921,-1.,-4.09410597627116));
#42809=CARTESIAN_POINT('Ctrl Pts',(-0.534833963476999,-1.,-4.08750259988693));
#42810=CARTESIAN_POINT('Ctrl Pts',(-0.530769518728075,-1.,-4.08088789536488));
#42811=CARTESIAN_POINT('Ctrl Pts',(-0.526740277227,-1.,-4.07426172299496));
#42812=CARTESIAN_POINT('Ctrl Pts',(-0.522746528602768,-1.,-4.06762394471075));
#42813=CARTESIAN_POINT('Ctrl Pts',(-0.51878857233681,-1.,-4.06097448037934));
#42814=CARTESIAN_POINT('Ctrl Pts',(-0.514866728193104,-1.,-4.05431335771261));
#42815=CARTESIAN_POINT('Ctrl Pts',(-0.510981349219174,-1.,-4.04764078815591));
#42816=CARTESIAN_POINT('Ctrl Pts',(-0.507132823288362,-1.,-4.04095715149074));
#42817=CARTESIAN_POINT('Ctrl Pts',(-0.503321556915514,-1.,-4.0342628417439));
#42818=CARTESIAN_POINT('Ctrl Pts',(-0.49954796234089,-1.,-4.0275581398015));
#42819=CARTESIAN_POINT('Ctrl Pts',(-0.495812444326223,-1.,-4.02084308851813));
#42820=CARTESIAN_POINT('Ctrl Pts',(-0.492115383417931,-1.,-4.01411733503486));
#42821=CARTESIAN_POINT('Ctrl Pts',(-0.488457130424531,-1.,-4.0073800839092));
#42822=CARTESIAN_POINT('Ctrl Pts',(-0.484838042421754,-1.,-4.00063045119234));
#42823=CARTESIAN_POINT('Ctrl Pts',(-0.481258512209638,-1.,-3.99386775880655));
#42824=CARTESIAN_POINT('Ctrl Pts',(-0.477718999122033,-1.,-3.98709184306743));
#42825=CARTESIAN_POINT('Ctrl Pts',(-0.474220061019542,-1.,-3.9803033804443));
#42826=CARTESIAN_POINT('Ctrl Pts',(-0.470762379613477,-1.,-3.97350414289415));
#42827=CARTESIAN_POINT('Ctrl Pts',(-0.467346690880672,-1.,-3.96669622273946));
#42828=CARTESIAN_POINT('Ctrl Pts',(-0.463973722115744,-1.,-3.95988133243543));
#42829=CARTESIAN_POINT('Ctrl Pts',(-0.460644124429119,-1.,-3.95306005817363));
#42830=CARTESIAN_POINT('Ctrl Pts',(-0.457358410451674,-1.,-3.94623117206675));
#42831=CARTESIAN_POINT('Ctrl Pts',(-0.454116879027576,-1.,-3.93939080846298));
#42832=CARTESIAN_POINT('Ctrl Pts',(-0.450919768356347,-1.,-3.93253407403128));
#42833=CARTESIAN_POINT('Ctrl Pts',(-0.447767416837297,-1.,-3.92565674143424));
#42834=CARTESIAN_POINT('Ctrl Pts',(-0.444660430230593,-1.,-3.91875701610721));
#42835=CARTESIAN_POINT('Ctrl Pts',(-0.441599824524047,-1.,-3.91183704069146));
#42836=CARTESIAN_POINT('Ctrl Pts',(-0.438587235458233,-1.,-3.90490512938546));
#42837=CARTESIAN_POINT('Ctrl Pts',(-0.435624629433506,-1.,-3.8979725665544));
#42838=CARTESIAN_POINT('Ctrl Pts',(-0.432713929544439,-1.,-3.89104947940592));
#42839=CARTESIAN_POINT('Ctrl Pts',(-0.429856640579734,-1.,-3.88414070943334));
#42840=CARTESIAN_POINT('Ctrl Pts',(-0.427053541173469,-1.,-3.87724240306609));
#42841=CARTESIAN_POINT('Ctrl Pts',(-0.424304173195142,-1.,-3.87033643487882));
#42842=CARTESIAN_POINT('Ctrl Pts',(-0.421607423177576,-1.,-3.86339652542749));
#42843=CARTESIAN_POINT('Ctrl Pts',(-0.41896246808681,-1.,-3.85639825648031));
#42844=CARTESIAN_POINT('Ctrl Pts',(-0.41636967805292,-1.,-3.8493286415751));
#42845=CARTESIAN_POINT('Ctrl Pts',(-0.413831367016727,-1.,-3.84219403994742));
#42846=CARTESIAN_POINT('Ctrl Pts',(-0.41135303879846,-1.,-3.83503345578645));
#42847=CARTESIAN_POINT('Ctrl Pts',(-0.408942371447377,-1.,-3.82790724256397));
#42848=CARTESIAN_POINT('Ctrl Pts',(-0.406607038258906,-1.,-3.82087303913741));
#42849=CARTESIAN_POINT('Ctrl Pts',(-0.404352694628236,-1.,-3.81396374287762));
#42850=CARTESIAN_POINT('Ctrl Pts',(-0.402181320148475,-1.,-3.80716881962763));
#42851=CARTESIAN_POINT('Ctrl Pts',(-0.400088346504727,-1.,-3.80040370384659));
#42852=CARTESIAN_POINT('Ctrl Pts',(-0.398064818684158,-1.,-3.79352887163457));
#42853=CARTESIAN_POINT('Ctrl Pts',(-0.396103205335029,-1.,-3.78640521279479));
#42854=CARTESIAN_POINT('Ctrl Pts',(-0.394202481011595,-1.,-3.77894173114368));
#42855=CARTESIAN_POINT('Ctrl Pts',(-0.392372786223347,-1.,-3.77114011595892));
#42856=CARTESIAN_POINT('Ctrl Pts',(-0.390642072979259,-1.,-3.76315635032993));
#42857=CARTESIAN_POINT('Ctrl Pts',(-0.389054775898251,-1.,-3.75529302894757));
#42858=CARTESIAN_POINT('Ctrl Pts',(-0.387663020050396,-1.,-3.74792651696269));
#42859=CARTESIAN_POINT('Ctrl Pts',(-0.386519576222035,-1.,-3.74144965781088));
#42860=CARTESIAN_POINT('Ctrl Pts',(-0.385670806454744,-1.,-3.73621371845475));
#42861=CARTESIAN_POINT('Ctrl Pts',(-0.385187124633965,-1.,-3.73273893363318));
#42862=CARTESIAN_POINT('Ctrl Pts',(-0.385031656499141,-1.,-3.73106082862399));
#42863=CARTESIAN_POINT('Ctrl Pts',(-0.385037797882046,-1.,-3.73040527620929));
#42864=CARTESIAN_POINT('Ctrl Pts',(-0.385087139001609,-1.,-3.73021431755218));
#42865=CARTESIAN_POINT('Ctrl Pts',(-0.385112848332549,-1.,-3.73017266276632));
#42866=CARTESIAN_POINT('',(-0.203156094897896,-1.,-3.74449296982994));
#42867=CARTESIAN_POINT('Origin',(0.,-1.,0.));
#42868=CARTESIAN_POINT('',(-0.0760622897878238,-1.,-4.19931119685982));
#42869=CARTESIAN_POINT('Ctrl Pts',(-0.203156094897896,-1.,-3.74449296982994));
#42870=CARTESIAN_POINT('Ctrl Pts',(-0.203188003947965,-1.,-3.74453008995129));
#42871=CARTESIAN_POINT('Ctrl Pts',(-0.203266610111264,-1.,-3.74471097893961));
#42872=CARTESIAN_POINT('Ctrl Pts',(-0.203375226874331,-1.,-3.74535749969262));
#42873=CARTESIAN_POINT('Ctrl Pts',(-0.203484186269315,-1.,-3.74703926501843));
#42874=CARTESIAN_POINT('Ctrl Pts',(-0.203550035479097,-1.,-3.75054693397716));
#42875=CARTESIAN_POINT('Ctrl Pts',(-0.203530796848404,-1.,-3.75585118707924));
#42876=CARTESIAN_POINT('Ctrl Pts',(-0.203414634707646,-1.,-3.76242717937273));
#42877=CARTESIAN_POINT('Ctrl Pts',(-0.203192390045337,-1.,-3.76992071595267));
#42878=CARTESIAN_POINT('Ctrl Pts',(-0.202854729699197,-1.,-3.77793553476879));
#42879=CARTESIAN_POINT('Ctrl Pts',(-0.202394260512193,-1.,-3.78609175019317));
#42880=CARTESIAN_POINT('Ctrl Pts',(-0.201807533800799,-1.,-3.79408354187274));
#42881=CARTESIAN_POINT('Ctrl Pts',(-0.201097756307252,-1.,-3.80175247447171));
#42882=CARTESIAN_POINT('Ctrl Pts',(-0.20027467943329,-1.,-3.80909529318501));
#42883=CARTESIAN_POINT('Ctrl Pts',(-0.199351525297396,-1.,-3.81620203429702));
#42884=CARTESIAN_POINT('Ctrl Pts',(-0.19834261690047,-1.,-3.82321127348981));
#42885=CARTESIAN_POINT('Ctrl Pts',(-0.197260935827375,-1.,-3.83026221776488));
#42886=CARTESIAN_POINT('Ctrl Pts',(-0.19611519897189,-1.,-3.83743910616265));
#42887=CARTESIAN_POINT('Ctrl Pts',(-0.194909009460255,-1.,-3.84475203347052));
#42888=CARTESIAN_POINT('Ctrl Pts',(-0.193642806777748,-1.,-3.85216762264019));
#42889=CARTESIAN_POINT('Ctrl Pts',(-0.19231515304498,-1.,-3.85962774407652));
#42890=CARTESIAN_POINT('Ctrl Pts',(-0.190924190418613,-1.,-3.8670715862477));
#42891=CARTESIAN_POINT('Ctrl Pts',(-0.189469253358254,-1.,-3.87445976418377));
#42892=CARTESIAN_POINT('Ctrl Pts',(-0.187951632512663,-1.,-3.88178563496187));
#42893=CARTESIAN_POINT('Ctrl Pts',(-0.186373724985263,-1.,-3.88906196725817));
#42894=CARTESIAN_POINT('Ctrl Pts',(-0.184738537728035,-1.,-3.89631300742633));
#42895=CARTESIAN_POINT('Ctrl Pts',(-0.183049081993193,-1.,-3.90356488555138));
#42896=CARTESIAN_POINT('Ctrl Pts',(-0.181307740731796,-1.,-3.91083557557193));
#42897=CARTESIAN_POINT('Ctrl Pts',(-0.179515885822895,-1.,-3.91812876180948));
#42898=CARTESIAN_POINT('Ctrl Pts',(-0.177674246152328,-1.,-3.92543942697672));
#42899=CARTESIAN_POINT('Ctrl Pts',(-0.175783136893873,-1.,-3.93275726771049));
#42900=CARTESIAN_POINT('Ctrl Pts',(-0.173842734974607,-1.,-3.94007083096214));
#42901=CARTESIAN_POINT('Ctrl Pts',(-0.171853355369233,-1.,-3.94737164900861));
#42902=CARTESIAN_POINT('Ctrl Pts',(-0.16981566637413,-1.,-3.95465744665263));
#42903=CARTESIAN_POINT('Ctrl Pts',(-0.167730547023312,-1.,-3.96192990160296));
#42904=CARTESIAN_POINT('Ctrl Pts',(-0.165598992851098,-1.,-3.9691931362141));
#42905=CARTESIAN_POINT('Ctrl Pts',(-0.163422004609999,-1.,-3.97645194630944));
#42906=CARTESIAN_POINT('Ctrl Pts',(-0.161200482186088,-1.,-3.98371010319866));
#42907=CARTESIAN_POINT('Ctrl Pts',(-0.158935123982796,-1.,-3.99096873945862));
#42908=CARTESIAN_POINT('Ctrl Pts',(-0.156626481393736,-1.,-3.99822717425869));
#42909=CARTESIAN_POINT('Ctrl Pts',(-0.15427500487231,-1.,-4.00548360245297));
#42910=CARTESIAN_POINT('Ctrl Pts',(-0.151881094022909,-1.,-4.01273584234684));
#42911=CARTESIAN_POINT('Ctrl Pts',(-0.149445144968708,-1.,-4.01998203715588));
#42912=CARTESIAN_POINT('Ctrl Pts',(-0.146967602878999,-1.,-4.02722143147048));
#42913=CARTESIAN_POINT('Ctrl Pts',(-0.144448947038352,-1.,-4.03445411510403));
#42914=CARTESIAN_POINT('Ctrl Pts',(-0.141889671485508,-1.,-4.04168069633842));
#42915=CARTESIAN_POINT('Ctrl Pts',(-0.13929026718006,-1.,-4.04890199238056));
#42916=CARTESIAN_POINT('Ctrl Pts',(-0.136651205046111,-1.,-4.05611873400122));
#42917=CARTESIAN_POINT('Ctrl Pts',(-0.133972916144225,-1.,-4.06333121018476));
#42918=CARTESIAN_POINT('Ctrl Pts',(-0.131255793548914,-1.,-4.07053931528579));
#42919=CARTESIAN_POINT('Ctrl Pts',(-0.128500200484814,-1.,-4.07774270738809));
#42920=CARTESIAN_POINT('Ctrl Pts',(-0.125706476822529,-1.,-4.08494093372315));
#42921=CARTESIAN_POINT('Ctrl Pts',(-0.122874946249119,-1.,-4.09213355850836));
#42922=CARTESIAN_POINT('Ctrl Pts',(-0.120005924388162,-1.,-4.09932031767243));
#42923=CARTESIAN_POINT('Ctrl Pts',(-0.117099722731705,-1.,-4.10650113382187));
#42924=CARTESIAN_POINT('Ctrl Pts',(-0.114156649609602,-1.,-4.11367603925313));
#42925=CARTESIAN_POINT('Ctrl Pts',(-0.111177012683377,-1.,-4.12084512502444));
#42926=CARTESIAN_POINT('Ctrl Pts',(-0.10816112052835,-1.,-4.12800848371386));
#42927=CARTESIAN_POINT('Ctrl Pts',(-0.105109286538864,-1.,-4.13516614458396));
#42928=CARTESIAN_POINT('Ctrl Pts',(-0.102021826577454,-1.,-4.14231804938737));
#42929=CARTESIAN_POINT('Ctrl Pts',(-0.0988990478899814,-1.,-4.1494640891762));
#42930=CARTESIAN_POINT('Ctrl Pts',(-0.095741240329707,-1.,-4.15660412653006));
#42931=CARTESIAN_POINT('Ctrl Pts',(-0.0925486672167692,-1.,-4.16373802265942));
#42932=CARTESIAN_POINT('Ctrl Pts',(-0.089321556085033,-1.,-4.17086566491823));
#42933=CARTESIAN_POINT('Ctrl Pts',(-0.0860600915552517,-1.,-4.17798698669991));
#42934=CARTESIAN_POINT('Ctrl Pts',(-0.0827644164389512,-1.,-4.1851019532944));
#42935=CARTESIAN_POINT('Ctrl Pts',(-0.0801005887117605,-1.,-4.19078883322483));
#42936=CARTESIAN_POINT('Ctrl Pts',(-0.0780873956244405,-1.,-4.19505112860624));
#42937=CARTESIAN_POINT('Ctrl Pts',(-0.0767384596142197,-1.,-4.19789138621624));
#42938=CARTESIAN_POINT('Ctrl Pts',(-0.0760622897878238,-1.,-4.19931119685982));
#42939=CARTESIAN_POINT('',(0.0760622897878244,-1.,-4.19931119685982));
#42940=CARTESIAN_POINT('',(-0.0760622897878238,-1.,-4.19931119685982));
#42941=CARTESIAN_POINT('',(0.2031560948961,-1.,-3.74449296983004));
#42942=CARTESIAN_POINT('Ctrl Pts',(0.0760622897878244,-1.,-4.19931119685982));
#42943=CARTESIAN_POINT('Ctrl Pts',(0.0767384596141462,-1.,-4.1978913862118));
#42944=CARTESIAN_POINT('Ctrl Pts',(0.0780873956242395,-1.,-4.19505112859416));
#42945=CARTESIAN_POINT('Ctrl Pts',(0.0801005887114317,-1.,-4.19078883320504));
#42946=CARTESIAN_POINT('Ctrl Pts',(0.0827644164385676,-1.,-4.18510195327123));
#42947=CARTESIAN_POINT('Ctrl Pts',(0.0860600915549394,-1.,-4.17798698668094));
#42948=CARTESIAN_POINT('Ctrl Pts',(0.0893215560848647,-1.,-4.17086566490794));
#42949=CARTESIAN_POINT('Ctrl Pts',(0.0925486672167528,-1.,-4.16373802265839));
#42950=CARTESIAN_POINT('Ctrl Pts',(0.0957412403298004,-1.,-4.15660412653577));
#42951=CARTESIAN_POINT('Ctrl Pts',(0.0988990478901223,-1.,-4.14946408918485));
#42952=CARTESIAN_POINT('Ctrl Pts',(0.102021826577584,-1.,-4.14231804939538));
#42953=CARTESIAN_POINT('Ctrl Pts',(0.105109286538945,-1.,-4.13516614458895));
#42954=CARTESIAN_POINT('Ctrl Pts',(0.108161120528369,-1.,-4.12800848371504));
#42955=CARTESIAN_POINT('Ctrl Pts',(0.111177012683346,-1.,-4.1208451250225));
#42956=CARTESIAN_POINT('Ctrl Pts',(0.114156649609545,-1.,-4.11367603924961));
#42957=CARTESIAN_POINT('Ctrl Pts',(0.117099722731648,-1.,-4.10650113381833));
#42958=CARTESIAN_POINT('Ctrl Pts',(0.120005924388124,-1.,-4.09932031767002));
#42959=CARTESIAN_POINT('Ctrl Pts',(0.122874946249107,-1.,-4.09213355850756));
#42960=CARTESIAN_POINT('Ctrl Pts',(0.12570647682254,-1.,-4.08494093372377));
#42961=CARTESIAN_POINT('Ctrl Pts',(0.128500200484837,-1.,-4.07774270738954));
#42962=CARTESIAN_POINT('Ctrl Pts',(0.13125579354894,-1.,-4.0705393152874));
#42963=CARTESIAN_POINT('Ctrl Pts',(0.133972916144245,-1.,-4.06333121018596));
#42964=CARTESIAN_POINT('Ctrl Pts',(0.136651205046119,-1.,-4.05611873400172));
#42965=CARTESIAN_POINT('Ctrl Pts',(0.139290267180057,-1.,-4.04890199238036));
#42966=CARTESIAN_POINT('Ctrl Pts',(0.1418896714855,-1.,-4.04168069633781));
#42967=CARTESIAN_POINT('Ctrl Pts',(0.144448947038344,-1.,-4.03445411510333));
#42968=CARTESIAN_POINT('Ctrl Pts',(0.146967602878994,-1.,-4.02722143146994));
#42969=CARTESIAN_POINT('Ctrl Pts',(0.149445144968707,-1.,-4.01998203715564));
#42970=CARTESIAN_POINT('Ctrl Pts',(0.15188109402291,-1.,-4.01273584234689));
#42971=CARTESIAN_POINT('Ctrl Pts',(0.15427500487231,-1.,-4.00548360245319));
#42972=CARTESIAN_POINT('Ctrl Pts',(0.156626481393734,-1.,-3.99822717425893));
#42973=CARTESIAN_POINT('Ctrl Pts',(0.158935123982793,-1.,-3.99096873945878));
#42974=CARTESIAN_POINT('Ctrl Pts',(0.161200482186084,-1.,-3.98371010319872));
#42975=CARTESIAN_POINT('Ctrl Pts',(0.163422004609999,-1.,-3.97645194630943));
#42976=CARTESIAN_POINT('Ctrl Pts',(0.165598992851102,-1.,-3.96919313621407));
#42977=CARTESIAN_POINT('Ctrl Pts',(0.167730547023319,-1.,-3.96192990160296));
#42978=CARTESIAN_POINT('Ctrl Pts',(0.169815666374139,-1.,-3.95465744665268));
#42979=CARTESIAN_POINT('Ctrl Pts',(0.17185335536924,-1.,-3.94737164900868));
#42980=CARTESIAN_POINT('Ctrl Pts',(0.173842734974609,-1.,-3.94007083096217));
#42981=CARTESIAN_POINT('Ctrl Pts',(0.175783136893868,-1.,-3.93275726771042));
#42982=CARTESIAN_POINT('Ctrl Pts',(0.177674246152317,-1.,-3.92543942697655));
#42983=CARTESIAN_POINT('Ctrl Pts',(0.179515885822881,-1.,-3.91812876180926));
#42984=CARTESIAN_POINT('Ctrl Pts',(0.181307740731785,-1.,-3.91083557557175));
#42985=CARTESIAN_POINT('Ctrl Pts',(0.18304908199319,-1.,-3.90356488555132));
#42986=CARTESIAN_POINT('Ctrl Pts',(0.184738537728043,-1.,-3.89631300742646));
#42987=CARTESIAN_POINT('Ctrl Pts',(0.18637372498528,-1.,-3.88906196725848));
#42988=CARTESIAN_POINT('Ctrl Pts',(0.187951632512685,-1.,-3.88178563496228));
#42989=CARTESIAN_POINT('Ctrl Pts',(0.189469253358272,-1.,-3.87445976418412));
#42990=CARTESIAN_POINT('Ctrl Pts',(0.19092419041862,-1.,-3.86707158624783));
#42991=CARTESIAN_POINT('Ctrl Pts',(0.19231515304497,-1.,-3.85962774407633));
#42992=CARTESIAN_POINT('Ctrl Pts',(0.193642806777723,-1.,-3.85216762263966));
#42993=CARTESIAN_POINT('Ctrl Pts',(0.19490900946022,-1.,-3.84475203346977));
#42994=CARTESIAN_POINT('Ctrl Pts',(0.196115198971859,-1.,-3.83743910616195));
#42995=CARTESIAN_POINT('Ctrl Pts',(0.197260935827361,-1.,-3.83026221776456));
#42996=CARTESIAN_POINT('Ctrl Pts',(0.198342616900486,-1.,-3.82321127349016));
#42997=CARTESIAN_POINT('Ctrl Pts',(0.199351525297447,-1.,-3.81620203429815));
#42998=CARTESIAN_POINT('Ctrl Pts',(0.200274679433364,-1.,-3.80909529318669));
#42999=CARTESIAN_POINT('Ctrl Pts',(0.201097756307326,-1.,-3.80175247447337));
#43000=CARTESIAN_POINT('Ctrl Pts',(0.201807533800837,-1.,-3.7940835418736));
#43001=CARTESIAN_POINT('Ctrl Pts',(0.20239426051216,-1.,-3.78609175019242));
#43002=CARTESIAN_POINT('Ctrl Pts',(0.202854729699081,-1.,-3.77793553476614));
#43003=CARTESIAN_POINT('Ctrl Pts',(0.203192390045164,-1.,-3.7699207159487));
#43004=CARTESIAN_POINT('Ctrl Pts',(0.203414634707478,-1.,-3.76242717936885));
#43005=CARTESIAN_POINT('Ctrl Pts',(0.203530796848321,-1.,-3.75585118707734));
#43006=CARTESIAN_POINT('Ctrl Pts',(0.203550035479166,-1.,-3.75054693397875));
#43007=CARTESIAN_POINT('Ctrl Pts',(0.203484186269415,-1.,-3.74703926501752));
#43008=CARTESIAN_POINT('Ctrl Pts',(0.203375226874121,-1.,-3.74535749969115));
#43009=CARTESIAN_POINT('Ctrl Pts',(0.203266610110531,-1.,-3.74471097893845));
#43010=CARTESIAN_POINT('Ctrl Pts',(0.203188003946657,-1.,-3.74453008995092));
#43011=CARTESIAN_POINT('Ctrl Pts',(0.2031560948961,-1.,-3.74449296983004));
#43012=CARTESIAN_POINT('',(0.385112848330761,-1.,-3.73017266276651));
#43013=CARTESIAN_POINT('Origin',(0.,-1.,0.));
#43014=CARTESIAN_POINT('',(0.581791163835815,-1.,-4.15950947128175));
#43015=CARTESIAN_POINT('Ctrl Pts',(0.385112848330761,-1.,-3.73017266276651));
#43016=CARTESIAN_POINT('Ctrl Pts',(0.385087139000374,-1.,-3.73021431755274));
#43017=CARTESIAN_POINT('Ctrl Pts',(0.385037797881504,-1.,-3.73040527621055));
#43018=CARTESIAN_POINT('Ctrl Pts',(0.385031656499164,-1.,-3.73106082862548));
#43019=CARTESIAN_POINT('Ctrl Pts',(0.385187124634206,-1.,-3.73273893363406));
#43020=CARTESIAN_POINT('Ctrl Pts',(0.385670806454565,-1.,-3.73621371845318));
#43021=CARTESIAN_POINT('Ctrl Pts',(0.386519576222251,-1.,-3.74144965781276));
#43022=CARTESIAN_POINT('Ctrl Pts',(0.387663020050836,-1.,-3.74792651696654));
#43023=CARTESIAN_POINT('Ctrl Pts',(0.389054775898701,-1.,-3.75529302895152));
#43024=CARTESIAN_POINT('Ctrl Pts',(0.390642072979559,-1.,-3.76315635033257));
#43025=CARTESIAN_POINT('Ctrl Pts',(0.392372786223432,-1.,-3.77114011595967));
#43026=CARTESIAN_POINT('Ctrl Pts',(0.394202481011499,-1.,-3.77894173114283));
#43027=CARTESIAN_POINT('Ctrl Pts',(0.39610320533484,-1.,-3.78640521279313));
#43028=CARTESIAN_POINT('Ctrl Pts',(0.398064818683969,-1.,-3.7935288716329));
#43029=CARTESIAN_POINT('Ctrl Pts',(0.4000883465046,-1.,-3.80040370384546));
#43030=CARTESIAN_POINT('Ctrl Pts',(0.402181320148435,-1.,-3.80716881962728));
#43031=CARTESIAN_POINT('Ctrl Pts',(0.404352694628273,-1.,-3.81396374287793));
#43032=CARTESIAN_POINT('Ctrl Pts',(0.406607038258985,-1.,-3.8208730391381));
#43033=CARTESIAN_POINT('Ctrl Pts',(0.408942371447459,-1.,-3.82790724256471));
#43034=CARTESIAN_POINT('Ctrl Pts',(0.411353038798518,-1.,-3.83503345578698));
#43035=CARTESIAN_POINT('Ctrl Pts',(0.413831367016748,-1.,-3.84219403994762));
#43036=CARTESIAN_POINT('Ctrl Pts',(0.416369678052906,-1.,-3.84932864157497));
#43037=CARTESIAN_POINT('Ctrl Pts',(0.418962468086773,-1.,-3.85639825647996));
#43038=CARTESIAN_POINT('Ctrl Pts',(0.421607423177534,-1.,-3.86339652542709));
#43039=CARTESIAN_POINT('Ctrl Pts',(0.42430417319511,-1.,-3.87033643487851));
#43040=CARTESIAN_POINT('Ctrl Pts',(0.427053541173457,-1.,-3.87724240306597));
#43041=CARTESIAN_POINT('Ctrl Pts',(0.429856640579741,-1.,-3.88414070943341));
#43042=CARTESIAN_POINT('Ctrl Pts',(0.432713929544458,-1.,-3.89104947940611));
#43043=CARTESIAN_POINT('Ctrl Pts',(0.435624629433527,-1.,-3.89797256655462));
#43044=CARTESIAN_POINT('Ctrl Pts',(0.438587235458249,-1.,-3.90490512938563));
#43045=CARTESIAN_POINT('Ctrl Pts',(0.441599824524054,-1.,-3.91183704069153));
#43046=CARTESIAN_POINT('Ctrl Pts',(0.44466043023059,-1.,-3.91875701610719));
#43047=CARTESIAN_POINT('Ctrl Pts',(0.447767416837292,-1.,-3.92565674143416));
#43048=CARTESIAN_POINT('Ctrl Pts',(0.450919768356348,-1.,-3.93253407403123));
#43049=CARTESIAN_POINT('Ctrl Pts',(0.454116879027584,-1.,-3.93939080846298));
#43050=CARTESIAN_POINT('Ctrl Pts',(0.457358410451682,-1.,-3.94623117206678));
#43051=CARTESIAN_POINT('Ctrl Pts',(0.460644124429121,-1.,-3.95306005817364));
#43052=CARTESIAN_POINT('Ctrl Pts',(0.463973722115733,-1.,-3.95988133243538));
#43053=CARTESIAN_POINT('Ctrl Pts',(0.467346690880643,-1.,-3.9666962227393));
#43054=CARTESIAN_POINT('Ctrl Pts',(0.470762379613439,-1.,-3.97350414289392));
#43055=CARTESIAN_POINT('Ctrl Pts',(0.474220061019509,-1.,-3.98030338044409));
#43056=CARTESIAN_POINT('Ctrl Pts',(0.477718999122027,-1.,-3.98709184306738));
#43057=CARTESIAN_POINT('Ctrl Pts',(0.481258512209675,-1.,-3.99386775880679));
#43058=CARTESIAN_POINT('Ctrl Pts',(0.484838042421834,-1.,-4.00063045119288));
#43059=CARTESIAN_POINT('Ctrl Pts',(0.488457130424633,-1.,-4.0073800839099));
#43060=CARTESIAN_POINT('Ctrl Pts',(0.492115383418018,-1.,-4.01411733503546));
#43061=CARTESIAN_POINT('Ctrl Pts',(0.495812444326251,-1.,-4.02084308851832));
#43062=CARTESIAN_POINT('Ctrl Pts',(0.499547962340821,-1.,-4.02755813980101));
#43063=CARTESIAN_POINT('Ctrl Pts',(0.503321556915346,-1.,-4.03426284174272));
#43064=CARTESIAN_POINT('Ctrl Pts',(0.507132823288136,-1.,-4.04095715148915));
#43065=CARTESIAN_POINT('Ctrl Pts',(0.51098134921897,-1.,-4.04764078815447));
#43066=CARTESIAN_POINT('Ctrl Pts',(0.514866728193016,-1.,-4.05431335771199));
#43067=CARTESIAN_POINT('Ctrl Pts',(0.518788572336923,-1.,-4.06097448038013));
#43068=CARTESIAN_POINT('Ctrl Pts',(0.522746528603107,-1.,-4.06762394471314));
#43069=CARTESIAN_POINT('Ctrl Pts',(0.526740277227498,-1.,-4.07426172299847));
#43070=CARTESIAN_POINT('Ctrl Pts',(0.53076951872857,-1.,-4.08088789536836));
#43071=CARTESIAN_POINT('Ctrl Pts',(0.534833963477273,-1.,-4.08750259988885));
#43072=CARTESIAN_POINT('Ctrl Pts',(0.538933321179755,-1.,-4.09410597627));
#43073=CARTESIAN_POINT('Ctrl Pts',(0.543067286877757,-1.,-4.10069810243979));
#43074=CARTESIAN_POINT('Ctrl Pts',(0.547235539485636,-1.,-4.10727897027977));
#43075=CARTESIAN_POINT('Ctrl Pts',(0.551437758497032,-1.,-4.11384852024721));
#43076=CARTESIAN_POINT('Ctrl Pts',(0.555673636129977,-1.,-4.12040666195664));
#43077=CARTESIAN_POINT('Ctrl Pts',(0.559942890594773,-1.,-4.12695329951961));
#43078=CARTESIAN_POINT('Ctrl Pts',(0.564245279537148,-1.,-4.13348835727104));
#43079=CARTESIAN_POINT('Ctrl Pts',(0.568580610189774,-1.,-4.14001179830547));
#43080=CARTESIAN_POINT('Ctrl Pts',(0.572948736069522,-1.,-4.14652361068081));
#43081=CARTESIAN_POINT('Ctrl Pts',(0.576469391676688,-1.,-4.151723761217));
#43082=CARTESIAN_POINT('Ctrl Pts',(0.579124568914235,-1.,-4.15561864788576));
#43083=CARTESIAN_POINT('Ctrl Pts',(0.580901211463535,-1.,-4.1582129171283));
#43084=CARTESIAN_POINT('Ctrl Pts',(0.581791163835815,-1.,-4.15950947128175));
#43085=CARTESIAN_POINT('',(0.73204283740062,-1.,-4.13571194405636));
#43086=CARTESIAN_POINT('',(0.581791163835815,-1.,-4.15950947128175));
#43087=CARTESIAN_POINT('',(0.786422660831985,-1.,-3.66661143271685));
#43088=CARTESIAN_POINT('Ctrl Pts',(0.73204283740062,-1.,-4.13571194405636));
#43089=CARTESIAN_POINT('Ctrl Pts',(0.732488575135159,-1.,-4.1342038373684));
#43090=CARTESIAN_POINT('Ctrl Pts',(0.733376589323546,-1.,-4.13118752795207));
#43091=CARTESIAN_POINT('Ctrl Pts',(0.734698226764092,-1.,-4.12666277570844));
#43092=CARTESIAN_POINT('Ctrl Pts',(0.736439634331344,-1.,-4.120629196238));
#43093=CARTESIAN_POINT('Ctrl Pts',(0.738581708225843,-1.,-4.11308626951927));
#43094=CARTESIAN_POINT('Ctrl Pts',(0.740688998553376,-1.,-4.10554241757547));
#43095=CARTESIAN_POINT('Ctrl Pts',(0.742761369689841,-1.,-4.09799769702611));
#43096=CARTESIAN_POINT('Ctrl Pts',(0.7447986497065,-1.,-4.09045220253573));
#43097=CARTESIAN_POINT('Ctrl Pts',(0.746800631492315,-1.,-4.08290608095642));
#43098=CARTESIAN_POINT('Ctrl Pts',(0.748767076680557,-1.,-4.07535951056152));
#43099=CARTESIAN_POINT('Ctrl Pts',(0.750697720484036,-1.,-4.06781267242378));
#43100=CARTESIAN_POINT('Ctrl Pts',(0.752592276483072,-1.,-4.06026572221515));
#43101=CARTESIAN_POINT('Ctrl Pts',(0.754450441816078,-1.,-4.05271876687915));
#43102=CARTESIAN_POINT('Ctrl Pts',(0.75627190236958,-1.,-4.04517182653997));
#43103=CARTESIAN_POINT('Ctrl Pts',(0.758056338884944,-1.,-4.03762485803119));
#43104=CARTESIAN_POINT('Ctrl Pts',(0.759803433243751,-1.,-4.03007781954412));
#43105=CARTESIAN_POINT('Ctrl Pts',(0.761512875859804,-1.,-4.02253072741268));
#43106=CARTESIAN_POINT('Ctrl Pts',(0.763184371182935,-1.,-4.01498370680496));
#43107=CARTESIAN_POINT('Ctrl Pts',(0.764817648785197,-1.,-4.00743706791509));
#43108=CARTESIAN_POINT('Ctrl Pts',(0.766412457136063,-1.,-3.99989129179622));
#43109=CARTESIAN_POINT('Ctrl Pts',(0.767968531377914,-1.,-3.9923468788101));
#43110=CARTESIAN_POINT('Ctrl Pts',(0.769485566245544,-1.,-3.98480422348451));
#43111=CARTESIAN_POINT('Ctrl Pts',(0.77096319003047,-1.,-3.97726349165488));
#43112=CARTESIAN_POINT('Ctrl Pts',(0.772400931772136,-1.,-3.96972446532772));
#43113=CARTESIAN_POINT('Ctrl Pts',(0.773798212026565,-1.,-3.96218649639807));
#43114=CARTESIAN_POINT('Ctrl Pts',(0.775154418039351,-1.,-3.9546488545231));
#43115=CARTESIAN_POINT('Ctrl Pts',(0.776468966697921,-1.,-3.94711101619447));
#43116=CARTESIAN_POINT('Ctrl Pts',(0.777741370568558,-1.,-3.93957296768103));
#43117=CARTESIAN_POINT('Ctrl Pts',(0.77897130813482,-1.,-3.93203552473174));
#43118=CARTESIAN_POINT('Ctrl Pts',(0.780158678615542,-1.,-3.92450058323823));
#43119=CARTESIAN_POINT('Ctrl Pts',(0.781303428618366,-1.,-3.91697036054676));
#43120=CARTESIAN_POINT('Ctrl Pts',(0.782405395622764,-1.,-3.90944671004542));
#43121=CARTESIAN_POINT('Ctrl Pts',(0.783464141529081,-1.,-3.9019303904397));
#43122=CARTESIAN_POINT('Ctrl Pts',(0.784478799358336,-1.,-3.89442039235103));
#43123=CARTESIAN_POINT('Ctrl Pts',(0.78544789034073,-1.,-3.88691313167398));
#43124=CARTESIAN_POINT('Ctrl Pts',(0.786369675812608,-1.,-3.8794040281819));
#43125=CARTESIAN_POINT('Ctrl Pts',(0.787242527617999,-1.,-3.87188916600912));
#43126=CARTESIAN_POINT('Ctrl Pts',(0.788065315093777,-1.,-3.86436702561345));
#43127=CARTESIAN_POINT('Ctrl Pts',(0.788837734090671,-1.,-3.85683995872529));
#43128=CARTESIAN_POINT('Ctrl Pts',(0.789560798155582,-1.,-3.84931637808894));
#43129=CARTESIAN_POINT('Ctrl Pts',(0.790236124191242,-1.,-3.84180762342454));
#43130=CARTESIAN_POINT('Ctrl Pts',(0.7908650127053,-1.,-3.83432392054786));
#43131=CARTESIAN_POINT('Ctrl Pts',(0.791447528662369,-1.,-3.82687033899792));
#43132=CARTESIAN_POINT('Ctrl Pts',(0.791981740718634,-1.,-3.81944345442249));
#43133=CARTESIAN_POINT('Ctrl Pts',(0.792462483517634,-1.,-3.81202588694756));
#43134=CARTESIAN_POINT('Ctrl Pts',(0.792882695234777,-1.,-3.80459229925637));
#43135=CARTESIAN_POINT('Ctrl Pts',(0.793235612973273,-1.,-3.79711921389897));
#43136=CARTESIAN_POINT('Ctrl Pts',(0.793516871680993,-1.,-3.78959439439235));
#43137=CARTESIAN_POINT('Ctrl Pts',(0.7937262357813,-1.,-3.78202460377598));
#43138=CARTESIAN_POINT('Ctrl Pts',(0.793870523787407,-1.,-3.77444863801212));
#43139=CARTESIAN_POINT('Ctrl Pts',(0.793961083688991,-1.,-3.76692626931111));
#43140=CARTESIAN_POINT('Ctrl Pts',(0.794008429134907,-1.,-3.75951468666257));
#43141=CARTESIAN_POINT('Ctrl Pts',(0.794017347371377,-1.,-3.75224692493864));
#43142=CARTESIAN_POINT('Ctrl Pts',(0.793982700459951,-1.,-3.74511357728861));
#43143=CARTESIAN_POINT('Ctrl Pts',(0.793882700937016,-1.,-3.73803280541687));
#43144=CARTESIAN_POINT('Ctrl Pts',(0.793682750269684,-1.,-3.73086914695805));
#43145=CARTESIAN_POINT('Ctrl Pts',(0.793347023784204,-1.,-3.72348797293734));
#43146=CARTESIAN_POINT('Ctrl Pts',(0.792848377370287,-1.,-3.71580242396124));
#43147=CARTESIAN_POINT('Ctrl Pts',(0.792177688845817,-1.,-3.70781724021806));
#43148=CARTESIAN_POINT('Ctrl Pts',(0.79135657569598,-1.,-3.69968940808721));
#43149=CARTESIAN_POINT('Ctrl Pts',(0.790436284988787,-1.,-3.69172044327364));
#43150=CARTESIAN_POINT('Ctrl Pts',(0.789483546064386,-1.,-3.68428439783905));
#43151=CARTESIAN_POINT('Ctrl Pts',(0.788569566220285,-1.,-3.67777119516252));
#43152=CARTESIAN_POINT('Ctrl Pts',(0.787758799995742,-1.,-3.67252923663655));
#43153=CARTESIAN_POINT('Ctrl Pts',(0.787145041181545,-1.,-3.66907505398677));
#43154=CARTESIAN_POINT('Ctrl Pts',(0.786774337198062,-1.,-3.66743103898702));
#43155=CARTESIAN_POINT('Ctrl Pts',(0.786565919558984,-1.,-3.66680946938292));
#43156=CARTESIAN_POINT('Ctrl Pts',(0.786459983895431,-1.,-3.6666431041522));
#43157=CARTESIAN_POINT('Ctrl Pts',(0.786422660831985,-1.,-3.66661143271685));
#43158=CARTESIAN_POINT('',(0.963899035117249,-1.,-3.62400312501245));
#43159=CARTESIAN_POINT('Origin',(0.,-1.,0.));
#43160=CARTESIAN_POINT('',(1.22531898815164,-1.,-4.01728681790024));
#43161=CARTESIAN_POINT('Ctrl Pts',(0.963899035117249,-1.,-3.62400312501245));
#43162=CARTESIAN_POINT('Ctrl Pts',(0.963880158555582,-1.,-3.6240482887845));
#43163=CARTESIAN_POINT('Ctrl Pts',(0.963861297423241,-1.,-3.62424461507588));
#43164=CARTESIAN_POINT('Ctrl Pts',(0.963957782642843,-1.,-3.62489305727662));
#43165=CARTESIAN_POINT('Ctrl Pts',(0.964373850166457,-1.,-3.62652618145335));
#43166=CARTESIAN_POINT('Ctrl Pts',(0.965395153165293,-1.,-3.62988252139846));
#43167=CARTESIAN_POINT('Ctrl Pts',(0.967052554541385,-1.,-3.63492122081143));
#43168=CARTESIAN_POINT('Ctrl Pts',(0.969195124675865,-1.,-3.64113946505766));
#43169=CARTESIAN_POINT('Ctrl Pts',(0.971722122061341,-1.,-3.64819756447455));
#43170=CARTESIAN_POINT('Ctrl Pts',(0.974519971354848,-1.,-3.65571576735126));
#43171=CARTESIAN_POINT('Ctrl Pts',(0.977478312751618,-1.,-3.66333049637475));
#43172=CARTESIAN_POINT('Ctrl Pts',(0.980505922458267,-1.,-3.67074983340361));
#43173=CARTESIAN_POINT('Ctrl Pts',(0.983550791470419,-1.,-3.67782408841715));
#43174=CARTESIAN_POINT('Ctrl Pts',(0.986602639863837,-1.,-3.68455317926068));
#43175=CARTESIAN_POINT('Ctrl Pts',(0.989676715398558,-1.,-3.69102682138847));
#43176=CARTESIAN_POINT('Ctrl Pts',(0.99280221833201,-1.,-3.69738123415662));
#43177=CARTESIAN_POINT('Ctrl Pts',(0.996009819772518,-1.,-3.70375282282138));
#43178=CARTESIAN_POINT('Ctrl Pts',(0.99931726075653,-1.,-3.71022439713938));
#43179=CARTESIAN_POINT('Ctrl Pts',(1.00272423396822,-1.,-3.71680667125119));
#43180=CARTESIAN_POINT('Ctrl Pts',(1.0062200073571,-1.,-3.72346803750596));
#43181=CARTESIAN_POINT('Ctrl Pts',(1.00978798539496,-1.,-3.73015276704426));
#43182=CARTESIAN_POINT('Ctrl Pts',(1.01341114319903,-1.,-3.73680245055734));
#43183=CARTESIAN_POINT('Ctrl Pts',(1.01707794311079,-1.,-3.74337942504959));
#43184=CARTESIAN_POINT('Ctrl Pts',(1.02078510487428,-1.,-3.74987777155834));
#43185=CARTESIAN_POINT('Ctrl Pts',(1.0245342944466,-1.,-3.75631037456194));
#43186=CARTESIAN_POINT('Ctrl Pts',(1.02833014458181,-1.,-3.76270122291232));
#43187=CARTESIAN_POINT('Ctrl Pts',(1.0321778660492,-1.,-3.76907609832522));
#43188=CARTESIAN_POINT('Ctrl Pts',(1.03608074678013,-1.,-3.77545283140445));
#43189=CARTESIAN_POINT('Ctrl Pts',(1.04003862055804,-1.,-3.78183535008192));
#43190=CARTESIAN_POINT('Ctrl Pts',(1.04404924374426,-1.,-3.78821910787195));
#43191=CARTESIAN_POINT('Ctrl Pts',(1.04810913267641,-1.,-3.79459440308793));
#43192=CARTESIAN_POINT('Ctrl Pts',(1.05221457990015,-1.,-3.80095039790678));
#43193=CARTESIAN_POINT('Ctrl Pts',(1.05636266918643,-1.,-3.80727913637784));
#43194=CARTESIAN_POINT('Ctrl Pts',(1.06055206187298,-1.,-3.81357866117485));
#43195=CARTESIAN_POINT('Ctrl Pts',(1.06478244038931,-1.,-3.81985083953012));
#43196=CARTESIAN_POINT('Ctrl Pts',(1.0690541318036,-1.,-3.82609989967278));
#43197=CARTESIAN_POINT('Ctrl Pts',(1.0733676663346,-1.,-3.83233071195145));
#43198=CARTESIAN_POINT('Ctrl Pts',(1.07772335353856,-1.,-3.83854714117486));
#43199=CARTESIAN_POINT('Ctrl Pts',(1.08212087917986,-1.,-3.84475048030615));
#43200=CARTESIAN_POINT('Ctrl Pts',(1.08655950846377,-1.,-3.85094025222691));
#43201=CARTESIAN_POINT('Ctrl Pts',(1.09103825516288,-1.,-3.85711487933911));
#43202=CARTESIAN_POINT('Ctrl Pts',(1.09555606505012,-1.,-3.86327241021242));
#43203=CARTESIAN_POINT('Ctrl Pts',(1.10011198761202,-1.,-3.86941120134872));
#43204=CARTESIAN_POINT('Ctrl Pts',(1.10470536603303,-1.,-3.87553067187566));
#43205=CARTESIAN_POINT('Ctrl Pts',(1.10933577224029,-1.,-3.88163105531791));
#43206=CARTESIAN_POINT('Ctrl Pts',(1.11400292434447,-1.,-3.88771308285229));
#43207=CARTESIAN_POINT('Ctrl Pts',(1.11870660794609,-1.,-3.89377768340362));
#43208=CARTESIAN_POINT('Ctrl Pts',(1.12344660099029,-1.,-3.89982569749978));
#43209=CARTESIAN_POINT('Ctrl Pts',(1.12822258281518,-1.,-3.90585753318622));
#43210=CARTESIAN_POINT('Ctrl Pts',(1.13303414693849,-1.,-3.91187321145495));
#43211=CARTESIAN_POINT('Ctrl Pts',(1.13788084225511,-1.,-3.91787251936688));
#43212=CARTESIAN_POINT('Ctrl Pts',(1.14276220561575,-1.,-3.92385513133937));
#43213=CARTESIAN_POINT('Ctrl Pts',(1.14767779451147,-1.,-3.92982073294334));
#43214=CARTESIAN_POINT('Ctrl Pts',(1.1526272271639,-1.,-3.9357691705651));
#43215=CARTESIAN_POINT('Ctrl Pts',(1.1576101834106,-1.,-3.94170046685542));
#43216=CARTESIAN_POINT('Ctrl Pts',(1.16262637999261,-1.,-3.9476147478092));
#43217=CARTESIAN_POINT('Ctrl Pts',(1.16767555244495,-1.,-3.95351219510062));
#43218=CARTESIAN_POINT('Ctrl Pts',(1.17275743590327,-1.,-3.95939299213164));
#43219=CARTESIAN_POINT('Ctrl Pts',(1.17787174135445,-1.,-3.96525726357682));
#43220=CARTESIAN_POINT('Ctrl Pts',(1.18301815039596,-1.,-3.9711050516465));
#43221=CARTESIAN_POINT('Ctrl Pts',(1.18819633715285,-1.,-3.97693634766926));
#43222=CARTESIAN_POINT('Ctrl Pts',(1.19340598349307,-1.,-3.98275111052015));
#43223=CARTESIAN_POINT('Ctrl Pts',(1.19864679609596,-1.,-3.98854928957287));
#43224=CARTESIAN_POINT('Ctrl Pts',(1.2039185237544,-1.,-3.99433084800649));
#43225=CARTESIAN_POINT('Ctrl Pts',(1.20922097030107,-1.,-4.00009577952534));
#43226=CARTESIAN_POINT('Ctrl Pts',(1.21455398918813,-1.,-4.00584409524937));
#43227=CARTESIAN_POINT('Ctrl Pts',(1.21884478244983,-1.,-4.01042947142681));
#43228=CARTESIAN_POINT('Ctrl Pts',(1.22207656456199,-1.,-4.01386104434674));
#43229=CARTESIAN_POINT('Ctrl Pts',(1.22423716681447,-1.,-4.0161454457032));
#43230=CARTESIAN_POINT('Ctrl Pts',(1.22531898815164,-1.,-4.01728681790024));
#43231=CARTESIAN_POINT('',(1.36999806084572,-1.,-3.97027773754922));
#43232=CARTESIAN_POINT('',(1.22531898815164,-1.,-4.01728681790024));
#43233=CARTESIAN_POINT('',(1.35032489087101,-1.,-3.4984457533445));
#43234=CARTESIAN_POINT('Ctrl Pts',(1.36999806084572,-1.,-3.97027773754922));
#43235=CARTESIAN_POINT('Ctrl Pts',(1.37020239094614,-1.,-3.9687184694131));
#43236=CARTESIAN_POINT('Ctrl Pts',(1.37060761745635,-1.,-3.96560037974645));
#43237=CARTESIAN_POINT('Ctrl Pts',(1.3712051561502,-1.,-3.96092458506535));
#43238=CARTESIAN_POINT('Ctrl Pts',(1.37198126432386,-1.,-3.95469287280914));
#43239=CARTESIAN_POINT('Ctrl Pts',(1.37291699202807,-1.,-3.94690771785133));
#43240=CARTESIAN_POINT('Ctrl Pts',(1.37381821967165,-1.,-3.93912709040818));
#43241=CARTESIAN_POINT('Ctrl Pts',(1.37468482215751,-1.,-3.93135106761844));
#43242=CARTESIAN_POINT('Ctrl Pts',(1.37551664448242,-1.,-3.92357976987672));
#43243=CARTESIAN_POINT('Ctrl Pts',(1.37631350505797,-1.,-3.91581337462644));
#43244=CARTESIAN_POINT('Ctrl Pts',(1.3770751963402,-1.,-3.90805209523486));
#43245=CARTESIAN_POINT('Ctrl Pts',(1.37780148512792,-1.,-3.90029615196727));
#43246=CARTESIAN_POINT('Ctrl Pts',(1.3784921128802,-1.,-3.89254574338496));
#43247=CARTESIAN_POINT('Ctrl Pts',(1.37914679719383,-1.,-3.88480102249278));
#43248=CARTESIAN_POINT('Ctrl Pts',(1.37976523097073,-1.,-3.87706205830532));
#43249=CARTESIAN_POINT('Ctrl Pts',(1.38034709213014,-1.,-3.86932885813068));
#43250=CARTESIAN_POINT('Ctrl Pts',(1.38089205992989,-1.,-3.86160143043959));
#43251=CARTESIAN_POINT('Ctrl Pts',(1.38139983115049,-1.,-3.85387983979481));
#43252=CARTESIAN_POINT('Ctrl Pts',(1.38187013346109,-1.,-3.84616425605764));
#43253=CARTESIAN_POINT('Ctrl Pts',(1.38230274828821,-1.,-3.83845502790746));
#43254=CARTESIAN_POINT('Ctrl Pts',(1.38269750245138,-1.,-3.8307526698229));
#43255=CARTESIAN_POINT('Ctrl Pts',(1.38305421262763,-1.,-3.82305771743829));
#43256=CARTESIAN_POINT('Ctrl Pts',(1.38337263902782,-1.,-3.81537060817811));
#43257=CARTESIAN_POINT('Ctrl Pts',(1.3836524404622,-1.,-3.80769156398411));
#43258=CARTESIAN_POINT('Ctrl Pts',(1.38389311766682,-1.,-3.80002044322111));
#43259=CARTESIAN_POINT('Ctrl Pts',(1.38409399694566,-1.,-3.79235669640841));
#43260=CARTESIAN_POINT('Ctrl Pts',(1.38425435883756,-1.,-3.78469969805082));
#43261=CARTESIAN_POINT('Ctrl Pts',(1.38437354551428,-1.,-3.77704902230418));
#43262=CARTESIAN_POINT('Ctrl Pts',(1.38445107339518,-1.,-3.76940473185779));
#43263=CARTESIAN_POINT('Ctrl Pts',(1.3844867525335,-1.,-3.76176768271367));
#43264=CARTESIAN_POINT('Ctrl Pts',(1.38448077997163,-1.,-3.7541397631875));
#43265=CARTESIAN_POINT('Ctrl Pts',(1.38443344984394,-1.,-3.74652317167876));
#43266=CARTESIAN_POINT('Ctrl Pts',(1.38434489156458,-1.,-3.73891976418104));
#43267=CARTESIAN_POINT('Ctrl Pts',(1.38421479111531,-1.,-3.73133035859282));
#43268=CARTESIAN_POINT('Ctrl Pts',(1.3840421342895,-1.,-3.72375409358803));
#43269=CARTESIAN_POINT('Ctrl Pts',(1.38382489984586,-1.,-3.7161876605181));
#43270=CARTESIAN_POINT('Ctrl Pts',(1.38356065402124,-1.,-3.70862680753347));
#43271=CARTESIAN_POINT('Ctrl Pts',(1.38324717612865,-1.,-3.701067921679));
#43272=CARTESIAN_POINT('Ctrl Pts',(1.3828831117165,-1.,-3.69350967899526));
#43273=CARTESIAN_POINT('Ctrl Pts',(1.38246852827182,-1.,-3.68595444983838));
#43274=CARTESIAN_POINT('Ctrl Pts',(1.3820057429062,-1.,-3.67841038482414));
#43275=CARTESIAN_POINT('Ctrl Pts',(1.38149812653868,-1.,-3.67088843112262));
#43276=CARTESIAN_POINT('Ctrl Pts',(1.38094856333552,-1.,-3.66339848520857));
#43277=CARTESIAN_POINT('Ctrl Pts',(1.38035791051212,-1.,-3.6559455440439));
#43278=CARTESIAN_POINT('Ctrl Pts',(1.37972372481603,-1.,-3.64852652756456));
#43279=CARTESIAN_POINT('Ctrl Pts',(1.37903818567359,-1.,-3.64112507791141));
#43280=CARTESIAN_POINT('Ctrl Pts',(1.37829035457339,-1.,-3.63371727442486));
#43281=CARTESIAN_POINT('Ctrl Pts',(1.37746987919881,-1.,-3.62628098665145));
#43282=CARTESIAN_POINT('Ctrl Pts',(1.37657053403107,-1.,-3.61880481160421));
#43283=CARTESIAN_POINT('Ctrl Pts',(1.37559314436634,-1.,-3.61129546591064));
#43284=CARTESIAN_POINT('Ctrl Pts',(1.37455051379623,-1.,-3.60379020123988));
#43285=CARTESIAN_POINT('Ctrl Pts',(1.37346320103157,-1.,-3.59634627869048));
#43286=CARTESIAN_POINT('Ctrl Pts',(1.37235053660976,-1.,-3.58901853846365));
#43287=CARTESIAN_POINT('Ctrl Pts',(1.37122241663062,-1.,-3.58183885982715));
#43288=CARTESIAN_POINT('Ctrl Pts',(1.37007229485659,-1.,-3.57479875549486));
#43289=CARTESIAN_POINT('Ctrl Pts',(1.36886584973389,-1.,-3.5678208030466));
#43290=CARTESIAN_POINT('Ctrl Pts',(1.36754771771233,-1.,-3.56077662028649));
#43291=CARTESIAN_POINT('Ctrl Pts',(1.3660614545677,-1.,-3.55353883995949));
#43292=CARTESIAN_POINT('Ctrl Pts',(1.36436666257597,-1.,-3.54602591832973));
#43293=CARTESIAN_POINT('Ctrl Pts',(1.36245507339307,-1.,-3.53824396424961));
#43294=CARTESIAN_POINT('Ctrl Pts',(1.36037259643734,-1.,-3.530344649616));
#43295=CARTESIAN_POINT('Ctrl Pts',(1.35821701528836,-1.,-3.52261776116748));
#43296=CARTESIAN_POINT('Ctrl Pts',(1.35611275237152,-1.,-3.51542230699556));
#43297=CARTESIAN_POINT('Ctrl Pts',(1.35419113575956,-1.,-3.50913227059999));
#43298=CARTESIAN_POINT('Ctrl Pts',(1.35257032843486,-1.,-3.50408168106261));
#43299=CARTESIAN_POINT('Ctrl Pts',(1.35142377279517,-1.,-3.5007660381649));
#43300=CARTESIAN_POINT('Ctrl Pts',(1.35080045218586,-1.,-3.49920025459723));
#43301=CARTESIAN_POINT('Ctrl Pts',(1.35049736560527,-1.,-3.49861894124827));
#43302=CARTESIAN_POINT('Ctrl Pts',(1.35036670892966,-1.,-3.49847119623846));
#43303=CARTESIAN_POINT('Ctrl Pts',(1.35032489087101,-1.,-3.4984457533445));
#43304=CARTESIAN_POINT('',(1.51895082866166,-1.,-3.42859860294378));
#43305=CARTESIAN_POINT('Origin',(0.,-1.,0.));
#43306=CARTESIAN_POINT('',(1.83867539237861,-1.,-3.77614523045147));
#43307=CARTESIAN_POINT('Ctrl Pts',(1.51895082866166,-1.,-3.42859860294378));
#43308=CARTESIAN_POINT('Ctrl Pts',(1.51893924967231,-1.,-3.42864616361967));
#43309=CARTESIAN_POINT('Ctrl Pts',(1.51895133295017,-1.,-3.42884302333978));
#43310=CARTESIAN_POINT('Ctrl Pts',(1.51914806898539,-1.,-3.42946838852728));
#43311=CARTESIAN_POINT('Ctrl Pts',(1.5198144909343,-1.,-3.43101631893491));
#43312=CARTESIAN_POINT('Ctrl Pts',(1.52134826724227,-1.,-3.43417156977749));
#43313=CARTESIAN_POINT('Ctrl Pts',(1.52377348950429,-1.,-3.43888895974182));
#43314=CARTESIAN_POINT('Ctrl Pts',(1.52686242875717,-1.,-3.44469547527));
#43315=CARTESIAN_POINT('Ctrl Pts',(1.530462444618,-1.,-3.45127136828667));
#43316=CARTESIAN_POINT('Ctrl Pts',(1.53440195378902,-1.,-3.45825932955273));
#43317=CARTESIAN_POINT('Ctrl Pts',(1.53851507915533,-1.,-3.46531752207222));
#43318=CARTESIAN_POINT('Ctrl Pts',(1.54266605398152,-1.,-3.47217189224576));
#43319=CARTESIAN_POINT('Ctrl Pts',(1.54678009290206,-1.,-3.47868272898599));
#43320=CARTESIAN_POINT('Ctrl Pts',(1.55084702970382,-1.,-3.48485155928414));
#43321=CARTESIAN_POINT('Ctrl Pts',(1.5548959590107,-1.,-3.49076460877317));
#43322=CARTESIAN_POINT('Ctrl Pts',(1.55897703097859,-1.,-3.49655185179623));
#43323=CARTESIAN_POINT('Ctrl Pts',(1.56314187758689,-1.,-3.50234321621607));
#43324=CARTESIAN_POINT('Ctrl Pts',(1.56742097575041,-1.,-3.50821771695427));
#43325=CARTESIAN_POINT('Ctrl Pts',(1.57181569799774,-1.,-3.51418598431733));
#43326=CARTESIAN_POINT('Ctrl Pts',(1.5763104998818,-1.,-3.52021847865961));
#43327=CARTESIAN_POINT('Ctrl Pts',(1.58088027227856,-1.,-3.52626275334899));
#43328=CARTESIAN_POINT('Ctrl Pts',(1.58549906268083,-1.,-3.53226378147068));
#43329=CARTESIAN_POINT('Ctrl Pts',(1.59014958368725,-1.,-3.53818616861045));
#43330=CARTESIAN_POINT('Ctrl Pts',(1.5948276694975,-1.,-3.544024581823));
#43331=CARTESIAN_POINT('Ctrl Pts',(1.59953698113444,-1.,-3.54979148634426));
#43332=CARTESIAN_POINT('Ctrl Pts',(1.60428584699848,-1.,-3.55550985096117));
#43333=CARTESIAN_POINT('Ctrl Pts',(1.60908344685459,-1.,-3.56120432482986));
#43334=CARTESIAN_POINT('Ctrl Pts',(1.61393581747522,-1.,-3.56689200468404));
#43335=CARTESIAN_POINT('Ctrl Pts',(1.61884340915412,-1.,-3.57257679609826));
#43336=CARTESIAN_POINT('Ctrl Pts',(1.62380329464851,-1.,-3.57825455954405));
#43337=CARTESIAN_POINT('Ctrl Pts',(1.62881051550748,-1.,-3.5839162577435));
#43338=CARTESIAN_POINT('Ctrl Pts',(1.63385971451259,-1.,-3.58955176627876));
#43339=CARTESIAN_POINT('Ctrl Pts',(1.63894676675349,-1.,-3.59515368334887));
#43340=CARTESIAN_POINT('Ctrl Pts',(1.6440700438558,-1.,-3.6007202851384));
#43341=CARTESIAN_POINT('Ctrl Pts',(1.64922952425833,-1.,-3.60625346556992));
#43342=CARTESIAN_POINT('Ctrl Pts',(1.65442619244327,-1.,-3.61175734965129));
#43343=CARTESIAN_POINT('Ctrl Pts',(1.65966133399186,-1.,-3.61723666482457));
#43344=CARTESIAN_POINT('Ctrl Pts',(1.66493585923853,-1.,-3.62269517989104));
#43345=CARTESIAN_POINT('Ctrl Pts',(1.67024966008037,-1.,-3.62813422105257));
#43346=CARTESIAN_POINT('Ctrl Pts',(1.67560193613145,-1.,-3.63355343201211));
#43347=CARTESIAN_POINT('Ctrl Pts',(1.68099146651577,-1.,-3.63895140887443));
#43348=CARTESIAN_POINT('Ctrl Pts',(1.68641690471455,-1.,-3.64432638915199));
#43349=CARTESIAN_POINT('Ctrl Pts',(1.691877054817,-1.,-3.64967689827393));
#43350=CARTESIAN_POINT('Ctrl Pts',(1.69737117722558,-1.,-3.65500246526798));
#43351=CARTESIAN_POINT('Ctrl Pts',(1.70289888566904,-1.,-3.6603033877491));
#43352=CARTESIAN_POINT('Ctrl Pts',(1.70846001610983,-1.,-3.6655804319893));
#43353=CARTESIAN_POINT('Ctrl Pts',(1.71405450210392,-1.,-3.67083454901629));
#43354=CARTESIAN_POINT('Ctrl Pts',(1.71968225581787,-1.,-3.67606660374665));
#43355=CARTESIAN_POINT('Ctrl Pts',(1.72534302437003,-1.,-3.68127704936472));
#43356=CARTESIAN_POINT('Ctrl Pts',(1.73103640956647,-1.,-3.68646597019188));
#43357=CARTESIAN_POINT('Ctrl Pts',(1.73676193254493,-1.,-3.69163322647906));
#43358=CARTESIAN_POINT('Ctrl Pts',(1.74251908492589,-1.,-3.6967785691046));
#43359=CARTESIAN_POINT('Ctrl Pts',(1.74830738046092,-1.,-3.70190175673422));
#43360=CARTESIAN_POINT('Ctrl Pts',(1.75412641804148,-1.,-3.70700269736876));
#43361=CARTESIAN_POINT('Ctrl Pts',(1.75997588499021,-1.,-3.71208146346455));
#43362=CARTESIAN_POINT('Ctrl Pts',(1.76585552124549,-1.,-3.71713822377676));
#43363=CARTESIAN_POINT('Ctrl Pts',(1.77176509401846,-1.,-3.72217319911429));
#43364=CARTESIAN_POINT('Ctrl Pts',(1.77770437039606,-1.,-3.72718661205504));
#43365=CARTESIAN_POINT('Ctrl Pts',(1.78367308442682,-1.,-3.73217863095022));
#43366=CARTESIAN_POINT('Ctrl Pts',(1.78967092823139,-1.,-3.73714934729962));
#43367=CARTESIAN_POINT('Ctrl Pts',(1.79569757859041,-1.,-3.74209880351667));
#43368=CARTESIAN_POINT('Ctrl Pts',(1.80175271485519,-1.,-3.74702700874954));
#43369=CARTESIAN_POINT('Ctrl Pts',(1.80783603939662,-1.,-3.75193395888069));
#43370=CARTESIAN_POINT('Ctrl Pts',(1.81394729834032,-1.,-3.75681965683995));
#43371=CARTESIAN_POINT('Ctrl Pts',(1.82008629694924,-1.,-3.76168412709652));
#43372=CARTESIAN_POINT('Ctrl Pts',(1.82625289221933,-1.,-3.76652740355856));
#43373=CARTESIAN_POINT('Ctrl Pts',(1.83120816956515,-1.,-3.77038509819777));
#43374=CARTESIAN_POINT('Ctrl Pts',(1.83493697935064,-1.,-3.77326886065484));
#43375=CARTESIAN_POINT('Ctrl Pts',(1.83742834010821,-1.,-3.77518714458232));
#43376=CARTESIAN_POINT('Ctrl Pts',(1.83867539237861,-1.,-3.77614523045147));
#43377=CARTESIAN_POINT('',(1.97421938526992,-1.,-3.70708211654725));
#43378=CARTESIAN_POINT('',(1.83867539237861,-1.,-3.77614523045147));
#43379=CARTESIAN_POINT('',(1.88097764062541,-1.,-3.24413672884902));
#43380=CARTESIAN_POINT('Ctrl Pts',(1.97421938526992,-1.,-3.70708211654725));
#43381=CARTESIAN_POINT('Ctrl Pts',(1.974177276451,-1.,-3.7055100813194));
#43382=CARTESIAN_POINT('Ctrl Pts',(1.97408973726149,-1.,-3.70236698911837));
#43383=CARTESIAN_POINT('Ctrl Pts',(1.97394846382288,-1.,-3.69765528558292));
#43384=CARTESIAN_POINT('Ctrl Pts',(1.97374016224397,-1.,-3.69137888597855));
#43385=CARTESIAN_POINT('Ctrl Pts',(1.9734465030363,-1.,-3.68354319913416));
#43386=CARTESIAN_POINT('Ctrl Pts',(1.97311947678035,-1.,-3.67571738106175));
#43387=CARTESIAN_POINT('Ctrl Pts',(1.9727589719863,-1.,-3.66790152751984));
#43388=CARTESIAN_POINT('Ctrl Pts',(1.97236485439317,-1.,-3.66009578166865));
#43389=CARTESIAN_POINT('Ctrl Pts',(1.97193697240645,-1.,-3.65230034717364));
#43390=CARTESIAN_POINT('Ctrl Pts',(1.97147515441539,-1.,-3.64451546724222));
#43391=CARTESIAN_POINT('Ctrl Pts',(1.97097920454698,-1.,-3.63674139590853));
#43392=CARTESIAN_POINT('Ctrl Pts',(1.97044889850518,-1.,-3.62897836973397));
#43393=CARTESIAN_POINT('Ctrl Pts',(1.96988398129888,-1.,-3.62122658401722));
#43394=CARTESIAN_POINT('Ctrl Pts',(1.96928416040712,-1.,-3.61348615496393));
#43395=CARTESIAN_POINT('Ctrl Pts',(1.96864911885775,-1.,-3.60575714017676));
#43396=CARTESIAN_POINT('Ctrl Pts',(1.96797854118257,-1.,-3.59803959819725));
#43397=CARTESIAN_POINT('Ctrl Pts',(1.96727213799507,-1.,-3.5903336402273));
#43398=CARTESIAN_POINT('Ctrl Pts',(1.9665296668894,-1.,-3.58263947663884));
#43399=CARTESIAN_POINT('Ctrl Pts',(1.96575096652857,-1.,-3.57495748601088));
#43400=CARTESIAN_POINT('Ctrl Pts',(1.96493594634643,-1.,-3.56728820357933));
#43401=CARTESIAN_POINT('Ctrl Pts',(1.96408450906868,-1.,-3.55963218706201));
#43402=CARTESIAN_POINT('Ctrl Pts',(1.96319648628667,-1.,-3.55198990600929));
#43403=CARTESIAN_POINT('Ctrl Pts',(1.96227157573058,-1.,-3.54436163300425));
#43404=CARTESIAN_POINT('Ctrl Pts',(1.96130926212661,-1.,-3.53674730625759));
#43405=CARTESIAN_POINT('Ctrl Pts',(1.96030879411534,-1.,-3.52914648844289));
#43406=CARTESIAN_POINT('Ctrl Pts',(1.95926936324436,-1.,-3.52155867431438));
#43407=CARTESIAN_POINT('Ctrl Pts',(1.95819025316768,-1.,-3.51398354617773));
#43408=CARTESIAN_POINT('Ctrl Pts',(1.95707099606513,-1.,-3.50642124159913));
#43409=CARTESIAN_POINT('Ctrl Pts',(1.9559115382367,-1.,-3.49887263575602));
#43410=CARTESIAN_POINT('Ctrl Pts',(1.95471236969653,-1.,-3.49133956289154));
#43411=CARTESIAN_POINT('Ctrl Pts',(1.95347412486316,-1.,-3.48382414832649));
#43412=CARTESIAN_POINT('Ctrl Pts',(1.95219722189878,-1.,-3.47632820495926));
#43413=CARTESIAN_POINT('Ctrl Pts',(1.95088147859876,-1.,-3.4688525897419));
#43414=CARTESIAN_POINT('Ctrl Pts',(1.94952575850196,-1.,-3.46139661060959));
#43415=CARTESIAN_POINT('Ctrl Pts',(1.94812754766524,-1.,-3.45395731584051));
#43416=CARTESIAN_POINT('Ctrl Pts',(1.94668377715332,-1.,-3.44653088665685));
#43417=CARTESIAN_POINT('Ctrl Pts',(1.94519168842883,-1.,-3.43911410197693));
#43418=CARTESIAN_POINT('Ctrl Pts',(1.94364973660285,-1.,-3.43170586602436));
#43419=CARTESIAN_POINT('Ctrl Pts',(1.94205835913692,-1.,-3.42430850941497));
#43420=CARTESIAN_POINT('Ctrl Pts',(1.94042111965237,-1.,-3.41692971994082));
#43421=CARTESIAN_POINT('Ctrl Pts',(1.93874306008132,-1.,-3.40957978266623));
#43422=CARTESIAN_POINT('Ctrl Pts',(1.93702857723089,-1.,-3.40226802104093));
#43423=CARTESIAN_POINT('Ctrl Pts',(1.93527929945982,-1.,-3.39499923640789));
#43424=CARTESIAN_POINT('Ctrl Pts',(1.93349233176794,-1.,-3.38777076883267));
#43425=CARTESIAN_POINT('Ctrl Pts',(1.93165739093292,-1.,-3.38056768525577));
#43426=CARTESIAN_POINT('Ctrl Pts',(1.92975993109897,-1.,-3.37336807068078));
#43427=CARTESIAN_POINT('Ctrl Pts',(1.92778626543803,-1.,-3.36615168657597));
#43428=CARTESIAN_POINT('Ctrl Pts',(1.92572846125763,-1.,-3.35890824422976));
#43429=CARTESIAN_POINT('Ctrl Pts',(1.92358838440518,-1.,-3.35164424847207));
#43430=CARTESIAN_POINT('Ctrl Pts',(1.92138450828378,-1.,-3.34439448941915));
#43431=CARTESIAN_POINT('Ctrl Pts',(1.91914609610173,-1.,-3.33721230709948));
#43432=CARTESIAN_POINT('Ctrl Pts',(1.91690081930297,-1.,-3.33014884257812));
#43433=CARTESIAN_POINT('Ctrl Pts',(1.91466343916612,-1.,-3.32323403454507));
#43434=CARTESIAN_POINT('Ctrl Pts',(1.91242616234459,-1.,-3.31646052426395));
#43435=CARTESIAN_POINT('Ctrl Pts',(1.91014297830502,-1.,-3.30975721158694));
#43436=CARTESIAN_POINT('Ctrl Pts',(1.90773912171424,-1.,-3.30300595568341));
#43437=CARTESIAN_POINT('Ctrl Pts',(1.9051389186417,-1.,-3.29608978722258));
#43438=CARTESIAN_POINT('Ctrl Pts',(1.9022897124757,-1.,-3.28893448600364));
#43439=CARTESIAN_POINT('Ctrl Pts',(1.89918429230424,-1.,-3.28154737912287));
#43440=CARTESIAN_POINT('Ctrl Pts',(1.89589172903662,-1.,-3.27407108932908));
#43441=CARTESIAN_POINT('Ctrl Pts',(1.89255393500769,-1.,-3.2667765388833));
#43442=CARTESIAN_POINT('Ctrl Pts',(1.88934996203508,-1.,-3.2599988519361));
#43443=CARTESIAN_POINT('Ctrl Pts',(1.88646802523372,-1.,-3.25408686339298));
#43444=CARTESIAN_POINT('Ctrl Pts',(1.88407708646435,-1.,-3.24935200512055));
#43445=CARTESIAN_POINT('Ctrl Pts',(1.88242596600422,-1.,-3.24625654410705));
#43446=CARTESIAN_POINT('Ctrl Pts',(1.88156537699118,-1.,-3.24480754675942));
#43447=CARTESIAN_POINT('Ctrl Pts',(1.88117508446657,-1.,-3.24428080352952));
#43448=CARTESIAN_POINT('Ctrl Pts',(1.88102292397987,-1.,-3.24415531671311));
#43449=CARTESIAN_POINT('Ctrl Pts',(1.88097764062541,-1.,-3.24413672884902));
#43450=CARTESIAN_POINT('',(2.03660101169564,-1.,-3.14877060440425));
#43451=CARTESIAN_POINT('Origin',(0.,-1.,0.));
#43452=CARTESIAN_POINT('',(2.40675750623143,-1.,-3.44202241512147));
#43453=CARTESIAN_POINT('Ctrl Pts',(2.03660101169564,-1.,-3.14877060440425));
#43454=CARTESIAN_POINT('Ctrl Pts',(2.03659701539175,-1.,-3.1488193908823));
#43455=CARTESIAN_POINT('Ctrl Pts',(2.03663974554941,-1.,-3.14901193669147));
#43456=CARTESIAN_POINT('Ctrl Pts',(2.03693188810614,-1.,-3.14959882629936));
#43457=CARTESIAN_POINT('Ctrl Pts',(2.03783225496023,-1.,-3.15102344775396));
#43458=CARTESIAN_POINT('Ctrl Pts',(2.03984073791432,-1.,-3.1538999167466));
#43459=CARTESIAN_POINT('Ctrl Pts',(2.04297406404132,-1.,-3.15817983946525));
#43460=CARTESIAN_POINT('Ctrl Pts',(2.0469333124766,-1.,-3.16343165059235));
#43461=CARTESIAN_POINT('Ctrl Pts',(2.05151770247452,-1.,-3.16936341689859));
#43462=CARTESIAN_POINT('Ctrl Pts',(2.05650186773279,-1.,-3.17564906975592));
#43463=CARTESIAN_POINT('Ctrl Pts',(2.06166849827143,-1.,-3.18197692964677));
#43464=CARTESIAN_POINT('Ctrl Pts',(2.06684062744065,-1.,-3.18809755562297));
#43465=CARTESIAN_POINT('Ctrl Pts',(2.07192253497765,-1.,-3.19388465568113));
#43466=CARTESIAN_POINT('Ctrl Pts',(2.0769044187063,-1.,-3.19934132835879));
#43467=CARTESIAN_POINT('Ctrl Pts',(2.08182850370816,-1.,-3.20454818630635));
#43468=CARTESIAN_POINT('Ctrl Pts',(2.08676465517435,-1.,-3.20962575845433));
#43469=CARTESIAN_POINT('Ctrl Pts',(2.0917841946046,-1.,-3.2146942960168));
#43470=CARTESIAN_POINT('Ctrl Pts',(2.09692958434933,-1.,-3.21982707347067));
#43471=CARTESIAN_POINT('Ctrl Pts',(2.10220384298533,-1.,-3.22503437553496));
#43472=CARTESIAN_POINT('Ctrl Pts',(2.1075869964248,-1.,-3.23028945793334));
#43473=CARTESIAN_POINT('Ctrl Pts',(2.11304604021784,-1.,-3.23554444767115));
#43474=CARTESIAN_POINT('Ctrl Pts',(2.11854673326972,-1.,-3.24074905517282));
#43475=CARTESIAN_POINT('Ctrl Pts',(2.12406646410943,-1.,-3.24587102613347));
#43476=CARTESIAN_POINT('Ctrl Pts',(2.1296002839681,-1.,-3.25090574493994));
#43477=CARTESIAN_POINT('Ctrl Pts',(2.13515375878786,-1.,-3.25586495065027));
#43478=CARTESIAN_POINT('Ctrl Pts',(2.14073870754257,-1.,-3.26077002641868));
#43479=CARTESIAN_POINT('Ctrl Pts',(2.14636805295663,-1.,-3.26564388189764));
#43480=CARTESIAN_POINT('Ctrl Pts',(2.15205043199818,-1.,-3.27050245897244));
#43481=CARTESIAN_POINT('Ctrl Pts',(2.15778690038359,-1.,-3.27534954469206));
#43482=CARTESIAN_POINT('Ctrl Pts',(2.16357391934434,-1.,-3.28018150841414));
#43483=CARTESIAN_POINT('Ctrl Pts',(2.16940517773459,-1.,-3.2849901997973));
#43484=CARTESIAN_POINT('Ctrl Pts',(2.17527380048422,-1.,-3.28976645712566));
#43485=CARTESIAN_POINT('Ctrl Pts',(2.18117455557062,-1.,-3.29450361500484));
#43486=CARTESIAN_POINT('Ctrl Pts',(2.18710556500325,-1.,-3.29920022557635));
#43487=CARTESIAN_POINT('Ctrl Pts',(2.19306710376112,-1.,-3.30385816281831));
#43488=CARTESIAN_POINT('Ctrl Pts',(2.19906078949924,-1.,-3.30848134694597));
#43489=CARTESIAN_POINT('Ctrl Pts',(2.20508863150608,-1.,-3.3130742460895));
#43490=CARTESIAN_POINT('Ctrl Pts',(2.21115211847872,-1.,-3.31764044024231));
#43491=CARTESIAN_POINT('Ctrl Pts',(2.21725135110889,-1.,-3.32218125618955));
#43492=CARTESIAN_POINT('Ctrl Pts',(2.22338548312758,-1.,-3.32669646722871));
#43493=CARTESIAN_POINT('Ctrl Pts',(2.22955308907221,-1.,-3.33118487773593));
#43494=CARTESIAN_POINT('Ctrl Pts',(2.23575256328809,-1.,-3.33564495756478));
#43495=CARTESIAN_POINT('Ctrl Pts',(2.24198249391437,-1.,-3.34007543738044));
#43496=CARTESIAN_POINT('Ctrl Pts',(2.24824207678287,-1.,-3.34447596770768));
#43497=CARTESIAN_POINT('Ctrl Pts',(2.25453097693524,-1.,-3.34884690292342));
#43498=CARTESIAN_POINT('Ctrl Pts',(2.26084915222484,-1.,-3.35318902552676));
#43499=CARTESIAN_POINT('Ctrl Pts',(2.26719668579921,-1.,-3.35750328523077));
#43500=CARTESIAN_POINT('Ctrl Pts',(2.27357362620902,-1.,-3.36179055004369));
#43501=CARTESIAN_POINT('Ctrl Pts',(2.27997979457968,-1.,-3.36605130712978));
#43502=CARTESIAN_POINT('Ctrl Pts',(2.28641481081045,-1.,-3.37028570206357));
#43503=CARTESIAN_POINT('Ctrl Pts',(2.2928781800731,-1.,-3.37449367172707));
#43504=CARTESIAN_POINT('Ctrl Pts',(2.29936936127588,-1.,-3.37867504959382));
#43505=CARTESIAN_POINT('Ctrl Pts',(2.30588783640389,-1.,-3.38282967336676));
#43506=CARTESIAN_POINT('Ctrl Pts',(2.31243319489505,-1.,-3.38695751492659));
#43507=CARTESIAN_POINT('Ctrl Pts',(2.31900513925627,-1.,-3.39105869475112));
#43508=CARTESIAN_POINT('Ctrl Pts',(2.32560343902683,-1.,-3.39513342020045));
#43509=CARTESIAN_POINT('Ctrl Pts',(2.33222789882601,-1.,-3.39918194578115));
#43510=CARTESIAN_POINT('Ctrl Pts',(2.33887832342715,-1.,-3.40320452776646));
#43511=CARTESIAN_POINT('Ctrl Pts',(2.34555447648901,-1.,-3.40720137403888));
#43512=CARTESIAN_POINT('Ctrl Pts',(2.35225606823649,-1.,-3.41117262313464));
#43513=CARTESIAN_POINT('Ctrl Pts',(2.35898278606449,-1.,-3.4151183675076));
#43514=CARTESIAN_POINT('Ctrl Pts',(2.36573431470313,-1.,-3.41903866635384));
#43515=CARTESIAN_POINT('Ctrl Pts',(2.37251035954351,-1.,-3.42293356216595));
#43516=CARTESIAN_POINT('Ctrl Pts',(2.37931067029517,-1.,-3.42680309755241));
#43517=CARTESIAN_POINT('Ctrl Pts',(2.38613505844641,-1.,-3.43064732714472));
#43518=CARTESIAN_POINT('Ctrl Pts',(2.39298338805823,-1.,-3.43446630680436));
#43519=CARTESIAN_POINT('Ctrl Pts',(2.39848113411428,-1.,-3.43750133066037));
#43520=CARTESIAN_POINT('Ctrl Pts',(2.40261515590099,-1.,-3.43976627485223));
#43521=CARTESIAN_POINT('Ctrl Pts',(2.40537592959345,-1.,-3.44127120683402));
#43522=CARTESIAN_POINT('Ctrl Pts',(2.40675750623143,-1.,-3.44202241512147));
#43523=CARTESIAN_POINT('',(2.52982887637028,-1.,-3.35260583073571));
#43524=CARTESIAN_POINT('',(2.40675750623143,-1.,-3.44202241512147));
#43525=CARTESIAN_POINT('',(2.36531447826073,-1.,-2.90994629141676));
#43526=CARTESIAN_POINT('Ctrl Pts',(2.52982887637028,-1.,-3.35260583073571));
#43527=CARTESIAN_POINT('Ctrl Pts',(2.5295413654909,-1.,-3.35105973714072));
#43528=CARTESIAN_POINT('Ctrl Pts',(2.52896321610703,-1.,-3.34796903576663));
#43529=CARTESIAN_POINT('Ctrl Pts',(2.52808660915689,-1.,-3.34333744115511));
#43530=CARTESIAN_POINT('Ctrl Pts',(2.52689902690158,-1.,-3.33717089999103));
#43531=CARTESIAN_POINT('Ctrl Pts',(2.52538321164634,-1.,-3.32947762187533));
#43532=CARTESIAN_POINT('Ctrl Pts',(2.5238359839626,-1.,-3.32179931078699));
#43533=CARTESIAN_POINT('Ctrl Pts',(2.52225724871313,-1.,-3.31413607874645));
#43534=CARTESIAN_POINT('Ctrl Pts',(2.52064689568511,-1.,-3.30648808815443));
#43535=CARTESIAN_POINT('Ctrl Pts',(2.51900480701068,-1.,-3.29885556388353));
#43536=CARTESIAN_POINT('Ctrl Pts',(2.51733085123797,-1.,-3.2912387729927));
#43537=CARTESIAN_POINT('Ctrl Pts',(2.51562487464514,-1.,-3.28363799702982));
#43538=CARTESIAN_POINT('Ctrl Pts',(2.513886692704,-1.,-3.27605350473142));
#43539=CARTESIAN_POINT('Ctrl Pts',(2.51211608411423,-1.,-3.26848552888116));
#43540=CARTESIAN_POINT('Ctrl Pts',(2.51031277813486,-1.,-3.26093423001434));
#43541=CARTESIAN_POINT('Ctrl Pts',(2.50847647070723,-1.,-3.25339971460982));
#43542=CARTESIAN_POINT('Ctrl Pts',(2.506606859405,-1.,-3.24588208983849));
#43543=CARTESIAN_POINT('Ctrl Pts',(2.5047036758003,-1.,-3.23838151080319));
#43544=CARTESIAN_POINT('Ctrl Pts',(2.50276671338111,-1.,-3.23089822320646));
#43545=CARTESIAN_POINT('Ctrl Pts',(2.50079587201957,-1.,-3.22343262620503));
#43546=CARTESIAN_POINT('Ctrl Pts',(2.4987911459939,-1.,-3.21598526261286));
#43547=CARTESIAN_POINT('Ctrl Pts',(2.4967525264737,-1.,-3.20855669849836));
#43548=CARTESIAN_POINT('Ctrl Pts',(2.49467992057755,-1.,-3.20114742397588));
#43549=CARTESIAN_POINT('Ctrl Pts',(2.49257307239848,-1.,-3.19375775555798));
#43550=CARTESIAN_POINT('Ctrl Pts',(2.49043146334059,-1.,-3.18638771282266));
#43551=CARTESIAN_POINT('Ctrl Pts',(2.48825428288201,-1.,-3.17903698136622));
#43552=CARTESIAN_POINT('Ctrl Pts',(2.48604065348587,-1.,-3.17170518863313));
#43553=CARTESIAN_POINT('Ctrl Pts',(2.48378981792725,-1.,-3.16439213290161));
#43554=CARTESIAN_POINT('Ctrl Pts',(2.48150133566571,-1.,-3.15709802322739));
#43555=CARTESIAN_POINT('Ctrl Pts',(2.47917529057029,-1.,-3.14982373241352));
#43556=CARTESIAN_POINT('Ctrl Pts',(2.47681245356109,-1.,-3.1425709954655));
#43557=CARTESIAN_POINT('Ctrl Pts',(2.47441378371932,-1.,-3.13534181229295));
#43558=CARTESIAN_POINT('Ctrl Pts',(2.47197997765871,-1.,-3.12813790805952));
#43559=CARTESIAN_POINT('Ctrl Pts',(2.46951098947469,-1.,-3.12096015766983));
#43560=CARTESIAN_POINT('Ctrl Pts',(2.46700558843506,-1.,-3.11380805536122));
#43561=CARTESIAN_POINT('Ctrl Pts',(2.46446082979646,-1.,-3.1066790790198));
#43562=CARTESIAN_POINT('Ctrl Pts',(2.46187308501884,-1.,-3.09956993697052));
#43563=CARTESIAN_POINT('Ctrl Pts',(2.4592391256388,-1.,-3.09247787931887));
#43564=CARTESIAN_POINT('Ctrl Pts',(2.45655725437039,-1.,-3.08540206545315));
#43565=CARTESIAN_POINT('Ctrl Pts',(2.4538282678779,-1.,-3.07834472886139));
#43566=CARTESIAN_POINT('Ctrl Pts',(2.45105688854422,-1.,-3.07131290521297));
#43567=CARTESIAN_POINT('Ctrl Pts',(2.44824970516543,-1.,-3.06431596421405));
#43568=CARTESIAN_POINT('Ctrl Pts',(2.44541251892556,-1.,-3.05736242671506));
#43569=CARTESIAN_POINT('Ctrl Pts',(2.44254768923105,-1.,-3.05045678021504));
#43570=CARTESIAN_POINT('Ctrl Pts',(2.43965194061857,-1.,-3.04359685040555));
#43571=CARTESIAN_POINT('Ctrl Pts',(2.43671278042414,-1.,-3.03676949672822));
#43572=CARTESIAN_POINT('Ctrl Pts',(2.43371241361488,-1.,-3.02995534946978));
#43573=CARTESIAN_POINT('Ctrl Pts',(2.43063415586637,-1.,-3.02313656036004));
#43574=CARTESIAN_POINT('Ctrl Pts',(2.42746856264168,-1.,-3.01630420830504));
#43575=CARTESIAN_POINT('Ctrl Pts',(2.42421849439613,-1.,-3.00946442616659));
#43576=CARTESIAN_POINT('Ctrl Pts',(2.42090763946779,-1.,-3.00264868585996));
#43577=CARTESIAN_POINT('Ctrl Pts',(2.41757324500514,-1.,-2.99590509293503));
#43578=CARTESIAN_POINT('Ctrl Pts',(2.41425064199586,-1.,-2.98927983005796));
#43579=CARTESIAN_POINT('Ctrl Pts',(2.41095909342571,-1.,-2.98280015815107));
#43580=CARTESIAN_POINT('Ctrl Pts',(2.40768975073713,-1.,-2.97646002822422));
#43581=CARTESIAN_POINT('Ctrl Pts',(2.40438604734919,-1.,-2.9701964131236));
#43582=CARTESIAN_POINT('Ctrl Pts',(2.4009556571164,-1.,-2.96390432240312));
#43583=CARTESIAN_POINT('Ctrl Pts',(2.39730553974516,-1.,-2.95748006482942));
#43584=CARTESIAN_POINT('Ctrl Pts',(2.39337207631667,-1.,-2.95085857128439));
#43585=CARTESIAN_POINT('Ctrl Pts',(2.38914929090759,-1.,-2.94404820669076));
#43586=CARTESIAN_POINT('Ctrl Pts',(2.38472771516311,-1.,-2.93717903280391));
#43587=CARTESIAN_POINT('Ctrl Pts',(2.38028989582073,-1.,-2.93049643640206));
#43588=CARTESIAN_POINT('Ctrl Pts',(2.3760651052403,-1.,-2.92430340582608));
#43589=CARTESIAN_POINT('Ctrl Pts',(2.37229381109821,-1.,-2.91891503791411));
#43590=CARTESIAN_POINT('Ctrl Pts',(2.36919161373173,-1.,-2.9146124988314));
#43591=CARTESIAN_POINT('Ctrl Pts',(2.36707658451664,-1.,-2.91181344022549));
#43592=CARTESIAN_POINT('Ctrl Pts',(2.36599991765749,-1.,-2.91051690822156));
#43593=CARTESIAN_POINT('Ctrl Pts',(2.36553202948613,-1.,-2.91005770527719));
#43594=CARTESIAN_POINT('Ctrl Pts',(2.36536211188453,-1.,-2.90995756655606));
#43595=CARTESIAN_POINT('Ctrl Pts',(2.36531447826073,-1.,-2.90994629141676));
#43596=CARTESIAN_POINT('',(2.50410331873042,-1.,-2.79140942341378));
#43597=CARTESIAN_POINT('Origin',(0.,-1.,0.));
#43598=CARTESIAN_POINT('',(2.91557726271063,-1.,-3.02314558451372));
#43599=CARTESIAN_POINT('Ctrl Pts',(2.50410331873042,-1.,-2.79140942341378));
#43600=CARTESIAN_POINT('Ctrl Pts',(2.50410700351426,-1.,-2.79145823440899));
#43601=CARTESIAN_POINT('Ctrl Pts',(2.50417932839343,-1.,-2.79164172519039));
#43602=CARTESIAN_POINT('Ctrl Pts',(2.50455968395235,-1.,-2.79217568804874));
#43603=CARTESIAN_POINT('Ctrl Pts',(2.50567182569153,-1.,-2.79344192164204));
#43604=CARTESIAN_POINT('Ctrl Pts',(2.50810555977564,-1.,-2.7959687805717));
#43605=CARTESIAN_POINT('Ctrl Pts',(2.51186983687947,-1.,-2.79970585014308));
#43606=CARTESIAN_POINT('Ctrl Pts',(2.51660190466067,-1.,-2.80427363984939));
#43607=CARTESIAN_POINT('Ctrl Pts',(2.52205778589922,-1.,-2.80941521967234));
#43608=CARTESIAN_POINT('Ctrl Pts',(2.52796388055457,-1.,-2.8148437904867));
#43609=CARTESIAN_POINT('Ctrl Pts',(2.53405679667463,-1.,-2.82028550483744));
#43610=CARTESIAN_POINT('Ctrl Pts',(2.54012272520141,-1.,-2.82552167649157));
#43611=CARTESIAN_POINT('Ctrl Pts',(2.54604736792542,-1.,-2.83044254225794));
#43612=CARTESIAN_POINT('Ctrl Pts',(2.55182152806964,-1.,-2.83505269592412));
#43613=CARTESIAN_POINT('Ctrl Pts',(2.55749952145165,-1.,-2.83942515220699));
#43614=CARTESIAN_POINT('Ctrl Pts',(2.56316920798489,-1.,-2.84366802680211));
#43615=CARTESIAN_POINT('Ctrl Pts',(2.56891984251743,-1.,-2.84788893329091));
#43616=CARTESIAN_POINT('Ctrl Pts',(2.57480482727128,-1.,-2.85215360144483));
#43617=CARTESIAN_POINT('Ctrl Pts',(2.58082875254407,-1.,-2.85647171715147));
#43618=CARTESIAN_POINT('Ctrl Pts',(2.5869677064356,-1.,-2.86081999003668));
#43619=CARTESIAN_POINT('Ctrl Pts',(2.59318160184921,-1.,-2.86515629953528));
#43620=CARTESIAN_POINT('Ctrl Pts',(2.59942875223202,-1.,-2.86943633170712));
#43621=CARTESIAN_POINT('Ctrl Pts',(2.6056817788128,-1.,-2.87363176656475));
#43622=CARTESIAN_POINT('Ctrl Pts',(2.61193507170928,-1.,-2.87773881947885));
#43623=CARTESIAN_POINT('Ctrl Pts',(2.61819596473087,-1.,-2.88176821427502));
#43624=CARTESIAN_POINT('Ctrl Pts',(2.62447947640253,-1.,-2.88573922195049));
#43625=CARTESIAN_POINT('Ctrl Pts',(2.63080195420771,-1.,-2.88967244854243));
#43626=CARTESIAN_POINT('Ctrl Pts',(2.63717442263944,-1.,-2.89358228854557));
#43627=CARTESIAN_POINT('Ctrl Pts',(2.64359851684146,-1.,-2.89747231723361));
#43628=CARTESIAN_POINT('Ctrl Pts',(2.65007017365576,-1.,-2.90133950224879));
#43629=CARTESIAN_POINT('Ctrl Pts',(2.65658188464287,-1.,-2.90517678087467));
#43630=CARTESIAN_POINT('Ctrl Pts',(2.66312542616808,-1.,-2.90897617968921));
#43631=CARTESIAN_POINT('Ctrl Pts',(2.66969458792627,-1.,-2.91273193382876));
#43632=CARTESIAN_POINT('Ctrl Pts',(2.67628728855309,-1.,-2.91644290704281));
#43633=CARTESIAN_POINT('Ctrl Pts',(2.68290409279689,-1.,-2.92011090722152));
#43634=CARTESIAN_POINT('Ctrl Pts',(2.68954721165342,-1.,-2.92373955325876));
#43635=CARTESIAN_POINT('Ctrl Pts',(2.69621932864302,-1.,-2.92733294395268));
#43636=CARTESIAN_POINT('Ctrl Pts',(2.70292247416881,-1.,-2.93089438233746));
#43637=CARTESIAN_POINT('Ctrl Pts',(2.70965695523776,-1.,-2.93442516311168));
#43638=CARTESIAN_POINT('Ctrl Pts',(2.71642190053575,-1.,-2.93792519474955));
#43639=CARTESIAN_POINT('Ctrl Pts',(2.72321571511322,-1.,-2.94139351933882));
#43640=CARTESIAN_POINT('Ctrl Pts',(2.73003657371613,-1.,-2.94482887675139));
#43641=CARTESIAN_POINT('Ctrl Pts',(2.73688288329825,-1.,-2.94823023414381));
#43642=CARTESIAN_POINT('Ctrl Pts',(2.7437537949221,-1.,-2.95159737214305));
#43643=CARTESIAN_POINT('Ctrl Pts',(2.75064903318996,-1.,-2.95493069316211));
#43644=CARTESIAN_POINT('Ctrl Pts',(2.75756867888393,-1.,-2.9582309766594));
#43645=CARTESIAN_POINT('Ctrl Pts',(2.76451296269571,-1.,-2.96149914764832));
#43646=CARTESIAN_POINT('Ctrl Pts',(2.77148206836464,-1.,-2.96473605585548));
#43647=CARTESIAN_POINT('Ctrl Pts',(2.77847589542767,-1.,-2.9679422104295));
#43648=CARTESIAN_POINT('Ctrl Pts',(2.78549409123657,-1.,-2.97111781461349));
#43649=CARTESIAN_POINT('Ctrl Pts',(2.79253615718147,-1.,-2.97426288347475));
#43650=CARTESIAN_POINT('Ctrl Pts',(2.79960153278186,-1.,-2.97737733718242));
#43651=CARTESIAN_POINT('Ctrl Pts',(2.80668968101162,-1.,-2.98046109647299));
#43652=CARTESIAN_POINT('Ctrl Pts',(2.81380019196454,-1.,-2.9835141977994));
#43653=CARTESIAN_POINT('Ctrl Pts',(2.82093279065704,-1.,-2.98653680669434));
#43654=CARTESIAN_POINT('Ctrl Pts',(2.82808728190402,-1.,-2.98952916401699));
#43655=CARTESIAN_POINT('Ctrl Pts',(2.83526351254383,-1.,-2.99249155170479));
#43656=CARTESIAN_POINT('Ctrl Pts',(2.84246132984334,-1.,-2.995424253416));
#43657=CARTESIAN_POINT('Ctrl Pts',(2.84968053289104,-1.,-2.99832751144566));
#43658=CARTESIAN_POINT('Ctrl Pts',(2.85692085715129,-1.,-3.0012015079552));
#43659=CARTESIAN_POINT('Ctrl Pts',(2.86418200833065,-1.,-3.00404638316245));
#43660=CARTESIAN_POINT('Ctrl Pts',(2.87146368430104,-1.,-3.00686224485374));
#43661=CARTESIAN_POINT('Ctrl Pts',(2.87876560072799,-1.,-3.0096491810855));
#43662=CARTESIAN_POINT('Ctrl Pts',(2.88608751706796,-1.,-3.01240727309568));
#43663=CARTESIAN_POINT('Ctrl Pts',(2.8934292556764,-1.,-3.01513660433291));
#43664=CARTESIAN_POINT('Ctrl Pts',(2.90079069102661,-1.,-3.01783725123646));
#43665=CARTESIAN_POINT('Ctrl Pts',(2.90669553303902,-1.,-3.01997487194926));
#43666=CARTESIAN_POINT('Ctrl Pts',(2.91113297349052,-1.,-3.02156522743299));
#43667=CARTESIAN_POINT('Ctrl Pts',(2.91409518070707,-1.,-3.02261975104912));
#43668=CARTESIAN_POINT('Ctrl Pts',(2.91557726271063,-1.,-3.02314558451372));
#43669=CARTESIAN_POINT('',(3.02314558451372,-1.,-2.91557726271063));
#43670=CARTESIAN_POINT('',(2.91557726271063,-1.,-3.02314558451372));
#43671=CARTESIAN_POINT('',(2.79140942341258,-1.,-2.50410331873176));
#43672=CARTESIAN_POINT('Ctrl Pts',(3.02314558451372,-1.,-2.91557726271063));
#43673=CARTESIAN_POINT('Ctrl Pts',(3.02261975104593,-1.,-2.91409518070399));
#43674=CARTESIAN_POINT('Ctrl Pts',(3.02156522742431,-1.,-2.91113297348212));
#43675=CARTESIAN_POINT('Ctrl Pts',(3.01997487193503,-1.,-2.90669553302526));
#43676=CARTESIAN_POINT('Ctrl Pts',(3.01783725121981,-1.,-2.9007906910105));
#43677=CARTESIAN_POINT('Ctrl Pts',(3.01513660431928,-1.,-2.89342925566321));
#43678=CARTESIAN_POINT('Ctrl Pts',(3.01240727308829,-1.,-2.8860875170608));
#43679=CARTESIAN_POINT('Ctrl Pts',(3.00964918108476,-1.,-2.87876560072727));
#43680=CARTESIAN_POINT('Ctrl Pts',(3.00686224485784,-1.,-2.87146368430502));
#43681=CARTESIAN_POINT('Ctrl Pts',(3.00404638316867,-1.,-2.86418200833667));
#43682=CARTESIAN_POINT('Ctrl Pts',(3.00120150796095,-1.,-2.85692085715686));
#43683=CARTESIAN_POINT('Ctrl Pts',(2.99832751144925,-1.,-2.84968053289451));
#43684=CARTESIAN_POINT('Ctrl Pts',(2.99542425341685,-1.,-2.84246132984415));
#43685=CARTESIAN_POINT('Ctrl Pts',(2.99249155170339,-1.,-2.83526351254248));
#43686=CARTESIAN_POINT('Ctrl Pts',(2.98952916401446,-1.,-2.82808728190157));
#43687=CARTESIAN_POINT('Ctrl Pts',(2.9865368066918,-1.,-2.82093279065457));
#43688=CARTESIAN_POINT('Ctrl Pts',(2.98351419779767,-1.,-2.81380019196286));
#43689=CARTESIAN_POINT('Ctrl Pts',(2.98046109647241,-1.,-2.80668968101106));
#43690=CARTESIAN_POINT('Ctrl Pts',(2.97737733718287,-1.,-2.7996015327823));
#43691=CARTESIAN_POINT('Ctrl Pts',(2.9742628834758,-1.,-2.79253615718248));
#43692=CARTESIAN_POINT('Ctrl Pts',(2.97111781461465,-1.,-2.78549409123769));
#43693=CARTESIAN_POINT('Ctrl Pts',(2.96794221043036,-1.,-2.7784758954285));
#43694=CARTESIAN_POINT('Ctrl Pts',(2.96473605585583,-1.,-2.77148206836498));
#43695=CARTESIAN_POINT('Ctrl Pts',(2.96149914764818,-1.,-2.76451296269557));
#43696=CARTESIAN_POINT('Ctrl Pts',(2.95823097665896,-1.,-2.7575686788835));
#43697=CARTESIAN_POINT('Ctrl Pts',(2.95493069316161,-1.,-2.75064903318947));
#43698=CARTESIAN_POINT('Ctrl Pts',(2.95159737214266,-1.,-2.74375379492172));
#43699=CARTESIAN_POINT('Ctrl Pts',(2.94823023414364,-1.,-2.73688288329808));
#43700=CARTESIAN_POINT('Ctrl Pts',(2.94482887675143,-1.,-2.73003657371617));
#43701=CARTESIAN_POINT('Ctrl Pts',(2.94139351933897,-1.,-2.72321571511337));
#43702=CARTESIAN_POINT('Ctrl Pts',(2.93792519474972,-1.,-2.71642190053592));
#43703=CARTESIAN_POINT('Ctrl Pts',(2.93442516311179,-1.,-2.70965695523787));
#43704=CARTESIAN_POINT('Ctrl Pts',(2.93089438233749,-1.,-2.70292247416885));
#43705=CARTESIAN_POINT('Ctrl Pts',(2.92733294395267,-1.,-2.69621932864301));
#43706=CARTESIAN_POINT('Ctrl Pts',(2.92373955325875,-1.,-2.68954721165339));
#43707=CARTESIAN_POINT('Ctrl Pts',(2.92011090722152,-1.,-2.68290409279688));
#43708=CARTESIAN_POINT('Ctrl Pts',(2.91644290704285,-1.,-2.67628728855312));
#43709=CARTESIAN_POINT('Ctrl Pts',(2.91273193382882,-1.,-2.66969458792631));
#43710=CARTESIAN_POINT('Ctrl Pts',(2.90897617968923,-1.,-2.6631254261681));
#43711=CARTESIAN_POINT('Ctrl Pts',(2.90517678087461,-1.,-2.65658188464282));
#43712=CARTESIAN_POINT('Ctrl Pts',(2.90133950224867,-1.,-2.65007017365564));
#43713=CARTESIAN_POINT('Ctrl Pts',(2.89747231723345,-1.,-2.64359851684131));
#43714=CARTESIAN_POINT('Ctrl Pts',(2.89358228854544,-1.,-2.63717442263932));
#43715=CARTESIAN_POINT('Ctrl Pts',(2.88967244854239,-1.,-2.63080195420767));
#43716=CARTESIAN_POINT('Ctrl Pts',(2.88573922195059,-1.,-2.62447947640262));
#43717=CARTESIAN_POINT('Ctrl Pts',(2.88176821427525,-1.,-2.61819596473108));
#43718=CARTESIAN_POINT('Ctrl Pts',(2.87773881947915,-1.,-2.61193507170955));
#43719=CARTESIAN_POINT('Ctrl Pts',(2.87363176656501,-1.,-2.60568177881303));
#43720=CARTESIAN_POINT('Ctrl Pts',(2.86943633170722,-1.,-2.5994287522321));
#43721=CARTESIAN_POINT('Ctrl Pts',(2.86515629953513,-1.,-2.59318160184908));
#43722=CARTESIAN_POINT('Ctrl Pts',(2.86081999003629,-1.,-2.58696770643524));
#43723=CARTESIAN_POINT('Ctrl Pts',(2.85647171715092,-1.,-2.58082875254357));
#43724=CARTESIAN_POINT('Ctrl Pts',(2.85215360144431,-1.,-2.57480482727081));
#43725=CARTESIAN_POINT('Ctrl Pts',(2.84788893329067,-1.,-2.56891984251721));
#43726=CARTESIAN_POINT('Ctrl Pts',(2.84366802680237,-1.,-2.56316920798513));
#43727=CARTESIAN_POINT('Ctrl Pts',(2.83942515220782,-1.,-2.55749952145241));
#43728=CARTESIAN_POINT('Ctrl Pts',(2.83505269592536,-1.,-2.55182152807077));
#43729=CARTESIAN_POINT('Ctrl Pts',(2.83044254225917,-1.,-2.54604736792655));
#43730=CARTESIAN_POINT('Ctrl Pts',(2.8255216764922,-1.,-2.54012272520199));
#43731=CARTESIAN_POINT('Ctrl Pts',(2.82028550483689,-1.,-2.53405679667412));
#43732=CARTESIAN_POINT('Ctrl Pts',(2.81484379048475,-1.,-2.52796388055278));
#43733=CARTESIAN_POINT('Ctrl Pts',(2.80941521966941,-1.,-2.52205778589653));
#43734=CARTESIAN_POINT('Ctrl Pts',(2.80427363984653,-1.,-2.51660190465805));
#43735=CARTESIAN_POINT('Ctrl Pts',(2.79970585014168,-1.,-2.51186983687818));
#43736=CARTESIAN_POINT('Ctrl Pts',(2.79596878057287,-1.,-2.50810555977671));
#43737=CARTESIAN_POINT('Ctrl Pts',(2.79344192164147,-1.,-2.50567182569081));
#43738=CARTESIAN_POINT('Ctrl Pts',(2.79217568804755,-1.,-2.50455968395146));
#43739=CARTESIAN_POINT('Ctrl Pts',(2.79164172518905,-1.,-2.50417932839313));
#43740=CARTESIAN_POINT('Ctrl Pts',(2.79145823440781,-1.,-2.50410700351493));
#43741=CARTESIAN_POINT('Ctrl Pts',(2.79140942341258,-1.,-2.50410331873176));
#43742=CARTESIAN_POINT('',(2.90994629141562,-1.,-2.36531447826213));
#43743=CARTESIAN_POINT('Origin',(0.,-1.,0.));
#43744=CARTESIAN_POINT('',(3.35260583073571,-1.,-2.52982887637028));
#43745=CARTESIAN_POINT('Ctrl Pts',(2.90994629141562,-1.,-2.36531447826213));
#43746=CARTESIAN_POINT('Ctrl Pts',(2.90995756655558,-1.,-2.3653621118858));
#43747=CARTESIAN_POINT('Ctrl Pts',(2.9100577052777,-1.,-2.36553202948741));
#43748=CARTESIAN_POINT('Ctrl Pts',(2.91051690822262,-1.,-2.36599991765853));
#43749=CARTESIAN_POINT('Ctrl Pts',(2.91181344022628,-1.,-2.36707658451709));
#43750=CARTESIAN_POINT('Ctrl Pts',(2.91461249883016,-1.,-2.36919161373074));
#43751=CARTESIAN_POINT('Ctrl Pts',(2.9189150379156,-1.,-2.37229381109939));
#43752=CARTESIAN_POINT('Ctrl Pts',(2.92430340582912,-1.,-2.37606510524271));
#43753=CARTESIAN_POINT('Ctrl Pts',(2.93049643640517,-1.,-2.3802898958232));
#43754=CARTESIAN_POINT('Ctrl Pts',(2.93717903280599,-1.,-2.38472771516476));
#43755=CARTESIAN_POINT('Ctrl Pts',(2.94404820669135,-1.,-2.38914929090806));
#43756=CARTESIAN_POINT('Ctrl Pts',(2.95085857128372,-1.,-2.39337207631613));
#43757=CARTESIAN_POINT('Ctrl Pts',(2.95748006482811,-1.,-2.39730553974412));
#43758=CARTESIAN_POINT('Ctrl Pts',(2.9639043224018,-1.,-2.40095565711535));
#43759=CARTESIAN_POINT('Ctrl Pts',(2.97019641312272,-1.,-2.40438604734848));
#43760=CARTESIAN_POINT('Ctrl Pts',(2.97646002822395,-1.,-2.40768975073691));
#43761=CARTESIAN_POINT('Ctrl Pts',(2.98280015815132,-1.,-2.41095909342591));
#43762=CARTESIAN_POINT('Ctrl Pts',(2.98927983005851,-1.,-2.4142506419963));
#43763=CARTESIAN_POINT('Ctrl Pts',(2.99590509293561,-1.,-2.4175732450056));
#43764=CARTESIAN_POINT('Ctrl Pts',(3.00264868586038,-1.,-2.42090763946812));
#43765=CARTESIAN_POINT('Ctrl Pts',(3.00946442616674,-1.,-2.42421849439625));
#43766=CARTESIAN_POINT('Ctrl Pts',(3.01630420830493,-1.,-2.4274685626416));
#43767=CARTESIAN_POINT('Ctrl Pts',(3.02313656035977,-1.,-2.43063415586615));
#43768=CARTESIAN_POINT('Ctrl Pts',(3.02995534946946,-1.,-2.43371241361462));
#43769=CARTESIAN_POINT('Ctrl Pts',(3.03676949672797,-1.,-2.43671278042394));
#43770=CARTESIAN_POINT('Ctrl Pts',(3.04359685040545,-1.,-2.43965194061849));
#43771=CARTESIAN_POINT('Ctrl Pts',(3.05045678021509,-1.,-2.44254768923109));
#43772=CARTESIAN_POINT('Ctrl Pts',(3.05736242671521,-1.,-2.44541251892568));
#43773=CARTESIAN_POINT('Ctrl Pts',(3.06431596421422,-1.,-2.44824970516558));
#43774=CARTESIAN_POINT('Ctrl Pts',(3.0713129052131,-1.,-2.45105688854432));
#43775=CARTESIAN_POINT('Ctrl Pts',(3.07834472886145,-1.,-2.45382826787795));
#43776=CARTESIAN_POINT('Ctrl Pts',(3.08540206545313,-1.,-2.45655725437037));
#43777=CARTESIAN_POINT('Ctrl Pts',(3.09247787931881,-1.,-2.45923912563875));
#43778=CARTESIAN_POINT('Ctrl Pts',(3.09956993697048,-1.,-2.4618730850188));
#43779=CARTESIAN_POINT('Ctrl Pts',(3.10667907901981,-1.,-2.46446082979645));
#43780=CARTESIAN_POINT('Ctrl Pts',(3.11380805536124,-1.,-2.46700558843507));
#43781=CARTESIAN_POINT('Ctrl Pts',(3.12096015766984,-1.,-2.4695109894747));
#43782=CARTESIAN_POINT('Ctrl Pts',(3.12813790805948,-1.,-2.47197997765868));
#43783=CARTESIAN_POINT('Ctrl Pts',(3.13534181229282,-1.,-2.47441378371923));
#43784=CARTESIAN_POINT('Ctrl Pts',(3.14257099546531,-1.,-2.47681245356095));
#43785=CARTESIAN_POINT('Ctrl Pts',(3.14982373241335,-1.,-2.47917529057016));
#43786=CARTESIAN_POINT('Ctrl Pts',(3.15709802322735,-1.,-2.48150133566568));
#43787=CARTESIAN_POINT('Ctrl Pts',(3.16439213290181,-1.,-2.48378981792739));
#43788=CARTESIAN_POINT('Ctrl Pts',(3.17170518863357,-1.,-2.48604065348619));
#43789=CARTESIAN_POINT('Ctrl Pts',(3.17903698136678,-1.,-2.48825428288243));
#43790=CARTESIAN_POINT('Ctrl Pts',(3.18638771282315,-1.,-2.49043146334095));
#43791=CARTESIAN_POINT('Ctrl Pts',(3.19375775555814,-1.,-2.4925730723986));
#43792=CARTESIAN_POINT('Ctrl Pts',(3.20114742397549,-1.,-2.49467992057726));
#43793=CARTESIAN_POINT('Ctrl Pts',(3.2085566984974,-1.,-2.49675252647298));
#43794=CARTESIAN_POINT('Ctrl Pts',(3.21598526261157,-1.,-2.49879114599293));
#43795=CARTESIAN_POINT('Ctrl Pts',(3.22343262620387,-1.,-2.5007958720187));
#43796=CARTESIAN_POINT('Ctrl Pts',(3.23089822320596,-1.,-2.50276671338074));
#43797=CARTESIAN_POINT('Ctrl Pts',(3.23838151080383,-1.,-2.50470367580078));
#43798=CARTESIAN_POINT('Ctrl Pts',(3.24588208984042,-1.,-2.50660685940645));
#43799=CARTESIAN_POINT('Ctrl Pts',(3.25339971461265,-1.,-2.50847647070936));
#43800=CARTESIAN_POINT('Ctrl Pts',(3.26093423001716,-1.,-2.51031277813697));
#43801=CARTESIAN_POINT('Ctrl Pts',(3.26848552888271,-1.,-2.51211608411539));
#43802=CARTESIAN_POINT('Ctrl Pts',(3.27605350473048,-1.,-2.51388669270329));
#43803=CARTESIAN_POINT('Ctrl Pts',(3.28363799702583,-1.,-2.51562487464215));
#43804=CARTESIAN_POINT('Ctrl Pts',(3.2912387729863,-1.,-2.51733085123316));
#43805=CARTESIAN_POINT('Ctrl Pts',(3.29885556387661,-1.,-2.51900480700548));
#43806=CARTESIAN_POINT('Ctrl Pts',(3.30648808814986,-1.,-2.52064689568167));
#43807=CARTESIAN_POINT('Ctrl Pts',(3.31413607874727,-1.,-2.52225724871375));
#43808=CARTESIAN_POINT('Ctrl Pts',(3.32179931079521,-1.,-2.52383598396878));
#43809=CARTESIAN_POINT('Ctrl Pts',(3.32947762189049,-1.,-2.52538321165774));
#43810=CARTESIAN_POINT('Ctrl Pts',(3.33717090000955,-1.,-2.52689902691551));
#43811=CARTESIAN_POINT('Ctrl Pts',(3.34333744117093,-1.,-2.52808660916879));
#43812=CARTESIAN_POINT('Ctrl Pts',(3.34796903577628,-1.,-2.5289632161143));
#43813=CARTESIAN_POINT('Ctrl Pts',(3.35105973714426,-1.,-2.52954136549357));
#43814=CARTESIAN_POINT('Ctrl Pts',(3.35260583073571,-1.,-2.52982887637028));
#43815=CARTESIAN_POINT('',(3.44202241512147,-1.,-2.40675750623143));
#43816=CARTESIAN_POINT('',(3.35260583073571,-1.,-2.52982887637028));
#43817=CARTESIAN_POINT('',(3.14877060440327,-1.,-2.03660101169714));
#43818=CARTESIAN_POINT('Ctrl Pts',(3.44202241512147,-1.,-2.40675750623143));
#43819=CARTESIAN_POINT('Ctrl Pts',(3.44127120683039,-1.,-2.4053759295909));
#43820=CARTESIAN_POINT('Ctrl Pts',(3.43976627484234,-1.,-2.40261515589405));
#43821=CARTESIAN_POINT('Ctrl Pts',(3.43750133064416,-1.,-2.39848113410292));
#43822=CARTESIAN_POINT('Ctrl Pts',(3.4344663067854,-1.,-2.39298338804493));
#43823=CARTESIAN_POINT('Ctrl Pts',(3.43064732712919,-1.,-2.38613505843552));
#43824=CARTESIAN_POINT('Ctrl Pts',(3.42680309754399,-1.,-2.37931067028926));
#43825=CARTESIAN_POINT('Ctrl Pts',(3.42293356216511,-1.,-2.37251035954292));
#43826=CARTESIAN_POINT('Ctrl Pts',(3.41903866635852,-1.,-2.36573431470642));
#43827=CARTESIAN_POINT('Ctrl Pts',(3.41511836751469,-1.,-2.35898278606946));
#43828=CARTESIAN_POINT('Ctrl Pts',(3.41117262314119,-1.,-2.35225606824109));
#43829=CARTESIAN_POINT('Ctrl Pts',(3.40720137404297,-1.,-2.34555447649188));
#43830=CARTESIAN_POINT('Ctrl Pts',(3.40320452776743,-1.,-2.33887832342782));
#43831=CARTESIAN_POINT('Ctrl Pts',(3.39918194577956,-1.,-2.33222789882489));
#43832=CARTESIAN_POINT('Ctrl Pts',(3.39513342019756,-1.,-2.3256034390248));
#43833=CARTESIAN_POINT('Ctrl Pts',(3.39105869474822,-1.,-2.31900513925424));
#43834=CARTESIAN_POINT('Ctrl Pts',(3.38695751492462,-1.,-2.31243319489367));
#43835=CARTESIAN_POINT('Ctrl Pts',(3.3828296733661,-1.,-2.30588783640343));
#43836=CARTESIAN_POINT('Ctrl Pts',(3.37867504959433,-1.,-2.29936936127624));
#43837=CARTESIAN_POINT('Ctrl Pts',(3.37449367172826,-1.,-2.29287818007393));
#43838=CARTESIAN_POINT('Ctrl Pts',(3.37028570206488,-1.,-2.28641481081137));
#43839=CARTESIAN_POINT('Ctrl Pts',(3.36605130713076,-1.,-2.27997979458037));
#43840=CARTESIAN_POINT('Ctrl Pts',(3.36179055004409,-1.,-2.2735736262093));
#43841=CARTESIAN_POINT('Ctrl Pts',(3.35750328523061,-1.,-2.2671966857991));
#43842=CARTESIAN_POINT('Ctrl Pts',(3.35318902552626,-1.,-2.26084915222449));
#43843=CARTESIAN_POINT('Ctrl Pts',(3.34884690292285,-1.,-2.25453097693483));
#43844=CARTESIAN_POINT('Ctrl Pts',(3.34447596770723,-1.,-2.24824207678256));
#43845=CARTESIAN_POINT('Ctrl Pts',(3.34007543738025,-1.,-2.24198249391422));
#43846=CARTESIAN_POINT('Ctrl Pts',(3.33564495756481,-1.,-2.23575256328812));
#43847=CARTESIAN_POINT('Ctrl Pts',(3.33118487773611,-1.,-2.22955308907233));
#43848=CARTESIAN_POINT('Ctrl Pts',(3.3266964672289,-1.,-2.22338548312772));
#43849=CARTESIAN_POINT('Ctrl Pts',(3.32218125618968,-1.,-2.21725135110898));
#43850=CARTESIAN_POINT('Ctrl Pts',(3.31764044024235,-1.,-2.21115211847875));
#43851=CARTESIAN_POINT('Ctrl Pts',(3.31307424608949,-1.,-2.20508863150607));
#43852=CARTESIAN_POINT('Ctrl Pts',(3.30848134694595,-1.,-2.19906078949923));
#43853=CARTESIAN_POINT('Ctrl Pts',(3.30385816281831,-1.,-2.19306710376111));
#43854=CARTESIAN_POINT('Ctrl Pts',(3.29920022557639,-1.,-2.18710556500327));
#43855=CARTESIAN_POINT('Ctrl Pts',(3.2945036150049,-1.,-2.18117455557065));
#43856=CARTESIAN_POINT('Ctrl Pts',(3.28976645712568,-1.,-2.17527380048423));
#43857=CARTESIAN_POINT('Ctrl Pts',(3.28499019979724,-1.,-2.16940517773455));
#43858=CARTESIAN_POINT('Ctrl Pts',(3.280181508414,-1.,-2.16357391934425));
#43859=CARTESIAN_POINT('Ctrl Pts',(3.27534954469187,-1.,-2.15778690038347));
#43860=CARTESIAN_POINT('Ctrl Pts',(3.27050245897228,-1.,-2.15205043199808));
#43861=CARTESIAN_POINT('Ctrl Pts',(3.26564388189759,-1.,-2.1463680529566));
#43862=CARTESIAN_POINT('Ctrl Pts',(3.26077002641879,-1.,-2.14073870754264));
#43863=CARTESIAN_POINT('Ctrl Pts',(3.25586495065054,-1.,-2.13515375878803));
#43864=CARTESIAN_POINT('Ctrl Pts',(3.25090574494028,-1.,-2.12960028396832));
#43865=CARTESIAN_POINT('Ctrl Pts',(3.24587102613376,-1.,-2.12406646410962));
#43866=CARTESIAN_POINT('Ctrl Pts',(3.24074905517293,-1.,-2.11854673326979));
#43867=CARTESIAN_POINT('Ctrl Pts',(3.23554444767099,-1.,-2.11304604021773));
#43868=CARTESIAN_POINT('Ctrl Pts',(3.23028945793289,-1.,-2.10758699642451));
#43869=CARTESIAN_POINT('Ctrl Pts',(3.22503437553434,-1.,-2.10220384298492));
#43870=CARTESIAN_POINT('Ctrl Pts',(3.21982707347009,-1.,-2.09692958434895));
#43871=CARTESIAN_POINT('Ctrl Pts',(3.21469429601654,-1.,-2.09178419460443));
#43872=CARTESIAN_POINT('Ctrl Pts',(3.20962575845463,-1.,-2.08676465517455));
#43873=CARTESIAN_POINT('Ctrl Pts',(3.2045481863073,-1.,-2.08182850370878));
#43874=CARTESIAN_POINT('Ctrl Pts',(3.19934132836019,-1.,-2.07690441870722));
#43875=CARTESIAN_POINT('Ctrl Pts',(3.19388465568252,-1.,-2.07192253497857));
#43876=CARTESIAN_POINT('Ctrl Pts',(3.18809755562368,-1.,-2.06684062744112));
#43877=CARTESIAN_POINT('Ctrl Pts',(3.18197692964614,-1.,-2.06166849827101));
#43878=CARTESIAN_POINT('Ctrl Pts',(3.17564906975371,-1.,-2.05650186773132));
#43879=CARTESIAN_POINT('Ctrl Pts',(3.16936341689527,-1.,-2.05151770247233));
#43880=CARTESIAN_POINT('Ctrl Pts',(3.16343165058912,-1.,-2.04693331247446));
#43881=CARTESIAN_POINT('Ctrl Pts',(3.15817983946367,-1.,-2.04297406404027));
#43882=CARTESIAN_POINT('Ctrl Pts',(3.15389991674792,-1.,-2.03984073791519));
#43883=CARTESIAN_POINT('Ctrl Pts',(3.15102344775328,-1.,-2.03783225495961));
#43884=CARTESIAN_POINT('Ctrl Pts',(3.14959882629805,-1.,-2.03693188810545));
#43885=CARTESIAN_POINT('Ctrl Pts',(3.1490119366901,-1.,-2.03663974554932));
#43886=CARTESIAN_POINT('Ctrl Pts',(3.14881939088124,-1.,-2.03659701539259));
#43887=CARTESIAN_POINT('Ctrl Pts',(3.14877060440327,-1.,-2.03660101169714));
#43888=CARTESIAN_POINT('',(3.24413672884812,-1.,-1.88097764062697));
#43889=CARTESIAN_POINT('Origin',(0.,-1.,0.));
#43890=CARTESIAN_POINT('',(3.70708211654725,-1.,-1.97421938526992));
#43891=CARTESIAN_POINT('Ctrl Pts',(3.24413672884812,-1.,-1.88097764062697));
#43892=CARTESIAN_POINT('Ctrl Pts',(3.24415531671284,-1.,-1.8810229239812));
#43893=CARTESIAN_POINT('Ctrl Pts',(3.24428080353022,-1.,-1.88117508446775));
#43894=CARTESIAN_POINT('Ctrl Pts',(3.24480754676064,-1.,-1.88156537699203));
#43895=CARTESIAN_POINT('Ctrl Pts',(3.2462565441079,-1.,-1.88242596600454));
#43896=CARTESIAN_POINT('Ctrl Pts',(3.24935200511918,-1.,-1.88407708646357));
#43897=CARTESIAN_POINT('Ctrl Pts',(3.25408686339463,-1.,-1.88646802523466));
#43898=CARTESIAN_POINT('Ctrl Pts',(3.25999885193947,-1.,-1.88934996203698));
#43899=CARTESIAN_POINT('Ctrl Pts',(3.26677653888676,-1.,-1.89255393500965));
#43900=CARTESIAN_POINT('Ctrl Pts',(3.27407108933139,-1.,-1.89589172903793));
#43901=CARTESIAN_POINT('Ctrl Pts',(3.28154737912352,-1.,-1.89918429230462));
#43902=CARTESIAN_POINT('Ctrl Pts',(3.2889344860029,-1.,-1.90228971247527));
#43903=CARTESIAN_POINT('Ctrl Pts',(3.29608978722113,-1.,-1.90513891864087));
#43904=CARTESIAN_POINT('Ctrl Pts',(3.30300595568195,-1.,-1.90773912171341));
#43905=CARTESIAN_POINT('Ctrl Pts',(3.30975721158596,-1.,-1.91014297830446));
#43906=CARTESIAN_POINT('Ctrl Pts',(3.31646052426364,-1.,-1.91242616234442));
#43907=CARTESIAN_POINT('Ctrl Pts',(3.32323403454535,-1.,-1.91466343916628));
#43908=CARTESIAN_POINT('Ctrl Pts',(3.33014884257873,-1.,-1.91690081930332));
#43909=CARTESIAN_POINT('Ctrl Pts',(3.33721230710012,-1.,-1.9191460961021));
#43910=CARTESIAN_POINT('Ctrl Pts',(3.34439448941961,-1.,-1.92138450828404));
#43911=CARTESIAN_POINT('Ctrl Pts',(3.35164424847223,-1.,-1.92358838440528));
#43912=CARTESIAN_POINT('Ctrl Pts',(3.35890824422965,-1.,-1.92572846125756));
#43913=CARTESIAN_POINT('Ctrl Pts',(3.36615168657567,-1.,-1.92778626543786));
#43914=CARTESIAN_POINT('Ctrl Pts',(3.37336807068043,-1.,-1.92975993109877));
#43915=CARTESIAN_POINT('Ctrl Pts',(3.3805676852555,-1.,-1.93165739093276));
#43916=CARTESIAN_POINT('Ctrl Pts',(3.38777076883256,-1.,-1.93349233176788));
#43917=CARTESIAN_POINT('Ctrl Pts',(3.39499923640795,-1.,-1.93527929945985));
#43918=CARTESIAN_POINT('Ctrl Pts',(3.40226802104109,-1.,-1.93702857723098));
#43919=CARTESIAN_POINT('Ctrl Pts',(3.40957978266642,-1.,-1.93874306008143));
#43920=CARTESIAN_POINT('Ctrl Pts',(3.41692971994096,-1.,-1.94042111965246));
#43921=CARTESIAN_POINT('Ctrl Pts',(3.42430850941503,-1.,-1.94205835913696));
#43922=CARTESIAN_POINT('Ctrl Pts',(3.43170586602434,-1.,-1.94364973660284));
#43923=CARTESIAN_POINT('Ctrl Pts',(3.43911410197687,-1.,-1.94519168842879));
#43924=CARTESIAN_POINT('Ctrl Pts',(3.44653088665681,-1.,-1.94668377715329));
#43925=CARTESIAN_POINT('Ctrl Pts',(3.45395731584051,-1.,-1.94812754766524));
#43926=CARTESIAN_POINT('Ctrl Pts',(3.46139661060962,-1.,-1.94952575850197));
#43927=CARTESIAN_POINT('Ctrl Pts',(3.46885258974191,-1.,-1.95088147859877));
#43928=CARTESIAN_POINT('Ctrl Pts',(3.47632820495921,-1.,-1.95219722189876));
#43929=CARTESIAN_POINT('Ctrl Pts',(3.48382414832634,-1.,-1.95347412486309));
#43930=CARTESIAN_POINT('Ctrl Pts',(3.49133956289133,-1.,-1.95471236969643));
#43931=CARTESIAN_POINT('Ctrl Pts',(3.49887263575583,-1.,-1.95591153823661));
#43932=CARTESIAN_POINT('Ctrl Pts',(3.50642124159909,-1.,-1.95707099606511));
#43933=CARTESIAN_POINT('Ctrl Pts',(3.51398354617794,-1.,-1.95819025316779));
#43934=CARTESIAN_POINT('Ctrl Pts',(3.52155867431486,-1.,-1.95926936324461));
#43935=CARTESIAN_POINT('Ctrl Pts',(3.52914648844351,-1.,-1.96030879411566));
#43936=CARTESIAN_POINT('Ctrl Pts',(3.53674730625813,-1.,-1.96130926212689));
#43937=CARTESIAN_POINT('Ctrl Pts',(3.54436163300443,-1.,-1.96227157573067));
#43938=CARTESIAN_POINT('Ctrl Pts',(3.55198990600886,-1.,-1.96319648628644));
#43939=CARTESIAN_POINT('Ctrl Pts',(3.55963218706096,-1.,-1.96408450906812));
#43940=CARTESIAN_POINT('Ctrl Pts',(3.56728820357791,-1.,-1.96493594634567));
#43941=CARTESIAN_POINT('Ctrl Pts',(3.57495748600959,-1.,-1.96575096652789));
#43942=CARTESIAN_POINT('Ctrl Pts',(3.58263947663829,-1.,-1.96652966688911));
#43943=CARTESIAN_POINT('Ctrl Pts',(3.59033364022801,-1.,-1.96727213799544));
#43944=CARTESIAN_POINT('Ctrl Pts',(3.59803959819938,-1.,-1.96797854118369));
#43945=CARTESIAN_POINT('Ctrl Pts',(3.60575714017989,-1.,-1.9686491188594));
#43946=CARTESIAN_POINT('Ctrl Pts',(3.61348615496704,-1.,-1.96928416040877));
#43947=CARTESIAN_POINT('Ctrl Pts',(3.62122658401893,-1.,-1.96988398129978));
#43948=CARTESIAN_POINT('Ctrl Pts',(3.62897836973293,-1.,-1.97044889850463));
#43949=CARTESIAN_POINT('Ctrl Pts',(3.63674139590412,-1.,-1.97097920454464));
#43950=CARTESIAN_POINT('Ctrl Pts',(3.64451546723514,-1.,-1.97147515441164));
#43951=CARTESIAN_POINT('Ctrl Pts',(3.652300347166,-1.,-1.9719369724024));
#43952=CARTESIAN_POINT('Ctrl Pts',(3.6600957816636,-1.,-1.9723648543905));
#43953=CARTESIAN_POINT('Ctrl Pts',(3.66790152752075,-1.,-1.97275897198678));
#43954=CARTESIAN_POINT('Ctrl Pts',(3.67571738107084,-1.,-1.97311947678517));
#43955=CARTESIAN_POINT('Ctrl Pts',(3.68354319915092,-1.,-1.97344650304519));
#43956=CARTESIAN_POINT('Ctrl Pts',(3.69137888599902,-1.,-1.97374016225483));
#43957=CARTESIAN_POINT('Ctrl Pts',(3.6976552856004,-1.,-1.97394846383216));
#43958=CARTESIAN_POINT('Ctrl Pts',(3.70236698912904,-1.,-1.97408973726715));
#43959=CARTESIAN_POINT('Ctrl Pts',(3.70551008132332,-1.,-1.97417727645308));
#43960=CARTESIAN_POINT('Ctrl Pts',(3.70708211654725,-1.,-1.97421938526992));
#43961=CARTESIAN_POINT('',(3.77614523045147,-1.,-1.83867539237861));
#43962=CARTESIAN_POINT('',(3.70708211654725,-1.,-1.97421938526992));
#43963=CARTESIAN_POINT('',(3.42859860294305,-1.,-1.5189508286633));
#43964=CARTESIAN_POINT('Ctrl Pts',(3.77614523045147,-1.,-1.83867539237861));
#43965=CARTESIAN_POINT('Ctrl Pts',(3.77518714457833,-1.,-1.83742834010626));
#43966=CARTESIAN_POINT('Ctrl Pts',(3.77326886064398,-1.,-1.83493697934534));
#43967=CARTESIAN_POINT('Ctrl Pts',(3.77038509817999,-1.,-1.83120816955646));
#43968=CARTESIAN_POINT('Ctrl Pts',(3.76652740353775,-1.,-1.82625289220915));
#43969=CARTESIAN_POINT('Ctrl Pts',(3.76168412707948,-1.,-1.82008629694091));
#43970=CARTESIAN_POINT('Ctrl Pts',(3.75681965683071,-1.,-1.8139472983358));
#43971=CARTESIAN_POINT('Ctrl Pts',(3.75193395887977,-1.,-1.80783603939617));
#43972=CARTESIAN_POINT('Ctrl Pts',(3.74702700875467,-1.,-1.8017527148577));
#43973=CARTESIAN_POINT('Ctrl Pts',(3.74209880352445,-1.,-1.79569757859422));
#43974=CARTESIAN_POINT('Ctrl Pts',(3.73714934730681,-1.,-1.78967092823491));
#43975=CARTESIAN_POINT('Ctrl Pts',(3.7321786309547,-1.,-1.78367308442901));
#43976=CARTESIAN_POINT('Ctrl Pts',(3.72718661205609,-1.,-1.77770437039658));
#43977=CARTESIAN_POINT('Ctrl Pts',(3.72217319911254,-1.,-1.77176509401761));
#43978=CARTESIAN_POINT('Ctrl Pts',(3.71713822377359,-1.,-1.76585552124394));
#43979=CARTESIAN_POINT('Ctrl Pts',(3.71208146346136,-1.,-1.75997588498865));
#43980=CARTESIAN_POINT('Ctrl Pts',(3.70700269736659,-1.,-1.75412641804042));
#43981=CARTESIAN_POINT('Ctrl Pts',(3.7019017567335,-1.,-1.74830738046057));
#43982=CARTESIAN_POINT('Ctrl Pts',(3.69677856910517,-1.,-1.74251908492617));
#43983=CARTESIAN_POINT('Ctrl Pts',(3.69163322648036,-1.,-1.73676193254557));
#43984=CARTESIAN_POINT('Ctrl Pts',(3.68646597019332,-1.,-1.73103640956717));
#43985=CARTESIAN_POINT('Ctrl Pts',(3.68127704936579,-1.,-1.72534302437056));
#43986=CARTESIAN_POINT('Ctrl Pts',(3.67606660374709,-1.,-1.71968225581808));
#43987=CARTESIAN_POINT('Ctrl Pts',(3.67083454901611,-1.,-1.71405450210384));
#43988=CARTESIAN_POINT('Ctrl Pts',(3.66558043198876,-1.,-1.70846001610956));
#43989=CARTESIAN_POINT('Ctrl Pts',(3.66030338774847,-1.,-1.70289888566873));
#43990=CARTESIAN_POINT('Ctrl Pts',(3.65500246526749,-1.,-1.69737117722534));
#43991=CARTESIAN_POINT('Ctrl Pts',(3.64967689827371,-1.,-1.69187705481689));
#43992=CARTESIAN_POINT('Ctrl Pts',(3.64432638915203,-1.,-1.68641690471457));
#43993=CARTESIAN_POINT('Ctrl Pts',(3.63895140887462,-1.,-1.68099146651586));
#43994=CARTESIAN_POINT('Ctrl Pts',(3.63355343201232,-1.,-1.67560193613156));
#43995=CARTESIAN_POINT('Ctrl Pts',(3.62813422105271,-1.,-1.67024966008045));
#43996=CARTESIAN_POINT('Ctrl Pts',(3.62269517989109,-1.,-1.66493585923855));
#43997=CARTESIAN_POINT('Ctrl Pts',(3.61723666482456,-1.,-1.65966133399186));
#43998=CARTESIAN_POINT('Ctrl Pts',(3.61175734965127,-1.,-1.65442619244325));
#43999=CARTESIAN_POINT('Ctrl Pts',(3.60625346556992,-1.,-1.64922952425832));
#44000=CARTESIAN_POINT('Ctrl Pts',(3.60072028513845,-1.,-1.64407004385582));
#44001=CARTESIAN_POINT('Ctrl Pts',(3.59515368334893,-1.,-1.63894676675352));
#44002=CARTESIAN_POINT('Ctrl Pts',(3.58955176627879,-1.,-1.6338597145126));
#44003=CARTESIAN_POINT('Ctrl Pts',(3.58391625774343,-1.,-1.62881051550745));
#44004=CARTESIAN_POINT('Ctrl Pts',(3.5782545595439,-1.,-1.62380329464844));
#44005=CARTESIAN_POINT('Ctrl Pts',(3.57257679609806,-1.,-1.61884340915404));
#44006=CARTESIAN_POINT('Ctrl Pts',(3.56689200468387,-1.,-1.61393581747514));
#44007=CARTESIAN_POINT('Ctrl Pts',(3.5612043248298,-1.,-1.60908344685457));
#44008=CARTESIAN_POINT('Ctrl Pts',(3.55550985096129,-1.,-1.60428584699853));
#44009=CARTESIAN_POINT('Ctrl Pts',(3.54979148634454,-1.,-1.59953698113457));
#44010=CARTESIAN_POINT('Ctrl Pts',(3.54402458182337,-1.,-1.59482766949766));
#44011=CARTESIAN_POINT('Ctrl Pts',(3.53818616861077,-1.,-1.59014958368739));
#44012=CARTESIAN_POINT('Ctrl Pts',(3.5322637814708,-1.,-1.58549906268088));
#44013=CARTESIAN_POINT('Ctrl Pts',(3.52626275334881,-1.,-1.58088027227848));
#44014=CARTESIAN_POINT('Ctrl Pts',(3.52021847865912,-1.,-1.57631049988158));
#44015=CARTESIAN_POINT('Ctrl Pts',(3.51418598431665,-1.,-1.57181569799743));
#44016=CARTESIAN_POINT('Ctrl Pts',(3.50821771695363,-1.,-1.56742097575012));
#44017=CARTESIAN_POINT('Ctrl Pts',(3.50234321621578,-1.,-1.56314187758675));
#44018=CARTESIAN_POINT('Ctrl Pts',(3.49655185179655,-1.,-1.55897703097874));
#44019=CARTESIAN_POINT('Ctrl Pts',(3.4907646087742,-1.,-1.55489595901116));
#44020=CARTESIAN_POINT('Ctrl Pts',(3.48485155928567,-1.,-1.55084702970452));
#44021=CARTESIAN_POINT('Ctrl Pts',(3.47868272898751,-1.,-1.54678009290276));
#44022=CARTESIAN_POINT('Ctrl Pts',(3.47217189224653,-1.,-1.54266605398188));
#44023=CARTESIAN_POINT('Ctrl Pts',(3.46531752207153,-1.,-1.53851507915502));
#44024=CARTESIAN_POINT('Ctrl Pts',(3.45825932955032,-1.,-1.53440195378792));
#44025=CARTESIAN_POINT('Ctrl Pts',(3.45127136828305,-1.,-1.53046244461635));
#44026=CARTESIAN_POINT('Ctrl Pts',(3.44469547526647,-1.,-1.52686242875556));
#44027=CARTESIAN_POINT('Ctrl Pts',(3.4388889597401,-1.,-1.5237734895035));
#44028=CARTESIAN_POINT('Ctrl Pts',(3.43417156977893,-1.,-1.52134826724293));
#44029=CARTESIAN_POINT('Ctrl Pts',(3.43101631893414,-1.,-1.5198144909338));
#44030=CARTESIAN_POINT('Ctrl Pts',(3.42946838852587,-1.,-1.51914806898491));
#44031=CARTESIAN_POINT('Ctrl Pts',(3.42884302333841,-1.,-1.5189513329503));
#44032=CARTESIAN_POINT('Ctrl Pts',(3.42864616361875,-1.,-1.51893924967331));
#44033=CARTESIAN_POINT('Ctrl Pts',(3.42859860294305,-1.,-1.5189508286633));
#44034=CARTESIAN_POINT('',(3.49844575334386,-1.,-1.35032489087269));
#44035=CARTESIAN_POINT('Origin',(0.,-1.,0.));
#44036=CARTESIAN_POINT('',(3.97027773754922,-1.,-1.36999806084572));
#44037=CARTESIAN_POINT('Ctrl Pts',(3.49844575334386,-1.,-1.35032489087269));
#44038=CARTESIAN_POINT('Ctrl Pts',(3.49847119623841,-1.,-1.35036670893102));
#44039=CARTESIAN_POINT('Ctrl Pts',(3.49861894124915,-1.,-1.35049736560633));
#44040=CARTESIAN_POINT('Ctrl Pts',(3.49920025459856,-1.,-1.35080045218652));
#44041=CARTESIAN_POINT('Ctrl Pts',(3.5007660381658,-1.,-1.35142377279535));
#44042=CARTESIAN_POINT('Ctrl Pts',(3.50408168106113,-1.,-1.3525703284343));
#44043=CARTESIAN_POINT('Ctrl Pts',(3.50913227060177,-1.,-1.35419113576022));
#44044=CARTESIAN_POINT('Ctrl Pts',(3.51542230699919,-1.,-1.35611275237288));
#44045=CARTESIAN_POINT('Ctrl Pts',(3.52261776117121,-1.,-1.35821701528975));
#44046=CARTESIAN_POINT('Ctrl Pts',(3.53034464961849,-1.,-1.36037259643827));
#44047=CARTESIAN_POINT('Ctrl Pts',(3.53824396425032,-1.,-1.36245507339334));
#44048=CARTESIAN_POINT('Ctrl Pts',(3.54602591832893,-1.,-1.36436666257568));
#44049=CARTESIAN_POINT('Ctrl Pts',(3.55353883995793,-1.,-1.36606145456711));
#44050=CARTESIAN_POINT('Ctrl Pts',(3.56077662028492,-1.,-1.36754771771174));
#44051=CARTESIAN_POINT('Ctrl Pts',(3.56782080304554,-1.,-1.36886584973349));
#44052=CARTESIAN_POINT('Ctrl Pts',(3.57479875549453,-1.,-1.37007229485646));
#44053=CARTESIAN_POINT('Ctrl Pts',(3.58183885982745,-1.,-1.37122241663073));
#44054=CARTESIAN_POINT('Ctrl Pts',(3.5890185384643,-1.,-1.37235053661));
#44055=CARTESIAN_POINT('Ctrl Pts',(3.59634627869117,-1.,-1.37346320103184));
#44056=CARTESIAN_POINT('Ctrl Pts',(3.60379020124038,-1.,-1.37455051379642));
#44057=CARTESIAN_POINT('Ctrl Pts',(3.61129546591082,-1.,-1.37559314436641));
#44058=CARTESIAN_POINT('Ctrl Pts',(3.61880481160408,-1.,-1.37657053403102));
#44059=CARTESIAN_POINT('Ctrl Pts',(3.62628098665112,-1.,-1.37746987919868));
#44060=CARTESIAN_POINT('Ctrl Pts',(3.63371727442448,-1.,-1.37829035457325));
#44061=CARTESIAN_POINT('Ctrl Pts',(3.64112507791112,-1.,-1.37903818567347));
#44062=CARTESIAN_POINT('Ctrl Pts',(3.64852652756444,-1.,-1.37972372481598));
#44063=CARTESIAN_POINT('Ctrl Pts',(3.65594554404396,-1.,-1.38035791051215));
#44064=CARTESIAN_POINT('Ctrl Pts',(3.66339848520874,-1.,-1.38094856333558));
#44065=CARTESIAN_POINT('Ctrl Pts',(3.67088843112282,-1.,-1.38149812653876));
#44066=CARTESIAN_POINT('Ctrl Pts',(3.6784103848243,-1.,-1.38200574290626));
#44067=CARTESIAN_POINT('Ctrl Pts',(3.68595444983844,-1.,-1.38246852827185));
#44068=CARTESIAN_POINT('Ctrl Pts',(3.69350967899523,-1.,-1.38288311171649));
#44069=CARTESIAN_POINT('Ctrl Pts',(3.70106792167894,-1.,-1.38324717612862));
#44070=CARTESIAN_POINT('Ctrl Pts',(3.70862680753343,-1.,-1.38356065402122));
#44071=CARTESIAN_POINT('Ctrl Pts',(3.7161876605181,-1.,-1.38382489984585));
#44072=CARTESIAN_POINT('Ctrl Pts',(3.72375409358805,-1.,-1.3840421342895));
#44073=CARTESIAN_POINT('Ctrl Pts',(3.73133035859283,-1.,-1.38421479111531));
#44074=CARTESIAN_POINT('Ctrl Pts',(3.73891976418099,-1.,-1.38434489156456));
#44075=CARTESIAN_POINT('Ctrl Pts',(3.7465231716786,-1.,-1.38443344984389));
#44076=CARTESIAN_POINT('Ctrl Pts',(3.75413976318727,-1.,-1.38448077997155));
#44077=CARTESIAN_POINT('Ctrl Pts',(3.76176768271347,-1.,-1.38448675253343));
#44078=CARTESIAN_POINT('Ctrl Pts',(3.76940473185775,-1.,-1.38445107339517));
#44079=CARTESIAN_POINT('Ctrl Pts',(3.77704902230441,-1.,-1.38437354551435));
#44080=CARTESIAN_POINT('Ctrl Pts',(3.78469969805134,-1.,-1.38425435883773));
#44081=CARTESIAN_POINT('Ctrl Pts',(3.79235669640907,-1.,-1.38409399694589));
#44082=CARTESIAN_POINT('Ctrl Pts',(3.80002044322169,-1.,-1.38389311766701));
#44083=CARTESIAN_POINT('Ctrl Pts',(3.80769156398429,-1.,-1.38365244046226));
#44084=CARTESIAN_POINT('Ctrl Pts',(3.81537060817765,-1.,-1.38337263902766));
#44085=CARTESIAN_POINT('Ctrl Pts',(3.82305771743715,-1.,-1.38305421262724));
#44086=CARTESIAN_POINT('Ctrl Pts',(3.83075266982138,-1.,-1.38269750245086));
#44087=CARTESIAN_POINT('Ctrl Pts',(3.83845502790609,-1.,-1.38230274828774));
#44088=CARTESIAN_POINT('Ctrl Pts',(3.84616425605705,-1.,-1.38187013346089));
#44089=CARTESIAN_POINT('Ctrl Pts',(3.85387983979557,-1.,-1.38139983115075));
#44090=CARTESIAN_POINT('Ctrl Pts',(3.86160143044187,-1.,-1.38089205993068));
#44091=CARTESIAN_POINT('Ctrl Pts',(3.86932885813403,-1.,-1.38034709213129));
#44092=CARTESIAN_POINT('Ctrl Pts',(3.87706205830865,-1.,-1.37976523097187));
#44093=CARTESIAN_POINT('Ctrl Pts',(3.88480102249461,-1.,-1.37914679719446));
#44094=CARTESIAN_POINT('Ctrl Pts',(3.89254574338385,-1.,-1.37849211287981));
#44095=CARTESIAN_POINT('Ctrl Pts',(3.90029615196255,-1.,-1.3778014851263));
#44096=CARTESIAN_POINT('Ctrl Pts',(3.90805209522729,-1.,-1.3770751963376));
#44097=CARTESIAN_POINT('Ctrl Pts',(3.91581337461825,-1.,-1.37631350505516));
#44098=CARTESIAN_POINT('Ctrl Pts',(3.92357976987132,-1.,-1.37551664448057));
#44099=CARTESIAN_POINT('Ctrl Pts',(3.93135106761941,-1.,-1.37468482215784));
#44100=CARTESIAN_POINT('Ctrl Pts',(3.93912709041791,-1.,-1.37381821967499));
#44101=CARTESIAN_POINT('Ctrl Pts',(3.94690771786926,-1.,-1.37291699203423));
#44102=CARTESIAN_POINT('Ctrl Pts',(3.95469287283105,-1.,-1.37198126433139));
#44103=CARTESIAN_POINT('Ctrl Pts',(3.96092458508407,-1.,-1.37120515615663));
#44104=CARTESIAN_POINT('Ctrl Pts',(3.96560037975788,-1.,-1.37060761746027));
#44105=CARTESIAN_POINT('Ctrl Pts',(3.9687184694173,-1.,-1.37020239094758));
#44106=CARTESIAN_POINT('Ctrl Pts',(3.97027773754922,-1.,-1.36999806084572));
#44107=CARTESIAN_POINT('',(4.01728681790024,-1.,-1.22531898815164));
#44108=CARTESIAN_POINT('',(3.97027773754922,-1.,-1.36999806084572));
#44109=CARTESIAN_POINT('',(3.62400312501199,-1.,-0.963899035118986));
#44110=CARTESIAN_POINT('Ctrl Pts',(4.01728681790024,-1.,-1.22531898815164));
#44111=CARTESIAN_POINT('Ctrl Pts',(4.01614544569895,-1.,-1.22423716681317));
#44112=CARTESIAN_POINT('Ctrl Pts',(4.01386104433519,-1.,-1.22207656455845));
#44113=CARTESIAN_POINT('Ctrl Pts',(4.01042947140789,-1.,-1.21884478244403));
#44114=CARTESIAN_POINT('Ctrl Pts',(4.00584409522722,-1.,-1.21455398918133));
#44115=CARTESIAN_POINT('Ctrl Pts',(4.00009577950721,-1.,-1.20922097029551));
#44116=CARTESIAN_POINT('Ctrl Pts',(3.99433084799666,-1.,-1.20391852375139));
#44117=CARTESIAN_POINT('Ctrl Pts',(3.98854928957189,-1.,-1.19864679609566));
#44118=CARTESIAN_POINT('Ctrl Pts',(3.98275111052561,-1.,-1.19340598349475));
#44119=CARTESIAN_POINT('Ctrl Pts',(3.97693634767754,-1.,-1.18819633715539));
#44120=CARTESIAN_POINT('Ctrl Pts',(3.97110505165415,-1.,-1.18301815039831));
#44121=CARTESIAN_POINT('Ctrl Pts',(3.96525726358159,-1.,-1.17787174135592));
#44122=CARTESIAN_POINT('Ctrl Pts',(3.95939299213276,-1.,-1.17275743590361));
#44123=CARTESIAN_POINT('Ctrl Pts',(3.95351219509876,-1.,-1.16767555244438));
#44124=CARTESIAN_POINT('Ctrl Pts',(3.94761474780583,-1.,-1.16262637999157));
#44125=CARTESIAN_POINT('Ctrl Pts',(3.94170046685203,-1.,-1.15761018340956));
#44126=CARTESIAN_POINT('Ctrl Pts',(3.9357691705628,-1.,-1.1526272271632));
#44127=CARTESIAN_POINT('Ctrl Pts',(3.92982073294257,-1.,-1.14767779451124));
#44128=CARTESIAN_POINT('Ctrl Pts',(3.92385513133997,-1.,-1.14276220561593));
#44129=CARTESIAN_POINT('Ctrl Pts',(3.91787251936827,-1.,-1.13788084225554));
#44130=CARTESIAN_POINT('Ctrl Pts',(3.91187321145649,-1.,-1.13303414693896));
#44131=CARTESIAN_POINT('Ctrl Pts',(3.90585753318737,-1.,-1.12822258281553));
#44132=CARTESIAN_POINT('Ctrl Pts',(3.89982569750025,-1.,-1.12344660099043));
#44133=CARTESIAN_POINT('Ctrl Pts',(3.89377768340344,-1.,-1.11870660794603));
#44134=CARTESIAN_POINT('Ctrl Pts',(3.88771308285171,-1.,-1.11400292434429));
#44135=CARTESIAN_POINT('Ctrl Pts',(3.88163105531724,-1.,-1.10933577224008));
#44136=CARTESIAN_POINT('Ctrl Pts',(3.87553067187514,-1.,-1.10470536603287));
#44137=CARTESIAN_POINT('Ctrl Pts',(3.86941120134849,-1.,-1.10011198761195));
#44138=CARTESIAN_POINT('Ctrl Pts',(3.86327241021247,-1.,-1.09555606505013));
#44139=CARTESIAN_POINT('Ctrl Pts',(3.85711487933931,-1.,-1.09103825516294));
#44140=CARTESIAN_POINT('Ctrl Pts',(3.85094025222713,-1.,-1.08655950846384));
#44141=CARTESIAN_POINT('Ctrl Pts',(3.8447504803063,-1.,-1.08212087917991));
#44142=CARTESIAN_POINT('Ctrl Pts',(3.83854714117491,-1.,-1.07772335353858));
#44143=CARTESIAN_POINT('Ctrl Pts',(3.83233071195144,-1.,-1.07336766633459));
#44144=CARTESIAN_POINT('Ctrl Pts',(3.82609989967276,-1.,-1.06905413180359));
#44145=CARTESIAN_POINT('Ctrl Pts',(3.81985083953012,-1.,-1.0647824403893));
#44146=CARTESIAN_POINT('Ctrl Pts',(3.8135786611749,-1.,-1.06055206187299));
#44147=CARTESIAN_POINT('Ctrl Pts',(3.80727913637791,-1.,-1.05636266918644));
#44148=CARTESIAN_POINT('Ctrl Pts',(3.80095039790681,-1.,-1.05221457990016));
#44149=CARTESIAN_POINT('Ctrl Pts',(3.79459440308786,-1.,-1.04810913267639));
#44150=CARTESIAN_POINT('Ctrl Pts',(3.78821910787179,-1.,-1.04404924374422));
#44151=CARTESIAN_POINT('Ctrl Pts',(3.7818353500817,-1.,-1.04003862055798));
#44152=CARTESIAN_POINT('Ctrl Pts',(3.77545283140427,-1.,-1.03608074678008));
#44153=CARTESIAN_POINT('Ctrl Pts',(3.76907609832516,-1.,-1.03217786604919));
#44154=CARTESIAN_POINT('Ctrl Pts',(3.76270122291245,-1.,-1.02833014458184));
#44155=CARTESIAN_POINT('Ctrl Pts',(3.75631037456224,-1.,-1.02453429444668));
#44156=CARTESIAN_POINT('Ctrl Pts',(3.74987777155873,-1.,-1.02078510487439));
#44157=CARTESIAN_POINT('Ctrl Pts',(3.74337942504993,-1.,-1.01707794311088));
#44158=CARTESIAN_POINT('Ctrl Pts',(3.73680245055747,-1.,-1.01341114319906));
#44159=CARTESIAN_POINT('Ctrl Pts',(3.73015276704407,-1.,-1.00978798539491));
#44160=CARTESIAN_POINT('Ctrl Pts',(3.72346803750544,-1.,-1.00622000735696));
#44161=CARTESIAN_POINT('Ctrl Pts',(3.71680667125047,-1.,-1.00272423396802));
#44162=CARTESIAN_POINT('Ctrl Pts',(3.7102243971387,-1.,-0.999317260756345));
#44163=CARTESIAN_POINT('Ctrl Pts',(3.70375282282107,-1.,-0.996009819772432));
#44164=CARTESIAN_POINT('Ctrl Pts',(3.69738123415696,-1.,-0.992802218332104));
#44165=CARTESIAN_POINT('Ctrl Pts',(3.69102682138955,-1.,-0.989676715398859));
#44166=CARTESIAN_POINT('Ctrl Pts',(3.6845531792623,-1.,-0.986602639864286));
#44167=CARTESIAN_POINT('Ctrl Pts',(3.67782408841876,-1.,-0.983550791470865));
#44168=CARTESIAN_POINT('Ctrl Pts',(3.67074983340444,-1.,-0.980505922458495));
#44169=CARTESIAN_POINT('Ctrl Pts',(3.66333049637403,-1.,-0.977478312751416));
#44170=CARTESIAN_POINT('Ctrl Pts',(3.6557157673487,-1.,-0.974519971354139));
#44171=CARTESIAN_POINT('Ctrl Pts',(3.64819756447072,-1.,-0.971722122060278));
#44172=CARTESIAN_POINT('Ctrl Pts',(3.64113946505393,-1.,-0.969195124674829));
#44173=CARTESIAN_POINT('Ctrl Pts',(3.6349212208096,-1.,-0.967052554540878));
#44174=CARTESIAN_POINT('Ctrl Pts',(3.62988252139998,-1.,-0.965395153165716));
#44175=CARTESIAN_POINT('Ctrl Pts',(3.62652618145252,-1.,-0.964373850166081));
#44176=CARTESIAN_POINT('Ctrl Pts',(3.62489305727516,-1.,-0.963957782642589));
#44177=CARTESIAN_POINT('Ctrl Pts',(3.62424461507455,-1.,-0.963861297423579));
#44178=CARTESIAN_POINT('Ctrl Pts',(3.62404828878374,-1.,-0.963880158556713));
#44179=CARTESIAN_POINT('Ctrl Pts',(3.62400312501199,-1.,-0.963899035118986));
#44180=CARTESIAN_POINT('',(3.66661143271648,-1.,-0.786422660833743));
#44181=CARTESIAN_POINT('Origin',(0.,-1.,0.));
#44182=CARTESIAN_POINT('',(4.13571194405636,-1.,-0.73204283740062));
#44183=CARTESIAN_POINT('Ctrl Pts',(3.66661143271648,-1.,-0.786422660833743));
#44184=CARTESIAN_POINT('Ctrl Pts',(3.66664310415236,-1.,-0.786459983896781));
#44185=CARTESIAN_POINT('Ctrl Pts',(3.66680946938396,-1.,-0.78656591955989));
#44186=CARTESIAN_POINT('Ctrl Pts',(3.66743103898844,-1.,-0.7867743371985));
#44187=CARTESIAN_POINT('Ctrl Pts',(3.66907505398769,-1.,-0.787145041181589));
#44188=CARTESIAN_POINT('Ctrl Pts',(3.672529236635,-1.,-0.787758799995427));
#44189=CARTESIAN_POINT('Ctrl Pts',(3.67777119516438,-1.,-0.788569566220663));
#44190=CARTESIAN_POINT('Ctrl Pts',(3.68428439784285,-1.,-0.789483546065159));
#44191=CARTESIAN_POINT('Ctrl Pts',(3.69172044327754,-1.,-0.79043628498958));
#44192=CARTESIAN_POINT('Ctrl Pts',(3.69968940808982,-1.,-0.791356575696509));
#44193=CARTESIAN_POINT('Ctrl Pts',(3.70781724021879,-1.,-0.792177688845968));
#44194=CARTESIAN_POINT('Ctrl Pts',(3.7158024239604,-1.,-0.792848377370116));
#44195=CARTESIAN_POINT('Ctrl Pts',(3.7234879729357,-1.,-0.793347023783871));
#44196=CARTESIAN_POINT('Ctrl Pts',(3.7308691469564,-1.,-0.793682750269348));
#44197=CARTESIAN_POINT('Ctrl Pts',(3.73803280541576,-1.,-0.793882700936791));
#44198=CARTESIAN_POINT('Ctrl Pts',(3.74511357728827,-1.,-0.79398270045988));
#44199=CARTESIAN_POINT('Ctrl Pts',(3.75224692493895,-1.,-0.794017347371441));
#44200=CARTESIAN_POINT('Ctrl Pts',(3.75951468666325,-1.,-0.794008429135047));
#44201=CARTESIAN_POINT('Ctrl Pts',(3.76692626931184,-1.,-0.793961083689141));
#44202=CARTESIAN_POINT('Ctrl Pts',(3.77444863801264,-1.,-0.793870523787515));
#44203=CARTESIAN_POINT('Ctrl Pts',(3.78202460377617,-1.,-0.79372623578134));
#44204=CARTESIAN_POINT('Ctrl Pts',(3.78959439439222,-1.,-0.793516871680966));
#44205=CARTESIAN_POINT('Ctrl Pts',(3.79711921389862,-1.,-0.793235612973201));
#44206=CARTESIAN_POINT('Ctrl Pts',(3.80459229925598,-1.,-0.792882695234693));
#44207=CARTESIAN_POINT('Ctrl Pts',(3.81202588694726,-1.,-0.792462483517568));
#44208=CARTESIAN_POINT('Ctrl Pts',(3.81944345442237,-1.,-0.791981740718607));
#44209=CARTESIAN_POINT('Ctrl Pts',(3.82687033899799,-1.,-0.791447528662381));
#44210=CARTESIAN_POINT('Ctrl Pts',(3.83432392054804,-1.,-0.79086501270534));
#44211=CARTESIAN_POINT('Ctrl Pts',(3.84180762342476,-1.,-0.790236124191289));
#44212=CARTESIAN_POINT('Ctrl Pts',(3.8493163780891,-1.,-0.789560798155619));
#44213=CARTESIAN_POINT('Ctrl Pts',(3.85683995872536,-1.,-0.788837734090688));
#44214=CARTESIAN_POINT('Ctrl Pts',(3.86436702561342,-1.,-0.788065315093771));
#44215=CARTESIAN_POINT('Ctrl Pts',(3.87188916600905,-1.,-0.787242527617981));
#44216=CARTESIAN_POINT('Ctrl Pts',(3.87940402818186,-1.,-0.786369675812592));
#44217=CARTESIAN_POINT('Ctrl Pts',(3.88691313167399,-1.,-0.785447890340723));
#44218=CARTESIAN_POINT('Ctrl Pts',(3.89442039235105,-1.,-0.784478799358336));
#44219=CARTESIAN_POINT('Ctrl Pts',(3.90193039043971,-1.,-0.783464141529083));
#44220=CARTESIAN_POINT('Ctrl Pts',(3.90944671004536,-1.,-0.782405395622759));
#44221=CARTESIAN_POINT('Ctrl Pts',(3.9169703605466,-1.,-0.781303428618344));
#44222=CARTESIAN_POINT('Ctrl Pts',(3.92450058323799,-1.,-0.780158678615507));
#44223=CARTESIAN_POINT('Ctrl Pts',(3.93203552473153,-1.,-0.778971308134786));
#44224=CARTESIAN_POINT('Ctrl Pts',(3.93957296768098,-1.,-0.77774137056855));
#44225=CARTESIAN_POINT('Ctrl Pts',(3.94711101619471,-1.,-0.77646896669796));
#44226=CARTESIAN_POINT('Ctrl Pts',(3.95464885452364,-1.,-0.775154418039442));
#44227=CARTESIAN_POINT('Ctrl Pts',(3.96218649639876,-1.,-0.773798212026683));
#44228=CARTESIAN_POINT('Ctrl Pts',(3.96972446532832,-1.,-0.772400931772239));
#44229=CARTESIAN_POINT('Ctrl Pts',(3.97726349165507,-1.,-0.770963190030504));
#44230=CARTESIAN_POINT('Ctrl Pts',(3.98480422348403,-1.,-0.76948556624546));
#44231=CARTESIAN_POINT('Ctrl Pts',(3.99234687880892,-1.,-0.767968531377708));
#44232=CARTESIAN_POINT('Ctrl Pts',(3.99989129179464,-1.,-0.766412457135786));
#44233=CARTESIAN_POINT('Ctrl Pts',(4.00743706791366,-1.,-0.764817648784947));
#44234=CARTESIAN_POINT('Ctrl Pts',(4.01498370680434,-1.,-0.763184371182827));
#44235=CARTESIAN_POINT('Ctrl Pts',(4.02253072741347,-1.,-0.761512875859942));
#44236=CARTESIAN_POINT('Ctrl Pts',(4.0300778195465,-1.,-0.759803433244166));
#44237=CARTESIAN_POINT('Ctrl Pts',(4.03762485803468,-1.,-0.758056338885554));
#44238=CARTESIAN_POINT('Ctrl Pts',(4.04517182654344,-1.,-0.756271902370187));
#44239=CARTESIAN_POINT('Ctrl Pts',(4.05271876688106,-1.,-0.754450441816412));
#44240=CARTESIAN_POINT('Ctrl Pts',(4.06026572221399,-1.,-0.752592276482869));
#44241=CARTESIAN_POINT('Ctrl Pts',(4.06781267241886,-1.,-0.750697720483176));
#44242=CARTESIAN_POINT('Ctrl Pts',(4.07535951055363,-1.,-0.748767076679177));
#44243=CARTESIAN_POINT('Ctrl Pts',(4.08290608094789,-1.,-0.746800631490822));
#44244=CARTESIAN_POINT('Ctrl Pts',(4.09045220253011,-1.,-0.744798649705514));
#44245=CARTESIAN_POINT('Ctrl Pts',(4.09799769702712,-1.,-0.742761369690018));
#44246=CARTESIAN_POINT('Ctrl Pts',(4.1055424175856,-1.,-0.740688998555152));
#44247=CARTESIAN_POINT('Ctrl Pts',(4.11308626953795,-1.,-0.738581708229119));
#44248=CARTESIAN_POINT('Ctrl Pts',(4.12062919626082,-1.,-0.736439634335347));
#44249=CARTESIAN_POINT('Ctrl Pts',(4.12666277572794,-1.,-0.734698226767513));
#44250=CARTESIAN_POINT('Ctrl Pts',(4.13118752796397,-1.,-0.733376589325634));
#44251=CARTESIAN_POINT('Ctrl Pts',(4.13420383737278,-1.,-0.732488575135926));
#44252=CARTESIAN_POINT('Ctrl Pts',(4.13571194405636,-1.,-0.73204283740062));
#44253=CARTESIAN_POINT('',(4.15950947128175,-1.,-0.581791163835815));
#44254=CARTESIAN_POINT('',(4.13571194405636,-1.,-0.73204283740062));
#44255=CARTESIAN_POINT('',(3.73017266276632,-1.,-0.385112848332549));
#44256=CARTESIAN_POINT('Ctrl Pts',(4.15950947128175,-1.,-0.581791163835815));
#44257=CARTESIAN_POINT('Ctrl Pts',(4.15821291712391,-1.,-0.580901211462913));
#44258=CARTESIAN_POINT('Ctrl Pts',(4.15561864787379,-1.,-0.579124568912544));
#44259=CARTESIAN_POINT('Ctrl Pts',(4.1517237611974,-1.,-0.576469391673917));
#44260=CARTESIAN_POINT('Ctrl Pts',(4.14652361065787,-1.,-0.572948736066277));
#44261=CARTESIAN_POINT('Ctrl Pts',(4.14001179828669,-1.,-0.568580610187116));
#44262=CARTESIAN_POINT('Ctrl Pts',(4.13348835726086,-1.,-0.564245279535706));
#44263=CARTESIAN_POINT('Ctrl Pts',(4.12695329951859,-1.,-0.559942890594628));
#44264=CARTESIAN_POINT('Ctrl Pts',(4.1204066619623,-1.,-0.555673636130778));
#44265=CARTESIAN_POINT('Ctrl Pts',(4.11384852025578,-1.,-0.551437758498247));
#44266=CARTESIAN_POINT('Ctrl Pts',(4.1072789702877,-1.,-0.54723553948676));
#44267=CARTESIAN_POINT('Ctrl Pts',(4.10069810244473,-1.,-0.543067286878457));
#44268=CARTESIAN_POINT('Ctrl Pts',(4.09410597627116,-1.,-0.538933321179921));
#44269=CARTESIAN_POINT('Ctrl Pts',(4.08750259988693,-1.,-0.534833963477));
#44270=CARTESIAN_POINT('Ctrl Pts',(4.08088789536488,-1.,-0.530769518728076));
#44271=CARTESIAN_POINT('Ctrl Pts',(4.07426172299496,-1.,-0.526740277227));
#44272=CARTESIAN_POINT('Ctrl Pts',(4.06762394471075,-1.,-0.522746528602768));
#44273=CARTESIAN_POINT('Ctrl Pts',(4.06097448037934,-1.,-0.51878857233681));
#44274=CARTESIAN_POINT('Ctrl Pts',(4.05431335771261,-1.,-0.514866728193104));
#44275=CARTESIAN_POINT('Ctrl Pts',(4.04764078815591,-1.,-0.510981349219174));
#44276=CARTESIAN_POINT('Ctrl Pts',(4.04095715149074,-1.,-0.507132823288362));
#44277=CARTESIAN_POINT('Ctrl Pts',(4.0342628417439,-1.,-0.503321556915514));
#44278=CARTESIAN_POINT('Ctrl Pts',(4.0275581398015,-1.,-0.49954796234089));
#44279=CARTESIAN_POINT('Ctrl Pts',(4.02084308851813,-1.,-0.495812444326223));
#44280=CARTESIAN_POINT('Ctrl Pts',(4.01411733503486,-1.,-0.492115383417931));
#44281=CARTESIAN_POINT('Ctrl Pts',(4.0073800839092,-1.,-0.488457130424531));
#44282=CARTESIAN_POINT('Ctrl Pts',(4.00063045119234,-1.,-0.484838042421754));
#44283=CARTESIAN_POINT('Ctrl Pts',(3.99386775880655,-1.,-0.481258512209638));
#44284=CARTESIAN_POINT('Ctrl Pts',(3.98709184306743,-1.,-0.477718999122033));
#44285=CARTESIAN_POINT('Ctrl Pts',(3.9803033804443,-1.,-0.474220061019542));
#44286=CARTESIAN_POINT('Ctrl Pts',(3.97350414289415,-1.,-0.470762379613478));
#44287=CARTESIAN_POINT('Ctrl Pts',(3.96669622273946,-1.,-0.467346690880672));
#44288=CARTESIAN_POINT('Ctrl Pts',(3.95988133243543,-1.,-0.463973722115745));
#44289=CARTESIAN_POINT('Ctrl Pts',(3.95306005817363,-1.,-0.460644124429119));
#44290=CARTESIAN_POINT('Ctrl Pts',(3.94623117206675,-1.,-0.457358410451674));
#44291=CARTESIAN_POINT('Ctrl Pts',(3.93939080846298,-1.,-0.454116879027576));
#44292=CARTESIAN_POINT('Ctrl Pts',(3.93253407403128,-1.,-0.450919768356347));
#44293=CARTESIAN_POINT('Ctrl Pts',(3.92565674143424,-1.,-0.447767416837297));
#44294=CARTESIAN_POINT('Ctrl Pts',(3.91875701610721,-1.,-0.444660430230593));
#44295=CARTESIAN_POINT('Ctrl Pts',(3.91183704069146,-1.,-0.441599824524048));
#44296=CARTESIAN_POINT('Ctrl Pts',(3.90490512938546,-1.,-0.438587235458234));
#44297=CARTESIAN_POINT('Ctrl Pts',(3.8979725665544,-1.,-0.435624629433506));
#44298=CARTESIAN_POINT('Ctrl Pts',(3.89104947940592,-1.,-0.43271392954444));
#44299=CARTESIAN_POINT('Ctrl Pts',(3.88414070943334,-1.,-0.429856640579734));
#44300=CARTESIAN_POINT('Ctrl Pts',(3.87724240306609,-1.,-0.427053541173469));
#44301=CARTESIAN_POINT('Ctrl Pts',(3.87033643487882,-1.,-0.424304173195143));
#44302=CARTESIAN_POINT('Ctrl Pts',(3.86339652542749,-1.,-0.421607423177576));
#44303=CARTESIAN_POINT('Ctrl Pts',(3.85639825648031,-1.,-0.41896246808681));
#44304=CARTESIAN_POINT('Ctrl Pts',(3.8493286415751,-1.,-0.41636967805292));
#44305=CARTESIAN_POINT('Ctrl Pts',(3.84219403994742,-1.,-0.413831367016727));
#44306=CARTESIAN_POINT('Ctrl Pts',(3.83503345578645,-1.,-0.41135303879846));
#44307=CARTESIAN_POINT('Ctrl Pts',(3.82790724256397,-1.,-0.408942371447377));
#44308=CARTESIAN_POINT('Ctrl Pts',(3.82087303913741,-1.,-0.406607038258907));
#44309=CARTESIAN_POINT('Ctrl Pts',(3.81396374287762,-1.,-0.404352694628237));
#44310=CARTESIAN_POINT('Ctrl Pts',(3.80716881962763,-1.,-0.402181320148475));
#44311=CARTESIAN_POINT('Ctrl Pts',(3.80040370384659,-1.,-0.400088346504727));
#44312=CARTESIAN_POINT('Ctrl Pts',(3.79352887163457,-1.,-0.398064818684159));
#44313=CARTESIAN_POINT('Ctrl Pts',(3.78640521279479,-1.,-0.396103205335029));
#44314=CARTESIAN_POINT('Ctrl Pts',(3.77894173114368,-1.,-0.394202481011595));
#44315=CARTESIAN_POINT('Ctrl Pts',(3.77114011595892,-1.,-0.392372786223347));
#44316=CARTESIAN_POINT('Ctrl Pts',(3.76315635032993,-1.,-0.390642072979259));
#44317=CARTESIAN_POINT('Ctrl Pts',(3.75529302894757,-1.,-0.389054775898251));
#44318=CARTESIAN_POINT('Ctrl Pts',(3.74792651696269,-1.,-0.387663020050396));
#44319=CARTESIAN_POINT('Ctrl Pts',(3.74144965781088,-1.,-0.386519576222036));
#44320=CARTESIAN_POINT('Ctrl Pts',(3.73621371845475,-1.,-0.385670806454744));
#44321=CARTESIAN_POINT('Ctrl Pts',(3.73273893363318,-1.,-0.385187124633965));
#44322=CARTESIAN_POINT('Ctrl Pts',(3.73106082862399,-1.,-0.385031656499142));
#44323=CARTESIAN_POINT('Ctrl Pts',(3.73040527620929,-1.,-0.385037797882046));
#44324=CARTESIAN_POINT('Ctrl Pts',(3.73021431755218,-1.,-0.385087139001609));
#44325=CARTESIAN_POINT('Ctrl Pts',(3.73017266276632,-1.,-0.385112848332549));
#44326=CARTESIAN_POINT('',(3.74449296982994,-1.,-0.203156094897896));
#44327=CARTESIAN_POINT('Origin',(0.,-1.,0.));
#44328=CARTESIAN_POINT('',(4.19931119685982,-1.,-0.0760622897878241));
#44329=CARTESIAN_POINT('Ctrl Pts',(3.74449296982994,-1.,-0.203156094897896));
#44330=CARTESIAN_POINT('Ctrl Pts',(3.74453008995129,-1.,-0.203188003947965));
#44331=CARTESIAN_POINT('Ctrl Pts',(3.74471097893961,-1.,-0.203266610111264));
#44332=CARTESIAN_POINT('Ctrl Pts',(3.74535749969262,-1.,-0.203375226874332));
#44333=CARTESIAN_POINT('Ctrl Pts',(3.74703926501843,-1.,-0.203484186269315));
#44334=CARTESIAN_POINT('Ctrl Pts',(3.75054693397716,-1.,-0.203550035479097));
#44335=CARTESIAN_POINT('Ctrl Pts',(3.75585118707924,-1.,-0.203530796848404));
#44336=CARTESIAN_POINT('Ctrl Pts',(3.76242717937273,-1.,-0.203414634707647));
#44337=CARTESIAN_POINT('Ctrl Pts',(3.76992071595267,-1.,-0.203192390045338));
#44338=CARTESIAN_POINT('Ctrl Pts',(3.77793553476879,-1.,-0.202854729699197));
#44339=CARTESIAN_POINT('Ctrl Pts',(3.78609175019317,-1.,-0.202394260512193));
#44340=CARTESIAN_POINT('Ctrl Pts',(3.79408354187274,-1.,-0.201807533800799));
#44341=CARTESIAN_POINT('Ctrl Pts',(3.80175247447171,-1.,-0.201097756307252));
#44342=CARTESIAN_POINT('Ctrl Pts',(3.80909529318501,-1.,-0.20027467943329));
#44343=CARTESIAN_POINT('Ctrl Pts',(3.81620203429702,-1.,-0.199351525297397));
#44344=CARTESIAN_POINT('Ctrl Pts',(3.82321127348981,-1.,-0.19834261690047));
#44345=CARTESIAN_POINT('Ctrl Pts',(3.83026221776488,-1.,-0.197260935827375));
#44346=CARTESIAN_POINT('Ctrl Pts',(3.83743910616265,-1.,-0.19611519897189));
#44347=CARTESIAN_POINT('Ctrl Pts',(3.84475203347052,-1.,-0.194909009460255));
#44348=CARTESIAN_POINT('Ctrl Pts',(3.85216762264019,-1.,-0.193642806777748));
#44349=CARTESIAN_POINT('Ctrl Pts',(3.85962774407652,-1.,-0.19231515304498));
#44350=CARTESIAN_POINT('Ctrl Pts',(3.8670715862477,-1.,-0.190924190418613));
#44351=CARTESIAN_POINT('Ctrl Pts',(3.87445976418377,-1.,-0.189469253358255));
#44352=CARTESIAN_POINT('Ctrl Pts',(3.88178563496187,-1.,-0.187951632512664));
#44353=CARTESIAN_POINT('Ctrl Pts',(3.88906196725817,-1.,-0.186373724985263));
#44354=CARTESIAN_POINT('Ctrl Pts',(3.89631300742633,-1.,-0.184738537728035));
#44355=CARTESIAN_POINT('Ctrl Pts',(3.90356488555138,-1.,-0.183049081993193));
#44356=CARTESIAN_POINT('Ctrl Pts',(3.91083557557193,-1.,-0.181307740731796));
#44357=CARTESIAN_POINT('Ctrl Pts',(3.91812876180948,-1.,-0.179515885822895));
#44358=CARTESIAN_POINT('Ctrl Pts',(3.92543942697672,-1.,-0.177674246152328));
#44359=CARTESIAN_POINT('Ctrl Pts',(3.93275726771049,-1.,-0.175783136893873));
#44360=CARTESIAN_POINT('Ctrl Pts',(3.94007083096214,-1.,-0.173842734974608));
#44361=CARTESIAN_POINT('Ctrl Pts',(3.94737164900861,-1.,-0.171853355369233));
#44362=CARTESIAN_POINT('Ctrl Pts',(3.95465744665263,-1.,-0.16981566637413));
#44363=CARTESIAN_POINT('Ctrl Pts',(3.96192990160296,-1.,-0.167730547023312));
#44364=CARTESIAN_POINT('Ctrl Pts',(3.9691931362141,-1.,-0.165598992851098));
#44365=CARTESIAN_POINT('Ctrl Pts',(3.97645194630944,-1.,-0.163422004609999));
#44366=CARTESIAN_POINT('Ctrl Pts',(3.98371010319866,-1.,-0.161200482186088));
#44367=CARTESIAN_POINT('Ctrl Pts',(3.99096873945862,-1.,-0.158935123982796));
#44368=CARTESIAN_POINT('Ctrl Pts',(3.99822717425869,-1.,-0.156626481393736));
#44369=CARTESIAN_POINT('Ctrl Pts',(4.00548360245297,-1.,-0.15427500487231));
#44370=CARTESIAN_POINT('Ctrl Pts',(4.01273584234684,-1.,-0.151881094022909));
#44371=CARTESIAN_POINT('Ctrl Pts',(4.01998203715588,-1.,-0.149445144968708));
#44372=CARTESIAN_POINT('Ctrl Pts',(4.02722143147048,-1.,-0.146967602878999));
#44373=CARTESIAN_POINT('Ctrl Pts',(4.03445411510403,-1.,-0.144448947038352));
#44374=CARTESIAN_POINT('Ctrl Pts',(4.04168069633842,-1.,-0.141889671485508));
#44375=CARTESIAN_POINT('Ctrl Pts',(4.04890199238056,-1.,-0.13929026718006));
#44376=CARTESIAN_POINT('Ctrl Pts',(4.05611873400122,-1.,-0.136651205046111));
#44377=CARTESIAN_POINT('Ctrl Pts',(4.06333121018476,-1.,-0.133972916144225));
#44378=CARTESIAN_POINT('Ctrl Pts',(4.07053931528579,-1.,-0.131255793548914));
#44379=CARTESIAN_POINT('Ctrl Pts',(4.07774270738809,-1.,-0.128500200484814));
#44380=CARTESIAN_POINT('Ctrl Pts',(4.08494093372315,-1.,-0.12570647682253));
#44381=CARTESIAN_POINT('Ctrl Pts',(4.09213355850836,-1.,-0.122874946249119));
#44382=CARTESIAN_POINT('Ctrl Pts',(4.09932031767243,-1.,-0.120005924388162));
#44383=CARTESIAN_POINT('Ctrl Pts',(4.10650113382187,-1.,-0.117099722731705));
#44384=CARTESIAN_POINT('Ctrl Pts',(4.11367603925313,-1.,-0.114156649609602));
#44385=CARTESIAN_POINT('Ctrl Pts',(4.12084512502444,-1.,-0.111177012683378));
#44386=CARTESIAN_POINT('Ctrl Pts',(4.12800848371386,-1.,-0.10816112052835));
#44387=CARTESIAN_POINT('Ctrl Pts',(4.13516614458396,-1.,-0.105109286538864));
#44388=CARTESIAN_POINT('Ctrl Pts',(4.14231804938737,-1.,-0.102021826577454));
#44389=CARTESIAN_POINT('Ctrl Pts',(4.1494640891762,-1.,-0.0988990478899816));
#44390=CARTESIAN_POINT('Ctrl Pts',(4.15660412653006,-1.,-0.0957412403297072));
#44391=CARTESIAN_POINT('Ctrl Pts',(4.16373802265942,-1.,-0.0925486672167695));
#44392=CARTESIAN_POINT('Ctrl Pts',(4.17086566491823,-1.,-0.0893215560850332));
#44393=CARTESIAN_POINT('Ctrl Pts',(4.17798698669991,-1.,-0.086060091555252));
#44394=CARTESIAN_POINT('Ctrl Pts',(4.1851019532944,-1.,-0.0827644164389515));
#44395=CARTESIAN_POINT('Ctrl Pts',(4.19078883322483,-1.,-0.0801005887117608));
#44396=CARTESIAN_POINT('Ctrl Pts',(4.19505112860624,-1.,-0.0780873956244407));
#44397=CARTESIAN_POINT('Ctrl Pts',(4.19789138621624,-1.,-0.07673845961422));
#44398=CARTESIAN_POINT('Ctrl Pts',(4.19931119685982,-1.,-0.0760622897878241));
#44399=CARTESIAN_POINT('',(4.19931119685982,-1.,0.0760622897878241));
#44400=CARTESIAN_POINT('',(4.19931119685982,-1.,-0.0760622897878241));
#44401=CARTESIAN_POINT('',(3.74449296983004,-1.,0.2031560948961));
#44402=CARTESIAN_POINT('Ctrl Pts',(4.19931119685982,-1.,0.0760622897878241));
#44403=CARTESIAN_POINT('Ctrl Pts',(4.1978913862118,-1.,0.0767384596141459));
#44404=CARTESIAN_POINT('Ctrl Pts',(4.19505112859416,-1.,0.0780873956242392));
#44405=CARTESIAN_POINT('Ctrl Pts',(4.19078883320504,-1.,0.0801005887114315));
#44406=CARTESIAN_POINT('Ctrl Pts',(4.18510195327123,-1.,0.0827644164385674));
#44407=CARTESIAN_POINT('Ctrl Pts',(4.17798698668094,-1.,0.0860600915549391));
#44408=CARTESIAN_POINT('Ctrl Pts',(4.17086566490794,-1.,0.0893215560848644));
#44409=CARTESIAN_POINT('Ctrl Pts',(4.16373802265839,-1.,0.0925486672167526));
#44410=CARTESIAN_POINT('Ctrl Pts',(4.15660412653577,-1.,0.0957412403298002));
#44411=CARTESIAN_POINT('Ctrl Pts',(4.14946408918485,-1.,0.0988990478901221));
#44412=CARTESIAN_POINT('Ctrl Pts',(4.14231804939538,-1.,0.102021826577583));
#44413=CARTESIAN_POINT('Ctrl Pts',(4.13516614458895,-1.,0.105109286538945));
#44414=CARTESIAN_POINT('Ctrl Pts',(4.12800848371504,-1.,0.108161120528369));
#44415=CARTESIAN_POINT('Ctrl Pts',(4.1208451250225,-1.,0.111177012683346));
#44416=CARTESIAN_POINT('Ctrl Pts',(4.11367603924961,-1.,0.114156649609545));
#44417=CARTESIAN_POINT('Ctrl Pts',(4.10650113381833,-1.,0.117099722731648));
#44418=CARTESIAN_POINT('Ctrl Pts',(4.09932031767002,-1.,0.120005924388124));
#44419=CARTESIAN_POINT('Ctrl Pts',(4.09213355850756,-1.,0.122874946249106));
#44420=CARTESIAN_POINT('Ctrl Pts',(4.08494093372377,-1.,0.125706476822539));
#44421=CARTESIAN_POINT('Ctrl Pts',(4.07774270738954,-1.,0.128500200484837));
#44422=CARTESIAN_POINT('Ctrl Pts',(4.0705393152874,-1.,0.13125579354894));
#44423=CARTESIAN_POINT('Ctrl Pts',(4.06333121018596,-1.,0.133972916144244));
#44424=CARTESIAN_POINT('Ctrl Pts',(4.05611873400172,-1.,0.136651205046119));
#44425=CARTESIAN_POINT('Ctrl Pts',(4.04890199238036,-1.,0.139290267180057));
#44426=CARTESIAN_POINT('Ctrl Pts',(4.04168069633781,-1.,0.1418896714855));
#44427=CARTESIAN_POINT('Ctrl Pts',(4.03445411510333,-1.,0.144448947038344));
#44428=CARTESIAN_POINT('Ctrl Pts',(4.02722143146994,-1.,0.146967602878994));
#44429=CARTESIAN_POINT('Ctrl Pts',(4.01998203715564,-1.,0.149445144968706));
#44430=CARTESIAN_POINT('Ctrl Pts',(4.01273584234689,-1.,0.15188109402291));
#44431=CARTESIAN_POINT('Ctrl Pts',(4.00548360245319,-1.,0.15427500487231));
#44432=CARTESIAN_POINT('Ctrl Pts',(3.99822717425893,-1.,0.156626481393734));
#44433=CARTESIAN_POINT('Ctrl Pts',(3.99096873945878,-1.,0.158935123982793));
#44434=CARTESIAN_POINT('Ctrl Pts',(3.98371010319872,-1.,0.161200482186084));
#44435=CARTESIAN_POINT('Ctrl Pts',(3.97645194630943,-1.,0.163422004609999));
#44436=CARTESIAN_POINT('Ctrl Pts',(3.96919313621407,-1.,0.165598992851102));
#44437=CARTESIAN_POINT('Ctrl Pts',(3.96192990160296,-1.,0.167730547023319));
#44438=CARTESIAN_POINT('Ctrl Pts',(3.95465744665268,-1.,0.169815666374138));
#44439=CARTESIAN_POINT('Ctrl Pts',(3.94737164900868,-1.,0.17185335536924));
#44440=CARTESIAN_POINT('Ctrl Pts',(3.94007083096217,-1.,0.173842734974609));
#44441=CARTESIAN_POINT('Ctrl Pts',(3.93275726771042,-1.,0.175783136893867));
#44442=CARTESIAN_POINT('Ctrl Pts',(3.92543942697655,-1.,0.177674246152317));
#44443=CARTESIAN_POINT('Ctrl Pts',(3.91812876180926,-1.,0.179515885822881));
#44444=CARTESIAN_POINT('Ctrl Pts',(3.91083557557175,-1.,0.181307740731785));
#44445=CARTESIAN_POINT('Ctrl Pts',(3.90356488555132,-1.,0.18304908199319));
#44446=CARTESIAN_POINT('Ctrl Pts',(3.89631300742646,-1.,0.184738537728042));
#44447=CARTESIAN_POINT('Ctrl Pts',(3.88906196725848,-1.,0.18637372498528));
#44448=CARTESIAN_POINT('Ctrl Pts',(3.88178563496228,-1.,0.187951632512684));
#44449=CARTESIAN_POINT('Ctrl Pts',(3.87445976418412,-1.,0.189469253358272));
#44450=CARTESIAN_POINT('Ctrl Pts',(3.86707158624783,-1.,0.190924190418619));
#44451=CARTESIAN_POINT('Ctrl Pts',(3.85962774407633,-1.,0.19231515304497));
#44452=CARTESIAN_POINT('Ctrl Pts',(3.85216762263966,-1.,0.193642806777722));
#44453=CARTESIAN_POINT('Ctrl Pts',(3.84475203346977,-1.,0.19490900946022));
#44454=CARTESIAN_POINT('Ctrl Pts',(3.83743910616195,-1.,0.196115198971858));
#44455=CARTESIAN_POINT('Ctrl Pts',(3.83026221776456,-1.,0.197260935827361));
#44456=CARTESIAN_POINT('Ctrl Pts',(3.82321127349016,-1.,0.198342616900486));
#44457=CARTESIAN_POINT('Ctrl Pts',(3.81620203429815,-1.,0.199351525297447));
#44458=CARTESIAN_POINT('Ctrl Pts',(3.80909529318669,-1.,0.200274679433364));
#44459=CARTESIAN_POINT('Ctrl Pts',(3.80175247447337,-1.,0.201097756307325));
#44460=CARTESIAN_POINT('Ctrl Pts',(3.7940835418736,-1.,0.201807533800837));
#44461=CARTESIAN_POINT('Ctrl Pts',(3.78609175019242,-1.,0.20239426051216));
#44462=CARTESIAN_POINT('Ctrl Pts',(3.77793553476614,-1.,0.20285472969908));
#44463=CARTESIAN_POINT('Ctrl Pts',(3.7699207159487,-1.,0.203192390045164));
#44464=CARTESIAN_POINT('Ctrl Pts',(3.76242717936885,-1.,0.203414634707478));
#44465=CARTESIAN_POINT('Ctrl Pts',(3.75585118707734,-1.,0.203530796848321));
#44466=CARTESIAN_POINT('Ctrl Pts',(3.75054693397875,-1.,0.203550035479166));
#44467=CARTESIAN_POINT('Ctrl Pts',(3.74703926501752,-1.,0.203484186269415));
#44468=CARTESIAN_POINT('Ctrl Pts',(3.74535749969115,-1.,0.203375226874121));
#44469=CARTESIAN_POINT('Ctrl Pts',(3.74471097893845,-1.,0.20326661011053));
#44470=CARTESIAN_POINT('Ctrl Pts',(3.74453008995092,-1.,0.203188003946656));
#44471=CARTESIAN_POINT('Ctrl Pts',(3.74449296983004,-1.,0.2031560948961));
#44472=CARTESIAN_POINT('',(3.73017266276651,-1.,0.385112848330762));
#44473=CARTESIAN_POINT('Origin',(0.,-1.,0.));
#44474=CARTESIAN_POINT('',(4.15950947128175,-1.,0.581791163835816));
#44475=CARTESIAN_POINT('Ctrl Pts',(3.73017266276651,-1.,0.385112848330762));
#44476=CARTESIAN_POINT('Ctrl Pts',(3.73021431755274,-1.,0.385087139000375));
#44477=CARTESIAN_POINT('Ctrl Pts',(3.73040527621055,-1.,0.385037797881504));
#44478=CARTESIAN_POINT('Ctrl Pts',(3.73106082862548,-1.,0.385031656499164));
#44479=CARTESIAN_POINT('Ctrl Pts',(3.73273893363406,-1.,0.385187124634207));
#44480=CARTESIAN_POINT('Ctrl Pts',(3.73621371845318,-1.,0.385670806454566));
#44481=CARTESIAN_POINT('Ctrl Pts',(3.74144965781276,-1.,0.386519576222252));
#44482=CARTESIAN_POINT('Ctrl Pts',(3.74792651696654,-1.,0.387663020050836));
#44483=CARTESIAN_POINT('Ctrl Pts',(3.75529302895152,-1.,0.389054775898702));
#44484=CARTESIAN_POINT('Ctrl Pts',(3.76315635033257,-1.,0.39064207297956));
#44485=CARTESIAN_POINT('Ctrl Pts',(3.77114011595967,-1.,0.392372786223433));
#44486=CARTESIAN_POINT('Ctrl Pts',(3.77894173114283,-1.,0.3942024810115));
#44487=CARTESIAN_POINT('Ctrl Pts',(3.78640521279313,-1.,0.396103205334841));
#44488=CARTESIAN_POINT('Ctrl Pts',(3.7935288716329,-1.,0.39806481868397));
#44489=CARTESIAN_POINT('Ctrl Pts',(3.80040370384546,-1.,0.400088346504601));
#44490=CARTESIAN_POINT('Ctrl Pts',(3.80716881962728,-1.,0.402181320148436));
#44491=CARTESIAN_POINT('Ctrl Pts',(3.81396374287793,-1.,0.404352694628274));
#44492=CARTESIAN_POINT('Ctrl Pts',(3.8208730391381,-1.,0.406607038258986));
#44493=CARTESIAN_POINT('Ctrl Pts',(3.82790724256471,-1.,0.40894237144746));
#44494=CARTESIAN_POINT('Ctrl Pts',(3.83503345578698,-1.,0.411353038798519));
#44495=CARTESIAN_POINT('Ctrl Pts',(3.84219403994762,-1.,0.413831367016748));
#44496=CARTESIAN_POINT('Ctrl Pts',(3.84932864157497,-1.,0.416369678052907));
#44497=CARTESIAN_POINT('Ctrl Pts',(3.85639825647996,-1.,0.418962468086773));
#44498=CARTESIAN_POINT('Ctrl Pts',(3.86339652542709,-1.,0.421607423177534));
#44499=CARTESIAN_POINT('Ctrl Pts',(3.87033643487851,-1.,0.424304173195111));
#44500=CARTESIAN_POINT('Ctrl Pts',(3.87724240306597,-1.,0.427053541173458));
#44501=CARTESIAN_POINT('Ctrl Pts',(3.88414070943341,-1.,0.429856640579741));
#44502=CARTESIAN_POINT('Ctrl Pts',(3.89104947940611,-1.,0.432713929544459));
#44503=CARTESIAN_POINT('Ctrl Pts',(3.89797256655462,-1.,0.435624629433528));
#44504=CARTESIAN_POINT('Ctrl Pts',(3.90490512938563,-1.,0.43858723545825));
#44505=CARTESIAN_POINT('Ctrl Pts',(3.91183704069153,-1.,0.441599824524055));
#44506=CARTESIAN_POINT('Ctrl Pts',(3.91875701610719,-1.,0.444660430230591));
#44507=CARTESIAN_POINT('Ctrl Pts',(3.92565674143416,-1.,0.447767416837293));
#44508=CARTESIAN_POINT('Ctrl Pts',(3.93253407403123,-1.,0.450919768356349));
#44509=CARTESIAN_POINT('Ctrl Pts',(3.93939080846298,-1.,0.454116879027584));
#44510=CARTESIAN_POINT('Ctrl Pts',(3.94623117206678,-1.,0.457358410451683));
#44511=CARTESIAN_POINT('Ctrl Pts',(3.95306005817364,-1.,0.460644124429122));
#44512=CARTESIAN_POINT('Ctrl Pts',(3.95988133243538,-1.,0.463973722115734));
#44513=CARTESIAN_POINT('Ctrl Pts',(3.9666962227393,-1.,0.467346690880644));
#44514=CARTESIAN_POINT('Ctrl Pts',(3.97350414289392,-1.,0.47076237961344));
#44515=CARTESIAN_POINT('Ctrl Pts',(3.98030338044409,-1.,0.47422006101951));
#44516=CARTESIAN_POINT('Ctrl Pts',(3.98709184306738,-1.,0.477718999122028));
#44517=CARTESIAN_POINT('Ctrl Pts',(3.99386775880679,-1.,0.481258512209676));
#44518=CARTESIAN_POINT('Ctrl Pts',(4.00063045119288,-1.,0.484838042421835));
#44519=CARTESIAN_POINT('Ctrl Pts',(4.0073800839099,-1.,0.488457130424634));
#44520=CARTESIAN_POINT('Ctrl Pts',(4.01411733503546,-1.,0.492115383418019));
#44521=CARTESIAN_POINT('Ctrl Pts',(4.02084308851832,-1.,0.495812444326251));
#44522=CARTESIAN_POINT('Ctrl Pts',(4.02755813980101,-1.,0.499547962340822));
#44523=CARTESIAN_POINT('Ctrl Pts',(4.03426284174272,-1.,0.503321556915346));
#44524=CARTESIAN_POINT('Ctrl Pts',(4.04095715148915,-1.,0.507132823288137));
#44525=CARTESIAN_POINT('Ctrl Pts',(4.04764078815447,-1.,0.510981349218971));
#44526=CARTESIAN_POINT('Ctrl Pts',(4.05431335771199,-1.,0.514866728193017));
#44527=CARTESIAN_POINT('Ctrl Pts',(4.06097448038013,-1.,0.518788572336924));
#44528=CARTESIAN_POINT('Ctrl Pts',(4.06762394471314,-1.,0.522746528603108));
#44529=CARTESIAN_POINT('Ctrl Pts',(4.07426172299847,-1.,0.526740277227498));
#44530=CARTESIAN_POINT('Ctrl Pts',(4.08088789536836,-1.,0.530769518728571));
#44531=CARTESIAN_POINT('Ctrl Pts',(4.08750259988885,-1.,0.534833963477273));
#44532=CARTESIAN_POINT('Ctrl Pts',(4.09410597627,-1.,0.538933321179756));
#44533=CARTESIAN_POINT('Ctrl Pts',(4.10069810243979,-1.,0.543067286877758));
#44534=CARTESIAN_POINT('Ctrl Pts',(4.10727897027977,-1.,0.547235539485637));
#44535=CARTESIAN_POINT('Ctrl Pts',(4.11384852024721,-1.,0.551437758497033));
#44536=CARTESIAN_POINT('Ctrl Pts',(4.12040666195664,-1.,0.555673636129978));
#44537=CARTESIAN_POINT('Ctrl Pts',(4.12695329951961,-1.,0.559942890594774));
#44538=CARTESIAN_POINT('Ctrl Pts',(4.13348835727104,-1.,0.564245279537149));
#44539=CARTESIAN_POINT('Ctrl Pts',(4.14001179830547,-1.,0.568580610189775));
#44540=CARTESIAN_POINT('Ctrl Pts',(4.14652361068081,-1.,0.572948736069523));
#44541=CARTESIAN_POINT('Ctrl Pts',(4.151723761217,-1.,0.576469391676689));
#44542=CARTESIAN_POINT('Ctrl Pts',(4.15561864788576,-1.,0.579124568914236));
#44543=CARTESIAN_POINT('Ctrl Pts',(4.1582129171283,-1.,0.580901211463535));
#44544=CARTESIAN_POINT('Ctrl Pts',(4.15950947128175,-1.,0.581791163835816));
#44545=CARTESIAN_POINT('',(4.13571194405636,-1.,0.732042837400621));
#44546=CARTESIAN_POINT('',(4.15950947128175,-1.,0.581791163835816));
#44547=CARTESIAN_POINT('Ctrl Pts',(4.13571194405636,-1.,0.732042837400621));
#44548=CARTESIAN_POINT('Ctrl Pts',(4.1342038373684,-1.,0.73248857513516));
#44549=CARTESIAN_POINT('Ctrl Pts',(4.13118752795207,-1.,0.733376589323547));
#44550=CARTESIAN_POINT('Ctrl Pts',(4.12666277570844,-1.,0.734698226764093));
#44551=CARTESIAN_POINT('Ctrl Pts',(4.120629196238,-1.,0.736439634331345));
#44552=CARTESIAN_POINT('Ctrl Pts',(4.11308626951927,-1.,0.738581708225844));
#44553=CARTESIAN_POINT('Ctrl Pts',(4.10554241757547,-1.,0.740688998553377));
#44554=CARTESIAN_POINT('Ctrl Pts',(4.09799769702611,-1.,0.742761369689842));
#44555=CARTESIAN_POINT('Ctrl Pts',(4.09045220253573,-1.,0.744798649706501));
#44556=CARTESIAN_POINT('Ctrl Pts',(4.08290608095642,-1.,0.746800631492316));
#44557=CARTESIAN_POINT('Ctrl Pts',(4.07535951056152,-1.,0.748767076680558));
#44558=CARTESIAN_POINT('Ctrl Pts',(4.06781267242378,-1.,0.750697720484037));
#44559=CARTESIAN_POINT('Ctrl Pts',(4.06026572221515,-1.,0.752592276483073));
#44560=CARTESIAN_POINT('Ctrl Pts',(4.05271876687915,-1.,0.754450441816078));
#44561=CARTESIAN_POINT('Ctrl Pts',(4.04517182653997,-1.,0.756271902369581));
#44562=CARTESIAN_POINT('Ctrl Pts',(4.03762485803119,-1.,0.758056338884945));
#44563=CARTESIAN_POINT('Ctrl Pts',(4.03007781954412,-1.,0.759803433243752));
#44564=CARTESIAN_POINT('Ctrl Pts',(4.02253072741268,-1.,0.761512875859805));
#44565=CARTESIAN_POINT('Ctrl Pts',(4.01498370680496,-1.,0.763184371182936));
#44566=CARTESIAN_POINT('Ctrl Pts',(4.00743706791509,-1.,0.764817648785198));
#44567=CARTESIAN_POINT('Ctrl Pts',(3.99989129179622,-1.,0.766412457136064));
#44568=CARTESIAN_POINT('Ctrl Pts',(3.9923468788101,-1.,0.767968531377915));
#44569=CARTESIAN_POINT('Ctrl Pts',(3.98480422348451,-1.,0.769485566245545));
#44570=CARTESIAN_POINT('Ctrl Pts',(3.97726349165488,-1.,0.770963190030471));
#44571=CARTESIAN_POINT('Ctrl Pts',(3.96972446532772,-1.,0.772400931772137));
#44572=CARTESIAN_POINT('Ctrl Pts',(3.96218649639807,-1.,0.773798212026566));
#44573=CARTESIAN_POINT('Ctrl Pts',(3.9546488545231,-1.,0.775154418039352));
#44574=CARTESIAN_POINT('Ctrl Pts',(3.94711101619447,-1.,0.776468966697922));
#44575=CARTESIAN_POINT('Ctrl Pts',(3.93957296768103,-1.,0.777741370568559));
#44576=CARTESIAN_POINT('Ctrl Pts',(3.93203552473174,-1.,0.778971308134821));
#44577=CARTESIAN_POINT('Ctrl Pts',(3.92450058323823,-1.,0.780158678615543));
#44578=CARTESIAN_POINT('Ctrl Pts',(3.91697036054676,-1.,0.781303428618367));
#44579=CARTESIAN_POINT('Ctrl Pts',(3.90944671004542,-1.,0.782405395622765));
#44580=CARTESIAN_POINT('Ctrl Pts',(3.9019303904397,-1.,0.783464141529082));
#44581=CARTESIAN_POINT('Ctrl Pts',(3.89442039235103,-1.,0.784478799358337));
#44582=CARTESIAN_POINT('Ctrl Pts',(3.88691313167398,-1.,0.785447890340731));
#44583=CARTESIAN_POINT('Ctrl Pts',(3.8794040281819,-1.,0.786369675812609));
#44584=CARTESIAN_POINT('Ctrl Pts',(3.87188916600912,-1.,0.787242527617999));
#44585=CARTESIAN_POINT('Ctrl Pts',(3.86436702561345,-1.,0.788065315093778));
#44586=CARTESIAN_POINT('Ctrl Pts',(3.85683995872529,-1.,0.788837734090672));
#44587=CARTESIAN_POINT('Ctrl Pts',(3.84931637808894,-1.,0.789560798155583));
#44588=CARTESIAN_POINT('Ctrl Pts',(3.84180762342454,-1.,0.790236124191243));
#44589=CARTESIAN_POINT('Ctrl Pts',(3.83432392054786,-1.,0.790865012705301));
#44590=CARTESIAN_POINT('Ctrl Pts',(3.82687033899792,-1.,0.791447528662369));
#44591=CARTESIAN_POINT('Ctrl Pts',(3.81944345442249,-1.,0.791981740718635));
#44592=CARTESIAN_POINT('Ctrl Pts',(3.81202588694756,-1.,0.792462483517635));
#44593=CARTESIAN_POINT('Ctrl Pts',(3.80459229925637,-1.,0.792882695234778));
#44594=CARTESIAN_POINT('Ctrl Pts',(3.79711921389897,-1.,0.793235612973274));
#44595=CARTESIAN_POINT('Ctrl Pts',(3.78959439439235,-1.,0.793516871680994));
#44596=CARTESIAN_POINT('Ctrl Pts',(3.78202460377598,-1.,0.793726235781301));
#44597=CARTESIAN_POINT('Ctrl Pts',(3.77444863801212,-1.,0.793870523787408));
#44598=CARTESIAN_POINT('Ctrl Pts',(3.76692626931111,-1.,0.793961083688992));
#44599=CARTESIAN_POINT('Ctrl Pts',(3.75951468666257,-1.,0.794008429134908));
#44600=CARTESIAN_POINT('Ctrl Pts',(3.75224692493864,-1.,0.794017347371378));
#44601=CARTESIAN_POINT('Ctrl Pts',(3.74511357728861,-1.,0.793982700459952));
#44602=CARTESIAN_POINT('Ctrl Pts',(3.73803280541687,-1.,0.793882700937017));
#44603=CARTESIAN_POINT('Ctrl Pts',(3.73086914695805,-1.,0.793682750269684));
#44604=CARTESIAN_POINT('Ctrl Pts',(3.72348797293734,-1.,0.793347023784205));
#44605=CARTESIAN_POINT('Ctrl Pts',(3.71580242396124,-1.,0.792848377370287));
#44606=CARTESIAN_POINT('Ctrl Pts',(3.70781724021806,-1.,0.792177688845818));
#44607=CARTESIAN_POINT('Ctrl Pts',(3.69968940808721,-1.,0.79135657569598));
#44608=CARTESIAN_POINT('Ctrl Pts',(3.69172044327364,-1.,0.790436284988788));
#44609=CARTESIAN_POINT('Ctrl Pts',(3.68428439783905,-1.,0.789483546064387));
#44610=CARTESIAN_POINT('Ctrl Pts',(3.67777119516252,-1.,0.788569566220286));
#44611=CARTESIAN_POINT('Ctrl Pts',(3.67252923663655,-1.,0.787758799995743));
#44612=CARTESIAN_POINT('Ctrl Pts',(3.66907505398677,-1.,0.787145041181546));
#44613=CARTESIAN_POINT('Ctrl Pts',(3.66743103898702,-1.,0.786774337198063));
#44614=CARTESIAN_POINT('Ctrl Pts',(3.66680946938292,-1.,0.786565919558984));
#44615=CARTESIAN_POINT('Ctrl Pts',(3.6666431041522,-1.,0.786459983895432));
#44616=CARTESIAN_POINT('Ctrl Pts',(3.66661143271685,-1.,0.786422660831985));
#44617=CARTESIAN_POINT('Origin',(0.,-1.,0.));
#44618=CARTESIAN_POINT('Origin',(0.,0.,0.));
#44619=CARTESIAN_POINT('Origin',(0.,2.2,0.));
#44620=CARTESIAN_POINT('Origin',(0.,1.,0.));
#44621=CARTESIAN_POINT('',(-2.,2.2,2.44929359829471E-16));
#44622=CARTESIAN_POINT('Origin',(0.,2.2,0.));
#44623=CARTESIAN_POINT('',(-2.,1.,2.44929359829471E-16));
#44624=CARTESIAN_POINT('',(-2.,1.,2.44929359829471E-16));
#44625=CARTESIAN_POINT('Origin',(0.,1.,0.));
#44626=CARTESIAN_POINT('Origin',(0.,2.2,0.));
#44627=CARTESIAN_POINT('Ctrl Pts',(4.15950947128175,-1.,0.581791163835816));
#44628=CARTESIAN_POINT('Ctrl Pts',(4.15950947128175,1.,0.581791163835816));
#44629=CARTESIAN_POINT('Ctrl Pts',(4.1582129171283,-1.,0.580901211463535));
#44630=CARTESIAN_POINT('Ctrl Pts',(4.1582129171283,1.,0.580901211463535));
#44631=CARTESIAN_POINT('Ctrl Pts',(4.15561864788576,-1.,0.579124568914236));
#44632=CARTESIAN_POINT('Ctrl Pts',(4.15561864788576,1.,0.579124568914236));
#44633=CARTESIAN_POINT('Ctrl Pts',(4.151723761217,-1.,0.576469391676689));
#44634=CARTESIAN_POINT('Ctrl Pts',(4.151723761217,1.,0.576469391676689));
#44635=CARTESIAN_POINT('Ctrl Pts',(4.14652361068081,-1.,0.572948736069523));
#44636=CARTESIAN_POINT('Ctrl Pts',(4.14652361068081,1.,0.572948736069523));
#44637=CARTESIAN_POINT('Ctrl Pts',(4.14001179830547,-1.,0.568580610189775));
#44638=CARTESIAN_POINT('Ctrl Pts',(4.14001179830547,1.,0.568580610189775));
#44639=CARTESIAN_POINT('Ctrl Pts',(4.13348835727104,-1.,0.564245279537149));
#44640=CARTESIAN_POINT('Ctrl Pts',(4.13348835727104,1.,0.564245279537149));
#44641=CARTESIAN_POINT('Ctrl Pts',(4.12695329951961,-1.,0.559942890594774));
#44642=CARTESIAN_POINT('Ctrl Pts',(4.12695329951961,1.,0.559942890594774));
#44643=CARTESIAN_POINT('Ctrl Pts',(4.12040666195664,-1.,0.555673636129978));
#44644=CARTESIAN_POINT('Ctrl Pts',(4.12040666195664,1.,0.555673636129978));
#44645=CARTESIAN_POINT('Ctrl Pts',(4.11384852024721,-1.,0.551437758497033));
#44646=CARTESIAN_POINT('Ctrl Pts',(4.11384852024721,1.,0.551437758497033));
#44647=CARTESIAN_POINT('Ctrl Pts',(4.10727897027977,-1.,0.547235539485637));
#44648=CARTESIAN_POINT('Ctrl Pts',(4.10727897027977,1.,0.547235539485637));
#44649=CARTESIAN_POINT('Ctrl Pts',(4.10069810243979,-1.,0.543067286877758));
#44650=CARTESIAN_POINT('Ctrl Pts',(4.10069810243979,1.,0.543067286877758));
#44651=CARTESIAN_POINT('Ctrl Pts',(4.09410597627,-1.,0.538933321179756));
#44652=CARTESIAN_POINT('Ctrl Pts',(4.09410597627,1.,0.538933321179756));
#44653=CARTESIAN_POINT('Ctrl Pts',(4.08750259988885,-1.,0.534833963477273));
#44654=CARTESIAN_POINT('Ctrl Pts',(4.08750259988885,1.,0.534833963477273));
#44655=CARTESIAN_POINT('Ctrl Pts',(4.08088789536836,-1.,0.530769518728571));
#44656=CARTESIAN_POINT('Ctrl Pts',(4.08088789536836,1.,0.530769518728571));
#44657=CARTESIAN_POINT('Ctrl Pts',(4.07426172299847,-1.,0.526740277227498));
#44658=CARTESIAN_POINT('Ctrl Pts',(4.07426172299847,1.,0.526740277227498));
#44659=CARTESIAN_POINT('Ctrl Pts',(4.06762394471314,-1.,0.522746528603108));
#44660=CARTESIAN_POINT('Ctrl Pts',(4.06762394471314,1.,0.522746528603108));
#44661=CARTESIAN_POINT('Ctrl Pts',(4.06097448038013,-1.,0.518788572336924));
#44662=CARTESIAN_POINT('Ctrl Pts',(4.06097448038013,1.,0.518788572336924));
#44663=CARTESIAN_POINT('Ctrl Pts',(4.05431335771199,-1.,0.514866728193017));
#44664=CARTESIAN_POINT('Ctrl Pts',(4.05431335771199,1.,0.514866728193017));
#44665=CARTESIAN_POINT('Ctrl Pts',(4.04764078815447,-1.,0.510981349218971));
#44666=CARTESIAN_POINT('Ctrl Pts',(4.04764078815447,1.,0.510981349218971));
#44667=CARTESIAN_POINT('Ctrl Pts',(4.04095715148915,-1.,0.507132823288137));
#44668=CARTESIAN_POINT('Ctrl Pts',(4.04095715148915,1.,0.507132823288137));
#44669=CARTESIAN_POINT('Ctrl Pts',(4.03426284174272,-1.,0.503321556915346));
#44670=CARTESIAN_POINT('Ctrl Pts',(4.03426284174272,1.,0.503321556915346));
#44671=CARTESIAN_POINT('Ctrl Pts',(4.02755813980101,-1.,0.499547962340822));
#44672=CARTESIAN_POINT('Ctrl Pts',(4.02755813980101,1.,0.499547962340822));
#44673=CARTESIAN_POINT('Ctrl Pts',(4.02084308851832,-1.,0.495812444326251));
#44674=CARTESIAN_POINT('Ctrl Pts',(4.02084308851832,1.,0.495812444326251));
#44675=CARTESIAN_POINT('Ctrl Pts',(4.01411733503546,-1.,0.492115383418019));
#44676=CARTESIAN_POINT('Ctrl Pts',(4.01411733503546,1.,0.492115383418019));
#44677=CARTESIAN_POINT('Ctrl Pts',(4.0073800839099,-1.,0.488457130424634));
#44678=CARTESIAN_POINT('Ctrl Pts',(4.0073800839099,1.,0.488457130424634));
#44679=CARTESIAN_POINT('Ctrl Pts',(4.00063045119288,-1.,0.484838042421835));
#44680=CARTESIAN_POINT('Ctrl Pts',(4.00063045119288,1.,0.484838042421835));
#44681=CARTESIAN_POINT('Ctrl Pts',(3.99386775880679,-1.,0.481258512209676));
#44682=CARTESIAN_POINT('Ctrl Pts',(3.99386775880679,1.,0.481258512209676));
#44683=CARTESIAN_POINT('Ctrl Pts',(3.98709184306738,-1.,0.477718999122028));
#44684=CARTESIAN_POINT('Ctrl Pts',(3.98709184306738,1.,0.477718999122028));
#44685=CARTESIAN_POINT('Ctrl Pts',(3.98030338044409,-1.,0.47422006101951));
#44686=CARTESIAN_POINT('Ctrl Pts',(3.98030338044409,1.,0.47422006101951));
#44687=CARTESIAN_POINT('Ctrl Pts',(3.97350414289392,-1.,0.47076237961344));
#44688=CARTESIAN_POINT('Ctrl Pts',(3.97350414289392,1.,0.47076237961344));
#44689=CARTESIAN_POINT('Ctrl Pts',(3.9666962227393,-1.,0.467346690880644));
#44690=CARTESIAN_POINT('Ctrl Pts',(3.9666962227393,1.,0.467346690880644));
#44691=CARTESIAN_POINT('Ctrl Pts',(3.95988133243538,-1.,0.463973722115734));
#44692=CARTESIAN_POINT('Ctrl Pts',(3.95988133243538,1.,0.463973722115734));
#44693=CARTESIAN_POINT('Ctrl Pts',(3.95306005817364,-1.,0.460644124429122));
#44694=CARTESIAN_POINT('Ctrl Pts',(3.95306005817364,1.,0.460644124429122));
#44695=CARTESIAN_POINT('Ctrl Pts',(3.94623117206678,-1.,0.457358410451683));
#44696=CARTESIAN_POINT('Ctrl Pts',(3.94623117206678,1.,0.457358410451683));
#44697=CARTESIAN_POINT('Ctrl Pts',(3.93939080846298,-1.,0.454116879027584));
#44698=CARTESIAN_POINT('Ctrl Pts',(3.93939080846298,1.,0.454116879027584));
#44699=CARTESIAN_POINT('Ctrl Pts',(3.93253407403123,-1.,0.450919768356349));
#44700=CARTESIAN_POINT('Ctrl Pts',(3.93253407403123,1.,0.450919768356349));
#44701=CARTESIAN_POINT('Ctrl Pts',(3.92565674143416,-1.,0.447767416837293));
#44702=CARTESIAN_POINT('Ctrl Pts',(3.92565674143416,1.,0.447767416837293));
#44703=CARTESIAN_POINT('Ctrl Pts',(3.91875701610719,-1.,0.444660430230591));
#44704=CARTESIAN_POINT('Ctrl Pts',(3.91875701610719,1.,0.444660430230591));
#44705=CARTESIAN_POINT('Ctrl Pts',(3.91183704069153,-1.,0.441599824524055));
#44706=CARTESIAN_POINT('Ctrl Pts',(3.91183704069153,1.,0.441599824524055));
#44707=CARTESIAN_POINT('Ctrl Pts',(3.90490512938563,-1.,0.43858723545825));
#44708=CARTESIAN_POINT('Ctrl Pts',(3.90490512938563,1.,0.43858723545825));
#44709=CARTESIAN_POINT('Ctrl Pts',(3.89797256655462,-1.,0.435624629433528));
#44710=CARTESIAN_POINT('Ctrl Pts',(3.89797256655462,1.,0.435624629433528));
#44711=CARTESIAN_POINT('Ctrl Pts',(3.89104947940611,-1.,0.432713929544459));
#44712=CARTESIAN_POINT('Ctrl Pts',(3.89104947940611,1.,0.432713929544459));
#44713=CARTESIAN_POINT('Ctrl Pts',(3.88414070943341,-1.,0.429856640579741));
#44714=CARTESIAN_POINT('Ctrl Pts',(3.88414070943341,1.,0.429856640579741));
#44715=CARTESIAN_POINT('Ctrl Pts',(3.87724240306597,-1.,0.427053541173458));
#44716=CARTESIAN_POINT('Ctrl Pts',(3.87724240306597,1.,0.427053541173458));
#44717=CARTESIAN_POINT('Ctrl Pts',(3.87033643487851,-1.,0.424304173195111));
#44718=CARTESIAN_POINT('Ctrl Pts',(3.87033643487851,1.,0.424304173195111));
#44719=CARTESIAN_POINT('Ctrl Pts',(3.86339652542709,-1.,0.421607423177534));
#44720=CARTESIAN_POINT('Ctrl Pts',(3.86339652542709,1.,0.421607423177534));
#44721=CARTESIAN_POINT('Ctrl Pts',(3.85639825647996,-1.,0.418962468086773));
#44722=CARTESIAN_POINT('Ctrl Pts',(3.85639825647996,1.,0.418962468086773));
#44723=CARTESIAN_POINT('Ctrl Pts',(3.84932864157497,-1.,0.416369678052907));
#44724=CARTESIAN_POINT('Ctrl Pts',(3.84932864157497,1.,0.416369678052907));
#44725=CARTESIAN_POINT('Ctrl Pts',(3.84219403994762,-1.,0.413831367016748));
#44726=CARTESIAN_POINT('Ctrl Pts',(3.84219403994762,1.,0.413831367016748));
#44727=CARTESIAN_POINT('Ctrl Pts',(3.83503345578698,-1.,0.411353038798519));
#44728=CARTESIAN_POINT('Ctrl Pts',(3.83503345578698,1.,0.411353038798519));
#44729=CARTESIAN_POINT('Ctrl Pts',(3.82790724256471,-1.,0.40894237144746));
#44730=CARTESIAN_POINT('Ctrl Pts',(3.82790724256471,1.,0.40894237144746));
#44731=CARTESIAN_POINT('Ctrl Pts',(3.8208730391381,-1.,0.406607038258986));
#44732=CARTESIAN_POINT('Ctrl Pts',(3.8208730391381,1.,0.406607038258986));
#44733=CARTESIAN_POINT('Ctrl Pts',(3.81396374287793,-1.,0.404352694628274));
#44734=CARTESIAN_POINT('Ctrl Pts',(3.81396374287793,1.,0.404352694628274));
#44735=CARTESIAN_POINT('Ctrl Pts',(3.80716881962728,-1.,0.402181320148436));
#44736=CARTESIAN_POINT('Ctrl Pts',(3.80716881962728,1.,0.402181320148436));
#44737=CARTESIAN_POINT('Ctrl Pts',(3.80040370384546,-1.,0.400088346504601));
#44738=CARTESIAN_POINT('Ctrl Pts',(3.80040370384546,1.,0.400088346504601));
#44739=CARTESIAN_POINT('Ctrl Pts',(3.7935288716329,-1.,0.39806481868397));
#44740=CARTESIAN_POINT('Ctrl Pts',(3.7935288716329,1.,0.39806481868397));
#44741=CARTESIAN_POINT('Ctrl Pts',(3.78640521279313,-1.,0.396103205334841));
#44742=CARTESIAN_POINT('Ctrl Pts',(3.78640521279313,1.,0.396103205334841));
#44743=CARTESIAN_POINT('Ctrl Pts',(3.77894173114283,-1.,0.3942024810115));
#44744=CARTESIAN_POINT('Ctrl Pts',(3.77894173114283,1.,0.3942024810115));
#44745=CARTESIAN_POINT('Ctrl Pts',(3.77114011595967,-1.,0.392372786223433));
#44746=CARTESIAN_POINT('Ctrl Pts',(3.77114011595967,1.,0.392372786223433));
#44747=CARTESIAN_POINT('Ctrl Pts',(3.76315635033257,-1.,0.39064207297956));
#44748=CARTESIAN_POINT('Ctrl Pts',(3.76315635033257,1.,0.39064207297956));
#44749=CARTESIAN_POINT('Ctrl Pts',(3.75529302895152,-1.,0.389054775898702));
#44750=CARTESIAN_POINT('Ctrl Pts',(3.75529302895152,1.,0.389054775898702));
#44751=CARTESIAN_POINT('Ctrl Pts',(3.74792651696654,-1.,0.387663020050836));
#44752=CARTESIAN_POINT('Ctrl Pts',(3.74792651696654,1.,0.387663020050836));
#44753=CARTESIAN_POINT('Ctrl Pts',(3.74144965781276,-1.,0.386519576222252));
#44754=CARTESIAN_POINT('Ctrl Pts',(3.74144965781276,1.,0.386519576222252));
#44755=CARTESIAN_POINT('Ctrl Pts',(3.73621371845318,-1.,0.385670806454566));
#44756=CARTESIAN_POINT('Ctrl Pts',(3.73621371845318,1.,0.385670806454566));
#44757=CARTESIAN_POINT('Ctrl Pts',(3.73245705638843,-1.,0.385147887988952));
#44758=CARTESIAN_POINT('Ctrl Pts',(3.73245705638843,1.,0.385147887988952));
#44759=CARTESIAN_POINT('Ctrl Pts',(3.73072465900175,-1.,0.385001870183213));
#44760=CARTESIAN_POINT('Ctrl Pts',(3.73072465900175,1.,0.385001870183213));
#44761=CARTESIAN_POINT('Ctrl Pts',(3.73015851028356,-1.,0.385047711603463));
#44762=CARTESIAN_POINT('Ctrl Pts',(3.73015851028356,1.,0.385047711603463));
#44763=CARTESIAN_POINT('Ctrl Pts',(3.73010668803042,-1.,0.385147278814643));
#44764=CARTESIAN_POINT('Ctrl Pts',(3.73010668803042,1.,0.385147278814643));
#44765=CARTESIAN_POINT('Ctrl Pts',(3.73016218570874,-1.,0.38521431477633));
#44766=CARTESIAN_POINT('Ctrl Pts',(3.73016218570874,1.,0.38521431477633));
#44767=CARTESIAN_POINT('',(3.73017266276651,1.,0.385112848330762));
#44768=CARTESIAN_POINT('Ctrl Pts',(3.73017266276651,1.,0.385112848330762));
#44769=CARTESIAN_POINT('Ctrl Pts',(3.73017266276651,0.666666666666667,0.385112848330762));
#44770=CARTESIAN_POINT('Ctrl Pts',(3.73017266276651,0.333333333333333,0.385112848330762));
#44771=CARTESIAN_POINT('Ctrl Pts',(3.73017266276651,-0.333333333333333,
0.385112848330762));
#44772=CARTESIAN_POINT('Ctrl Pts',(3.73017266276651,-0.666666666666667,
0.385112848330763));
#44773=CARTESIAN_POINT('Ctrl Pts',(3.73017266276651,-1.,0.385112848330763));
#44774=CARTESIAN_POINT('',(4.15950947128175,1.,0.581791163835816));
#44775=CARTESIAN_POINT('Ctrl Pts',(4.15950947128175,1.,0.581791163835816));
#44776=CARTESIAN_POINT('Ctrl Pts',(4.1582129171283,1.,0.580901211463535));
#44777=CARTESIAN_POINT('Ctrl Pts',(4.15561864788576,1.,0.579124568914236));
#44778=CARTESIAN_POINT('Ctrl Pts',(4.151723761217,1.,0.576469391676689));
#44779=CARTESIAN_POINT('Ctrl Pts',(4.14652361068081,1.,0.572948736069523));
#44780=CARTESIAN_POINT('Ctrl Pts',(4.14001179830547,1.,0.568580610189775));
#44781=CARTESIAN_POINT('Ctrl Pts',(4.13348835727104,1.,0.564245279537149));
#44782=CARTESIAN_POINT('Ctrl Pts',(4.12695329951961,1.,0.559942890594774));
#44783=CARTESIAN_POINT('Ctrl Pts',(4.12040666195664,1.,0.555673636129978));
#44784=CARTESIAN_POINT('Ctrl Pts',(4.11384852024721,1.,0.551437758497033));
#44785=CARTESIAN_POINT('Ctrl Pts',(4.10727897027977,1.,0.547235539485637));
#44786=CARTESIAN_POINT('Ctrl Pts',(4.10069810243979,1.,0.543067286877758));
#44787=CARTESIAN_POINT('Ctrl Pts',(4.09410597627,1.,0.538933321179756));
#44788=CARTESIAN_POINT('Ctrl Pts',(4.08750259988885,1.,0.534833963477273));
#44789=CARTESIAN_POINT('Ctrl Pts',(4.08088789536836,1.,0.530769518728571));
#44790=CARTESIAN_POINT('Ctrl Pts',(4.07426172299847,1.,0.526740277227498));
#44791=CARTESIAN_POINT('Ctrl Pts',(4.06762394471314,1.,0.522746528603108));
#44792=CARTESIAN_POINT('Ctrl Pts',(4.06097448038013,1.,0.518788572336924));
#44793=CARTESIAN_POINT('Ctrl Pts',(4.05431335771199,1.,0.514866728193017));
#44794=CARTESIAN_POINT('Ctrl Pts',(4.04764078815447,1.,0.510981349218971));
#44795=CARTESIAN_POINT('Ctrl Pts',(4.04095715148915,1.,0.507132823288137));
#44796=CARTESIAN_POINT('Ctrl Pts',(4.03426284174272,1.,0.503321556915346));
#44797=CARTESIAN_POINT('Ctrl Pts',(4.02755813980101,1.,0.499547962340822));
#44798=CARTESIAN_POINT('Ctrl Pts',(4.02084308851832,1.,0.495812444326251));
#44799=CARTESIAN_POINT('Ctrl Pts',(4.01411733503546,1.,0.492115383418019));
#44800=CARTESIAN_POINT('Ctrl Pts',(4.0073800839099,1.,0.488457130424634));
#44801=CARTESIAN_POINT('Ctrl Pts',(4.00063045119288,1.,0.484838042421835));
#44802=CARTESIAN_POINT('Ctrl Pts',(3.99386775880679,1.,0.481258512209676));
#44803=CARTESIAN_POINT('Ctrl Pts',(3.98709184306738,1.,0.477718999122028));
#44804=CARTESIAN_POINT('Ctrl Pts',(3.98030338044409,1.,0.47422006101951));
#44805=CARTESIAN_POINT('Ctrl Pts',(3.97350414289392,1.,0.47076237961344));
#44806=CARTESIAN_POINT('Ctrl Pts',(3.9666962227393,1.,0.467346690880644));
#44807=CARTESIAN_POINT('Ctrl Pts',(3.95988133243538,1.,0.463973722115734));
#44808=CARTESIAN_POINT('Ctrl Pts',(3.95306005817364,1.,0.460644124429122));
#44809=CARTESIAN_POINT('Ctrl Pts',(3.94623117206678,1.,0.457358410451683));
#44810=CARTESIAN_POINT('Ctrl Pts',(3.93939080846298,1.,0.454116879027584));
#44811=CARTESIAN_POINT('Ctrl Pts',(3.93253407403123,1.,0.450919768356349));
#44812=CARTESIAN_POINT('Ctrl Pts',(3.92565674143416,1.,0.447767416837293));
#44813=CARTESIAN_POINT('Ctrl Pts',(3.91875701610719,1.,0.444660430230591));
#44814=CARTESIAN_POINT('Ctrl Pts',(3.91183704069153,1.,0.441599824524055));
#44815=CARTESIAN_POINT('Ctrl Pts',(3.90490512938563,1.,0.43858723545825));
#44816=CARTESIAN_POINT('Ctrl Pts',(3.89797256655462,1.,0.435624629433528));
#44817=CARTESIAN_POINT('Ctrl Pts',(3.89104947940611,1.,0.432713929544459));
#44818=CARTESIAN_POINT('Ctrl Pts',(3.88414070943341,1.,0.429856640579741));
#44819=CARTESIAN_POINT('Ctrl Pts',(3.87724240306597,1.,0.427053541173458));
#44820=CARTESIAN_POINT('Ctrl Pts',(3.87033643487851,1.,0.424304173195111));
#44821=CARTESIAN_POINT('Ctrl Pts',(3.86339652542709,1.,0.421607423177534));
#44822=CARTESIAN_POINT('Ctrl Pts',(3.85639825647996,1.,0.418962468086773));
#44823=CARTESIAN_POINT('Ctrl Pts',(3.84932864157497,1.,0.416369678052907));
#44824=CARTESIAN_POINT('Ctrl Pts',(3.84219403994762,1.,0.413831367016748));
#44825=CARTESIAN_POINT('Ctrl Pts',(3.83503345578698,1.,0.411353038798519));
#44826=CARTESIAN_POINT('Ctrl Pts',(3.82790724256471,1.,0.40894237144746));
#44827=CARTESIAN_POINT('Ctrl Pts',(3.8208730391381,1.,0.406607038258986));
#44828=CARTESIAN_POINT('Ctrl Pts',(3.81396374287793,1.,0.404352694628274));
#44829=CARTESIAN_POINT('Ctrl Pts',(3.80716881962728,1.,0.402181320148436));
#44830=CARTESIAN_POINT('Ctrl Pts',(3.80040370384546,1.,0.400088346504601));
#44831=CARTESIAN_POINT('Ctrl Pts',(3.7935288716329,1.,0.39806481868397));
#44832=CARTESIAN_POINT('Ctrl Pts',(3.78640521279313,1.,0.396103205334841));
#44833=CARTESIAN_POINT('Ctrl Pts',(3.77894173114283,1.,0.3942024810115));
#44834=CARTESIAN_POINT('Ctrl Pts',(3.77114011595967,1.,0.392372786223433));
#44835=CARTESIAN_POINT('Ctrl Pts',(3.76315635033257,1.,0.39064207297956));
#44836=CARTESIAN_POINT('Ctrl Pts',(3.75529302895152,1.,0.389054775898702));
#44837=CARTESIAN_POINT('Ctrl Pts',(3.74792651696654,1.,0.387663020050836));
#44838=CARTESIAN_POINT('Ctrl Pts',(3.74144965781276,1.,0.386519576222252));
#44839=CARTESIAN_POINT('Ctrl Pts',(3.73621371845318,1.,0.385670806454566));
#44840=CARTESIAN_POINT('Ctrl Pts',(3.73273893363406,1.,0.385187124634207));
#44841=CARTESIAN_POINT('Ctrl Pts',(3.73106082862548,1.,0.385031656499164));
#44842=CARTESIAN_POINT('Ctrl Pts',(3.73040527621055,1.,0.385037797881504));
#44843=CARTESIAN_POINT('Ctrl Pts',(3.73021431755274,1.,0.385087139000375));
#44844=CARTESIAN_POINT('Ctrl Pts',(3.73017266276651,1.,0.385112848330762));
#44845=CARTESIAN_POINT('',(4.15950947128175,0.,0.581791163835816));
#44846=CARTESIAN_POINT('Ctrl Pts',(3.66663282329846,-1.,0.7863229229206));
#44847=CARTESIAN_POINT('Ctrl Pts',(3.66663282329846,1.,0.7863229229206));
#44848=CARTESIAN_POINT('Ctrl Pts',(3.66655932661986,-1.,0.786369528183326));
#44849=CARTESIAN_POINT('Ctrl Pts',(3.66655932661986,1.,0.786369528183326));
#44850=CARTESIAN_POINT('Ctrl Pts',(3.66657784455334,-1.,0.786480236185697));
#44851=CARTESIAN_POINT('Ctrl Pts',(3.66657784455334,1.,0.786480236185697));
#44852=CARTESIAN_POINT('Ctrl Pts',(3.66710211820482,-1.,0.786698783542764));
#44853=CARTESIAN_POINT('Ctrl Pts',(3.66710211820482,1.,0.786698783542764));
#44854=CARTESIAN_POINT('Ctrl Pts',(3.66879484801113,-1.,0.787095252590501));
#44855=CARTESIAN_POINT('Ctrl Pts',(3.66879484801113,1.,0.787095252590501));
#44856=CARTESIAN_POINT('Ctrl Pts',(3.67252923663655,-1.,0.787758799995743));
#44857=CARTESIAN_POINT('Ctrl Pts',(3.67252923663655,1.,0.787758799995743));
#44858=CARTESIAN_POINT('Ctrl Pts',(3.67777119516252,-1.,0.788569566220286));
#44859=CARTESIAN_POINT('Ctrl Pts',(3.67777119516252,1.,0.788569566220286));
#44860=CARTESIAN_POINT('Ctrl Pts',(3.68428439783905,-1.,0.789483546064387));
#44861=CARTESIAN_POINT('Ctrl Pts',(3.68428439783905,1.,0.789483546064387));
#44862=CARTESIAN_POINT('Ctrl Pts',(3.69172044327364,-1.,0.790436284988788));
#44863=CARTESIAN_POINT('Ctrl Pts',(3.69172044327364,1.,0.790436284988788));
#44864=CARTESIAN_POINT('Ctrl Pts',(3.69968940808721,-1.,0.79135657569598));
#44865=CARTESIAN_POINT('Ctrl Pts',(3.69968940808721,1.,0.79135657569598));
#44866=CARTESIAN_POINT('Ctrl Pts',(3.70781724021806,-1.,0.792177688845818));
#44867=CARTESIAN_POINT('Ctrl Pts',(3.70781724021806,1.,0.792177688845818));
#44868=CARTESIAN_POINT('Ctrl Pts',(3.71580242396124,-1.,0.792848377370287));
#44869=CARTESIAN_POINT('Ctrl Pts',(3.71580242396124,1.,0.792848377370287));
#44870=CARTESIAN_POINT('Ctrl Pts',(3.72348797293734,-1.,0.793347023784205));
#44871=CARTESIAN_POINT('Ctrl Pts',(3.72348797293734,1.,0.793347023784205));
#44872=CARTESIAN_POINT('Ctrl Pts',(3.73086914695805,-1.,0.793682750269684));
#44873=CARTESIAN_POINT('Ctrl Pts',(3.73086914695805,1.,0.793682750269684));
#44874=CARTESIAN_POINT('Ctrl Pts',(3.73803280541687,-1.,0.793882700937017));
#44875=CARTESIAN_POINT('Ctrl Pts',(3.73803280541687,1.,0.793882700937017));
#44876=CARTESIAN_POINT('Ctrl Pts',(3.74511357728861,-1.,0.793982700459952));
#44877=CARTESIAN_POINT('Ctrl Pts',(3.74511357728861,1.,0.793982700459952));
#44878=CARTESIAN_POINT('Ctrl Pts',(3.75224692493864,-1.,0.794017347371378));
#44879=CARTESIAN_POINT('Ctrl Pts',(3.75224692493864,1.,0.794017347371378));
#44880=CARTESIAN_POINT('Ctrl Pts',(3.75951468666257,-1.,0.794008429134908));
#44881=CARTESIAN_POINT('Ctrl Pts',(3.75951468666257,1.,0.794008429134908));
#44882=CARTESIAN_POINT('Ctrl Pts',(3.76692626931111,-1.,0.793961083688992));
#44883=CARTESIAN_POINT('Ctrl Pts',(3.76692626931111,1.,0.793961083688992));
#44884=CARTESIAN_POINT('Ctrl Pts',(3.77444863801212,-1.,0.793870523787408));
#44885=CARTESIAN_POINT('Ctrl Pts',(3.77444863801212,1.,0.793870523787408));
#44886=CARTESIAN_POINT('Ctrl Pts',(3.78202460377598,-1.,0.793726235781301));
#44887=CARTESIAN_POINT('Ctrl Pts',(3.78202460377598,1.,0.793726235781301));
#44888=CARTESIAN_POINT('Ctrl Pts',(3.78959439439235,-1.,0.793516871680994));
#44889=CARTESIAN_POINT('Ctrl Pts',(3.78959439439235,1.,0.793516871680994));
#44890=CARTESIAN_POINT('Ctrl Pts',(3.79711921389897,-1.,0.793235612973274));
#44891=CARTESIAN_POINT('Ctrl Pts',(3.79711921389897,1.,0.793235612973274));
#44892=CARTESIAN_POINT('Ctrl Pts',(3.80459229925637,-1.,0.792882695234778));
#44893=CARTESIAN_POINT('Ctrl Pts',(3.80459229925637,1.,0.792882695234778));
#44894=CARTESIAN_POINT('Ctrl Pts',(3.81202588694756,-1.,0.792462483517635));
#44895=CARTESIAN_POINT('Ctrl Pts',(3.81202588694756,1.,0.792462483517635));
#44896=CARTESIAN_POINT('Ctrl Pts',(3.81944345442249,-1.,0.791981740718635));
#44897=CARTESIAN_POINT('Ctrl Pts',(3.81944345442249,1.,0.791981740718635));
#44898=CARTESIAN_POINT('Ctrl Pts',(3.82687033899792,-1.,0.791447528662369));
#44899=CARTESIAN_POINT('Ctrl Pts',(3.82687033899792,1.,0.791447528662369));
#44900=CARTESIAN_POINT('Ctrl Pts',(3.83432392054786,-1.,0.790865012705301));
#44901=CARTESIAN_POINT('Ctrl Pts',(3.83432392054786,1.,0.790865012705301));
#44902=CARTESIAN_POINT('Ctrl Pts',(3.84180762342454,-1.,0.790236124191243));
#44903=CARTESIAN_POINT('Ctrl Pts',(3.84180762342454,1.,0.790236124191243));
#44904=CARTESIAN_POINT('Ctrl Pts',(3.84931637808894,-1.,0.789560798155583));
#44905=CARTESIAN_POINT('Ctrl Pts',(3.84931637808894,1.,0.789560798155583));
#44906=CARTESIAN_POINT('Ctrl Pts',(3.85683995872529,-1.,0.788837734090672));
#44907=CARTESIAN_POINT('Ctrl Pts',(3.85683995872529,1.,0.788837734090672));
#44908=CARTESIAN_POINT('Ctrl Pts',(3.86436702561345,-1.,0.788065315093778));
#44909=CARTESIAN_POINT('Ctrl Pts',(3.86436702561345,1.,0.788065315093778));
#44910=CARTESIAN_POINT('Ctrl Pts',(3.87188916600912,-1.,0.787242527617999));
#44911=CARTESIAN_POINT('Ctrl Pts',(3.87188916600912,1.,0.787242527617999));
#44912=CARTESIAN_POINT('Ctrl Pts',(3.8794040281819,-1.,0.786369675812609));
#44913=CARTESIAN_POINT('Ctrl Pts',(3.8794040281819,1.,0.786369675812609));
#44914=CARTESIAN_POINT('Ctrl Pts',(3.88691313167398,-1.,0.785447890340731));
#44915=CARTESIAN_POINT('Ctrl Pts',(3.88691313167398,1.,0.785447890340731));
#44916=CARTESIAN_POINT('Ctrl Pts',(3.89442039235103,-1.,0.784478799358337));
#44917=CARTESIAN_POINT('Ctrl Pts',(3.89442039235103,1.,0.784478799358337));
#44918=CARTESIAN_POINT('Ctrl Pts',(3.9019303904397,-1.,0.783464141529082));
#44919=CARTESIAN_POINT('Ctrl Pts',(3.9019303904397,1.,0.783464141529082));
#44920=CARTESIAN_POINT('Ctrl Pts',(3.90944671004542,-1.,0.782405395622765));
#44921=CARTESIAN_POINT('Ctrl Pts',(3.90944671004542,1.,0.782405395622765));
#44922=CARTESIAN_POINT('Ctrl Pts',(3.91697036054676,-1.,0.781303428618367));
#44923=CARTESIAN_POINT('Ctrl Pts',(3.91697036054676,1.,0.781303428618367));
#44924=CARTESIAN_POINT('Ctrl Pts',(3.92450058323823,-1.,0.780158678615543));
#44925=CARTESIAN_POINT('Ctrl Pts',(3.92450058323823,1.,0.780158678615543));
#44926=CARTESIAN_POINT('Ctrl Pts',(3.93203552473174,-1.,0.778971308134821));
#44927=CARTESIAN_POINT('Ctrl Pts',(3.93203552473174,1.,0.778971308134821));
#44928=CARTESIAN_POINT('Ctrl Pts',(3.93957296768103,-1.,0.777741370568559));
#44929=CARTESIAN_POINT('Ctrl Pts',(3.93957296768103,1.,0.777741370568559));
#44930=CARTESIAN_POINT('Ctrl Pts',(3.94711101619447,-1.,0.776468966697922));
#44931=CARTESIAN_POINT('Ctrl Pts',(3.94711101619447,1.,0.776468966697922));
#44932=CARTESIAN_POINT('Ctrl Pts',(3.9546488545231,-1.,0.775154418039352));
#44933=CARTESIAN_POINT('Ctrl Pts',(3.9546488545231,1.,0.775154418039352));
#44934=CARTESIAN_POINT('Ctrl Pts',(3.96218649639807,-1.,0.773798212026566));
#44935=CARTESIAN_POINT('Ctrl Pts',(3.96218649639807,1.,0.773798212026566));
#44936=CARTESIAN_POINT('Ctrl Pts',(3.96972446532772,-1.,0.772400931772137));
#44937=CARTESIAN_POINT('Ctrl Pts',(3.96972446532772,1.,0.772400931772137));
#44938=CARTESIAN_POINT('Ctrl Pts',(3.97726349165488,-1.,0.770963190030471));
#44939=CARTESIAN_POINT('Ctrl Pts',(3.97726349165488,1.,0.770963190030471));
#44940=CARTESIAN_POINT('Ctrl Pts',(3.98480422348451,-1.,0.769485566245545));
#44941=CARTESIAN_POINT('Ctrl Pts',(3.98480422348451,1.,0.769485566245545));
#44942=CARTESIAN_POINT('Ctrl Pts',(3.9923468788101,-1.,0.767968531377915));
#44943=CARTESIAN_POINT('Ctrl Pts',(3.9923468788101,1.,0.767968531377915));
#44944=CARTESIAN_POINT('Ctrl Pts',(3.99989129179622,-1.,0.766412457136064));
#44945=CARTESIAN_POINT('Ctrl Pts',(3.99989129179622,1.,0.766412457136064));
#44946=CARTESIAN_POINT('Ctrl Pts',(4.00743706791509,-1.,0.764817648785198));
#44947=CARTESIAN_POINT('Ctrl Pts',(4.00743706791509,1.,0.764817648785198));
#44948=CARTESIAN_POINT('Ctrl Pts',(4.01498370680496,-1.,0.763184371182936));
#44949=CARTESIAN_POINT('Ctrl Pts',(4.01498370680496,1.,0.763184371182936));
#44950=CARTESIAN_POINT('Ctrl Pts',(4.02253072741268,-1.,0.761512875859805));
#44951=CARTESIAN_POINT('Ctrl Pts',(4.02253072741268,1.,0.761512875859805));
#44952=CARTESIAN_POINT('Ctrl Pts',(4.03007781954412,-1.,0.759803433243752));
#44953=CARTESIAN_POINT('Ctrl Pts',(4.03007781954412,1.,0.759803433243752));
#44954=CARTESIAN_POINT('Ctrl Pts',(4.03762485803119,-1.,0.758056338884945));
#44955=CARTESIAN_POINT('Ctrl Pts',(4.03762485803119,1.,0.758056338884945));
#44956=CARTESIAN_POINT('Ctrl Pts',(4.04517182653997,-1.,0.756271902369581));
#44957=CARTESIAN_POINT('Ctrl Pts',(4.04517182653997,1.,0.756271902369581));
#44958=CARTESIAN_POINT('Ctrl Pts',(4.05271876687915,-1.,0.754450441816078));
#44959=CARTESIAN_POINT('Ctrl Pts',(4.05271876687915,1.,0.754450441816078));
#44960=CARTESIAN_POINT('Ctrl Pts',(4.06026572221515,-1.,0.752592276483073));
#44961=CARTESIAN_POINT('Ctrl Pts',(4.06026572221515,1.,0.752592276483073));
#44962=CARTESIAN_POINT('Ctrl Pts',(4.06781267242378,-1.,0.750697720484037));
#44963=CARTESIAN_POINT('Ctrl Pts',(4.06781267242378,1.,0.750697720484037));
#44964=CARTESIAN_POINT('Ctrl Pts',(4.07535951056152,-1.,0.748767076680558));
#44965=CARTESIAN_POINT('Ctrl Pts',(4.07535951056152,1.,0.748767076680558));
#44966=CARTESIAN_POINT('Ctrl Pts',(4.08290608095642,-1.,0.746800631492316));
#44967=CARTESIAN_POINT('Ctrl Pts',(4.08290608095642,1.,0.746800631492316));
#44968=CARTESIAN_POINT('Ctrl Pts',(4.09045220253573,-1.,0.744798649706501));
#44969=CARTESIAN_POINT('Ctrl Pts',(4.09045220253573,1.,0.744798649706501));
#44970=CARTESIAN_POINT('Ctrl Pts',(4.09799769702611,-1.,0.742761369689842));
#44971=CARTESIAN_POINT('Ctrl Pts',(4.09799769702611,1.,0.742761369689842));
#44972=CARTESIAN_POINT('Ctrl Pts',(4.10554241757547,-1.,0.740688998553377));
#44973=CARTESIAN_POINT('Ctrl Pts',(4.10554241757547,1.,0.740688998553377));
#44974=CARTESIAN_POINT('Ctrl Pts',(4.11308626951927,-1.,0.738581708225844));
#44975=CARTESIAN_POINT('Ctrl Pts',(4.11308626951927,1.,0.738581708225844));
#44976=CARTESIAN_POINT('Ctrl Pts',(4.120629196238,-1.,0.736439634331345));
#44977=CARTESIAN_POINT('Ctrl Pts',(4.120629196238,1.,0.736439634331345));
#44978=CARTESIAN_POINT('Ctrl Pts',(4.12666277570844,-1.,0.734698226764093));
#44979=CARTESIAN_POINT('Ctrl Pts',(4.12666277570844,1.,0.734698226764093));
#44980=CARTESIAN_POINT('Ctrl Pts',(4.13118752795207,-1.,0.733376589323547));
#44981=CARTESIAN_POINT('Ctrl Pts',(4.13118752795207,1.,0.733376589323547));
#44982=CARTESIAN_POINT('Ctrl Pts',(4.1342038373684,-1.,0.73248857513516));
#44983=CARTESIAN_POINT('Ctrl Pts',(4.1342038373684,1.,0.73248857513516));
#44984=CARTESIAN_POINT('Ctrl Pts',(4.13571194405636,-1.,0.732042837400621));
#44985=CARTESIAN_POINT('Ctrl Pts',(4.13571194405636,1.,0.732042837400621));
#44986=CARTESIAN_POINT('',(3.66661143271685,1.,0.786422660831985));
#44987=CARTESIAN_POINT('Ctrl Pts',(3.66661143271685,-1.,0.786422660831986));
#44988=CARTESIAN_POINT('Ctrl Pts',(3.66661143271685,-0.666666666666667,
0.786422660831986));
#44989=CARTESIAN_POINT('Ctrl Pts',(3.66661143271685,-0.333333333333333,
0.786422660831986));
#44990=CARTESIAN_POINT('Ctrl Pts',(3.66661143271685,0.333333333333333,0.786422660831986));
#44991=CARTESIAN_POINT('Ctrl Pts',(3.66661143271685,0.666666666666667,0.786422660831986));
#44992=CARTESIAN_POINT('Ctrl Pts',(3.66661143271685,1.,0.786422660831986));
#44993=CARTESIAN_POINT('',(4.13571194405636,1.,0.732042837400621));
#44994=CARTESIAN_POINT('',(4.13571194405636,0.,0.732042837400621));
#44995=CARTESIAN_POINT('Ctrl Pts',(3.66661143271685,1.,0.786422660831985));
#44996=CARTESIAN_POINT('Ctrl Pts',(3.6666431041522,1.,0.786459983895432));
#44997=CARTESIAN_POINT('Ctrl Pts',(3.66680946938292,1.,0.786565919558984));
#44998=CARTESIAN_POINT('Ctrl Pts',(3.66743103898702,1.,0.786774337198063));
#44999=CARTESIAN_POINT('Ctrl Pts',(3.66907505398677,1.,0.787145041181546));
#45000=CARTESIAN_POINT('Ctrl Pts',(3.67252923663655,1.,0.787758799995743));
#45001=CARTESIAN_POINT('Ctrl Pts',(3.67777119516252,1.,0.788569566220286));
#45002=CARTESIAN_POINT('Ctrl Pts',(3.68428439783905,1.,0.789483546064387));
#45003=CARTESIAN_POINT('Ctrl Pts',(3.69172044327364,1.,0.790436284988788));
#45004=CARTESIAN_POINT('Ctrl Pts',(3.69968940808721,1.,0.79135657569598));
#45005=CARTESIAN_POINT('Ctrl Pts',(3.70781724021806,1.,0.792177688845818));
#45006=CARTESIAN_POINT('Ctrl Pts',(3.71580242396124,1.,0.792848377370287));
#45007=CARTESIAN_POINT('Ctrl Pts',(3.72348797293734,1.,0.793347023784205));
#45008=CARTESIAN_POINT('Ctrl Pts',(3.73086914695805,1.,0.793682750269684));
#45009=CARTESIAN_POINT('Ctrl Pts',(3.73803280541687,1.,0.793882700937017));
#45010=CARTESIAN_POINT('Ctrl Pts',(3.74511357728861,1.,0.793982700459952));
#45011=CARTESIAN_POINT('Ctrl Pts',(3.75224692493864,1.,0.794017347371378));
#45012=CARTESIAN_POINT('Ctrl Pts',(3.75951468666257,1.,0.794008429134908));
#45013=CARTESIAN_POINT('Ctrl Pts',(3.76692626931111,1.,0.793961083688992));
#45014=CARTESIAN_POINT('Ctrl Pts',(3.77444863801212,1.,0.793870523787408));
#45015=CARTESIAN_POINT('Ctrl Pts',(3.78202460377598,1.,0.793726235781301));
#45016=CARTESIAN_POINT('Ctrl Pts',(3.78959439439235,1.,0.793516871680994));
#45017=CARTESIAN_POINT('Ctrl Pts',(3.79711921389897,1.,0.793235612973274));
#45018=CARTESIAN_POINT('Ctrl Pts',(3.80459229925637,1.,0.792882695234778));
#45019=CARTESIAN_POINT('Ctrl Pts',(3.81202588694756,1.,0.792462483517635));
#45020=CARTESIAN_POINT('Ctrl Pts',(3.81944345442249,1.,0.791981740718635));
#45021=CARTESIAN_POINT('Ctrl Pts',(3.82687033899792,1.,0.791447528662369));
#45022=CARTESIAN_POINT('Ctrl Pts',(3.83432392054786,1.,0.790865012705301));
#45023=CARTESIAN_POINT('Ctrl Pts',(3.84180762342454,1.,0.790236124191243));
#45024=CARTESIAN_POINT('Ctrl Pts',(3.84931637808894,1.,0.789560798155583));
#45025=CARTESIAN_POINT('Ctrl Pts',(3.85683995872529,1.,0.788837734090672));
#45026=CARTESIAN_POINT('Ctrl Pts',(3.86436702561345,1.,0.788065315093778));
#45027=CARTESIAN_POINT('Ctrl Pts',(3.87188916600912,1.,0.787242527617999));
#45028=CARTESIAN_POINT('Ctrl Pts',(3.8794040281819,1.,0.786369675812609));
#45029=CARTESIAN_POINT('Ctrl Pts',(3.88691313167398,1.,0.785447890340731));
#45030=CARTESIAN_POINT('Ctrl Pts',(3.89442039235103,1.,0.784478799358337));
#45031=CARTESIAN_POINT('Ctrl Pts',(3.9019303904397,1.,0.783464141529082));
#45032=CARTESIAN_POINT('Ctrl Pts',(3.90944671004542,1.,0.782405395622765));
#45033=CARTESIAN_POINT('Ctrl Pts',(3.91697036054676,1.,0.781303428618367));
#45034=CARTESIAN_POINT('Ctrl Pts',(3.92450058323823,1.,0.780158678615543));
#45035=CARTESIAN_POINT('Ctrl Pts',(3.93203552473174,1.,0.778971308134821));
#45036=CARTESIAN_POINT('Ctrl Pts',(3.93957296768103,1.,0.777741370568559));
#45037=CARTESIAN_POINT('Ctrl Pts',(3.94711101619447,1.,0.776468966697922));
#45038=CARTESIAN_POINT('Ctrl Pts',(3.9546488545231,1.,0.775154418039352));
#45039=CARTESIAN_POINT('Ctrl Pts',(3.96218649639807,1.,0.773798212026566));
#45040=CARTESIAN_POINT('Ctrl Pts',(3.96972446532772,1.,0.772400931772137));
#45041=CARTESIAN_POINT('Ctrl Pts',(3.97726349165488,1.,0.770963190030471));
#45042=CARTESIAN_POINT('Ctrl Pts',(3.98480422348451,1.,0.769485566245545));
#45043=CARTESIAN_POINT('Ctrl Pts',(3.9923468788101,1.,0.767968531377915));
#45044=CARTESIAN_POINT('Ctrl Pts',(3.99989129179622,1.,0.766412457136064));
#45045=CARTESIAN_POINT('Ctrl Pts',(4.00743706791509,1.,0.764817648785198));
#45046=CARTESIAN_POINT('Ctrl Pts',(4.01498370680496,1.,0.763184371182936));
#45047=CARTESIAN_POINT('Ctrl Pts',(4.02253072741268,1.,0.761512875859805));
#45048=CARTESIAN_POINT('Ctrl Pts',(4.03007781954412,1.,0.759803433243752));
#45049=CARTESIAN_POINT('Ctrl Pts',(4.03762485803119,1.,0.758056338884945));
#45050=CARTESIAN_POINT('Ctrl Pts',(4.04517182653997,1.,0.756271902369581));
#45051=CARTESIAN_POINT('Ctrl Pts',(4.05271876687915,1.,0.754450441816078));
#45052=CARTESIAN_POINT('Ctrl Pts',(4.06026572221515,1.,0.752592276483073));
#45053=CARTESIAN_POINT('Ctrl Pts',(4.06781267242378,1.,0.750697720484037));
#45054=CARTESIAN_POINT('Ctrl Pts',(4.07535951056152,1.,0.748767076680558));
#45055=CARTESIAN_POINT('Ctrl Pts',(4.08290608095642,1.,0.746800631492316));
#45056=CARTESIAN_POINT('Ctrl Pts',(4.09045220253573,1.,0.744798649706501));
#45057=CARTESIAN_POINT('Ctrl Pts',(4.09799769702611,1.,0.742761369689842));
#45058=CARTESIAN_POINT('Ctrl Pts',(4.10554241757547,1.,0.740688998553377));
#45059=CARTESIAN_POINT('Ctrl Pts',(4.11308626951927,1.,0.738581708225844));
#45060=CARTESIAN_POINT('Ctrl Pts',(4.120629196238,1.,0.736439634331345));
#45061=CARTESIAN_POINT('Ctrl Pts',(4.12666277570844,1.,0.734698226764093));
#45062=CARTESIAN_POINT('Ctrl Pts',(4.13118752795207,1.,0.733376589323547));
#45063=CARTESIAN_POINT('Ctrl Pts',(4.1342038373684,1.,0.73248857513516));
#45064=CARTESIAN_POINT('Ctrl Pts',(4.13571194405636,1.,0.732042837400621));
#45065=CARTESIAN_POINT('Origin',(4.13571194405636,0.,0.732042837400621));
#45066=CARTESIAN_POINT('',(4.15950947128175,1.,0.581791163835816));
#45067=CARTESIAN_POINT('Origin',(0.,0.,0.));
#45068=CARTESIAN_POINT('',(3.62400312501245,1.,0.963899035117249));
#45069=CARTESIAN_POINT('Origin',(0.,1.,0.));
#45070=CARTESIAN_POINT('Ctrl Pts',(3.62400312501245,1.,0.963899035117249));
#45071=CARTESIAN_POINT('Ctrl Pts',(3.62400312501245,0.666666666666667,0.963899035117249));
#45072=CARTESIAN_POINT('Ctrl Pts',(3.62400312501245,0.333333333333333,0.963899035117249));
#45073=CARTESIAN_POINT('Ctrl Pts',(3.62400312501245,-0.333333333333333,
0.963899035117249));
#45074=CARTESIAN_POINT('Ctrl Pts',(3.62400312501245,-0.666666666666667,
0.96389903511725));
#45075=CARTESIAN_POINT('Ctrl Pts',(3.62400312501245,-1.,0.96389903511725));
#45076=CARTESIAN_POINT('Ctrl Pts',(4.01728681790024,-1.,1.22531898815164));
#45077=CARTESIAN_POINT('Ctrl Pts',(4.01728681790024,1.,1.22531898815164));
#45078=CARTESIAN_POINT('Ctrl Pts',(4.0161454457032,-1.,1.22423716681447));
#45079=CARTESIAN_POINT('Ctrl Pts',(4.0161454457032,1.,1.22423716681447));
#45080=CARTESIAN_POINT('Ctrl Pts',(4.01386104434674,-1.,1.22207656456199));
#45081=CARTESIAN_POINT('Ctrl Pts',(4.01386104434674,1.,1.22207656456199));
#45082=CARTESIAN_POINT('Ctrl Pts',(4.01042947142681,-1.,1.21884478244983));
#45083=CARTESIAN_POINT('Ctrl Pts',(4.01042947142681,1.,1.21884478244983));
#45084=CARTESIAN_POINT('Ctrl Pts',(4.00584409524937,-1.,1.21455398918813));
#45085=CARTESIAN_POINT('Ctrl Pts',(4.00584409524937,1.,1.21455398918813));
#45086=CARTESIAN_POINT('Ctrl Pts',(4.00009577952534,-1.,1.20922097030107));
#45087=CARTESIAN_POINT('Ctrl Pts',(4.00009577952534,1.,1.20922097030107));
#45088=CARTESIAN_POINT('Ctrl Pts',(3.99433084800649,-1.,1.2039185237544));
#45089=CARTESIAN_POINT('Ctrl Pts',(3.99433084800649,1.,1.2039185237544));
#45090=CARTESIAN_POINT('Ctrl Pts',(3.98854928957287,-1.,1.19864679609596));
#45091=CARTESIAN_POINT('Ctrl Pts',(3.98854928957287,1.,1.19864679609596));
#45092=CARTESIAN_POINT('Ctrl Pts',(3.98275111052015,-1.,1.19340598349307));
#45093=CARTESIAN_POINT('Ctrl Pts',(3.98275111052015,1.,1.19340598349307));
#45094=CARTESIAN_POINT('Ctrl Pts',(3.97693634766926,-1.,1.18819633715285));
#45095=CARTESIAN_POINT('Ctrl Pts',(3.97693634766926,1.,1.18819633715285));
#45096=CARTESIAN_POINT('Ctrl Pts',(3.9711050516465,-1.,1.18301815039596));
#45097=CARTESIAN_POINT('Ctrl Pts',(3.9711050516465,1.,1.18301815039596));
#45098=CARTESIAN_POINT('Ctrl Pts',(3.96525726357682,-1.,1.17787174135446));
#45099=CARTESIAN_POINT('Ctrl Pts',(3.96525726357682,1.,1.17787174135446));
#45100=CARTESIAN_POINT('Ctrl Pts',(3.95939299213164,-1.,1.17275743590327));
#45101=CARTESIAN_POINT('Ctrl Pts',(3.95939299213164,1.,1.17275743590327));
#45102=CARTESIAN_POINT('Ctrl Pts',(3.95351219510062,-1.,1.16767555244495));
#45103=CARTESIAN_POINT('Ctrl Pts',(3.95351219510062,1.,1.16767555244495));
#45104=CARTESIAN_POINT('Ctrl Pts',(3.9476147478092,-1.,1.16262637999261));
#45105=CARTESIAN_POINT('Ctrl Pts',(3.9476147478092,1.,1.16262637999261));
#45106=CARTESIAN_POINT('Ctrl Pts',(3.94170046685542,-1.,1.15761018341061));
#45107=CARTESIAN_POINT('Ctrl Pts',(3.94170046685542,1.,1.15761018341061));
#45108=CARTESIAN_POINT('Ctrl Pts',(3.9357691705651,-1.,1.15262722716391));
#45109=CARTESIAN_POINT('Ctrl Pts',(3.9357691705651,1.,1.15262722716391));
#45110=CARTESIAN_POINT('Ctrl Pts',(3.92982073294334,-1.,1.14767779451147));
#45111=CARTESIAN_POINT('Ctrl Pts',(3.92982073294334,1.,1.14767779451147));
#45112=CARTESIAN_POINT('Ctrl Pts',(3.92385513133937,-1.,1.14276220561575));
#45113=CARTESIAN_POINT('Ctrl Pts',(3.92385513133937,1.,1.14276220561575));
#45114=CARTESIAN_POINT('Ctrl Pts',(3.91787251936688,-1.,1.13788084225511));
#45115=CARTESIAN_POINT('Ctrl Pts',(3.91787251936688,1.,1.13788084225511));
#45116=CARTESIAN_POINT('Ctrl Pts',(3.91187321145495,-1.,1.13303414693849));
#45117=CARTESIAN_POINT('Ctrl Pts',(3.91187321145495,1.,1.13303414693849));
#45118=CARTESIAN_POINT('Ctrl Pts',(3.90585753318622,-1.,1.12822258281518));
#45119=CARTESIAN_POINT('Ctrl Pts',(3.90585753318622,1.,1.12822258281518));
#45120=CARTESIAN_POINT('Ctrl Pts',(3.89982569749978,-1.,1.12344660099029));
#45121=CARTESIAN_POINT('Ctrl Pts',(3.89982569749978,1.,1.12344660099029));
#45122=CARTESIAN_POINT('Ctrl Pts',(3.89377768340362,-1.,1.11870660794609));
#45123=CARTESIAN_POINT('Ctrl Pts',(3.89377768340362,1.,1.11870660794609));
#45124=CARTESIAN_POINT('Ctrl Pts',(3.88771308285229,-1.,1.11400292434447));
#45125=CARTESIAN_POINT('Ctrl Pts',(3.88771308285229,1.,1.11400292434447));
#45126=CARTESIAN_POINT('Ctrl Pts',(3.88163105531791,-1.,1.10933577224029));
#45127=CARTESIAN_POINT('Ctrl Pts',(3.88163105531791,1.,1.10933577224029));
#45128=CARTESIAN_POINT('Ctrl Pts',(3.87553067187566,-1.,1.10470536603303));
#45129=CARTESIAN_POINT('Ctrl Pts',(3.87553067187566,1.,1.10470536603303));
#45130=CARTESIAN_POINT('Ctrl Pts',(3.86941120134872,-1.,1.10011198761203));
#45131=CARTESIAN_POINT('Ctrl Pts',(3.86941120134872,1.,1.10011198761203));
#45132=CARTESIAN_POINT('Ctrl Pts',(3.86327241021242,-1.,1.09555606505012));
#45133=CARTESIAN_POINT('Ctrl Pts',(3.86327241021242,1.,1.09555606505012));
#45134=CARTESIAN_POINT('Ctrl Pts',(3.85711487933911,-1.,1.09103825516288));
#45135=CARTESIAN_POINT('Ctrl Pts',(3.85711487933911,1.,1.09103825516288));
#45136=CARTESIAN_POINT('Ctrl Pts',(3.8509402522269,-1.,1.08655950846377));
#45137=CARTESIAN_POINT('Ctrl Pts',(3.8509402522269,1.,1.08655950846377));
#45138=CARTESIAN_POINT('Ctrl Pts',(3.84475048030615,-1.,1.08212087917986));
#45139=CARTESIAN_POINT('Ctrl Pts',(3.84475048030615,1.,1.08212087917986));
#45140=CARTESIAN_POINT('Ctrl Pts',(3.83854714117486,-1.,1.07772335353856));
#45141=CARTESIAN_POINT('Ctrl Pts',(3.83854714117486,1.,1.07772335353856));
#45142=CARTESIAN_POINT('Ctrl Pts',(3.83233071195145,-1.,1.0733676663346));
#45143=CARTESIAN_POINT('Ctrl Pts',(3.83233071195145,1.,1.0733676663346));
#45144=CARTESIAN_POINT('Ctrl Pts',(3.82609989967278,-1.,1.0690541318036));
#45145=CARTESIAN_POINT('Ctrl Pts',(3.82609989967278,1.,1.0690541318036));
#45146=CARTESIAN_POINT('Ctrl Pts',(3.81985083953012,-1.,1.06478244038931));
#45147=CARTESIAN_POINT('Ctrl Pts',(3.81985083953012,1.,1.06478244038931));
#45148=CARTESIAN_POINT('Ctrl Pts',(3.81357866117485,-1.,1.06055206187298));
#45149=CARTESIAN_POINT('Ctrl Pts',(3.81357866117485,1.,1.06055206187298));
#45150=CARTESIAN_POINT('Ctrl Pts',(3.80727913637784,-1.,1.05636266918643));
#45151=CARTESIAN_POINT('Ctrl Pts',(3.80727913637784,1.,1.05636266918643));
#45152=CARTESIAN_POINT('Ctrl Pts',(3.80095039790678,-1.,1.05221457990015));
#45153=CARTESIAN_POINT('Ctrl Pts',(3.80095039790678,1.,1.05221457990015));
#45154=CARTESIAN_POINT('Ctrl Pts',(3.79459440308793,-1.,1.04810913267641));
#45155=CARTESIAN_POINT('Ctrl Pts',(3.79459440308793,1.,1.04810913267641));
#45156=CARTESIAN_POINT('Ctrl Pts',(3.78821910787195,-1.,1.04404924374426));
#45157=CARTESIAN_POINT('Ctrl Pts',(3.78821910787195,1.,1.04404924374426));
#45158=CARTESIAN_POINT('Ctrl Pts',(3.78183535008192,-1.,1.04003862055804));
#45159=CARTESIAN_POINT('Ctrl Pts',(3.78183535008192,1.,1.04003862055804));
#45160=CARTESIAN_POINT('Ctrl Pts',(3.77545283140445,-1.,1.03608074678013));
#45161=CARTESIAN_POINT('Ctrl Pts',(3.77545283140445,1.,1.03608074678013));
#45162=CARTESIAN_POINT('Ctrl Pts',(3.76907609832522,-1.,1.0321778660492));
#45163=CARTESIAN_POINT('Ctrl Pts',(3.76907609832522,1.,1.0321778660492));
#45164=CARTESIAN_POINT('Ctrl Pts',(3.76270122291232,-1.,1.02833014458181));
#45165=CARTESIAN_POINT('Ctrl Pts',(3.76270122291232,1.,1.02833014458181));
#45166=CARTESIAN_POINT('Ctrl Pts',(3.75631037456194,-1.,1.0245342944466));
#45167=CARTESIAN_POINT('Ctrl Pts',(3.75631037456194,1.,1.0245342944466));
#45168=CARTESIAN_POINT('Ctrl Pts',(3.74987777155834,-1.,1.02078510487428));
#45169=CARTESIAN_POINT('Ctrl Pts',(3.74987777155834,1.,1.02078510487428));
#45170=CARTESIAN_POINT('Ctrl Pts',(3.74337942504959,-1.,1.01707794311079));
#45171=CARTESIAN_POINT('Ctrl Pts',(3.74337942504959,1.,1.01707794311079));
#45172=CARTESIAN_POINT('Ctrl Pts',(3.73680245055734,-1.,1.01341114319903));
#45173=CARTESIAN_POINT('Ctrl Pts',(3.73680245055734,1.,1.01341114319903));
#45174=CARTESIAN_POINT('Ctrl Pts',(3.73015276704426,-1.,1.00978798539496));
#45175=CARTESIAN_POINT('Ctrl Pts',(3.73015276704426,1.,1.00978798539496));
#45176=CARTESIAN_POINT('Ctrl Pts',(3.72346803750595,-1.,1.0062200073571));
#45177=CARTESIAN_POINT('Ctrl Pts',(3.72346803750595,1.,1.0062200073571));
#45178=CARTESIAN_POINT('Ctrl Pts',(3.71680667125118,-1.,1.00272423396822));
#45179=CARTESIAN_POINT('Ctrl Pts',(3.71680667125118,1.,1.00272423396822));
#45180=CARTESIAN_POINT('Ctrl Pts',(3.71022439713938,-1.,0.999317260756531));
#45181=CARTESIAN_POINT('Ctrl Pts',(3.71022439713938,1.,0.999317260756531));
#45182=CARTESIAN_POINT('Ctrl Pts',(3.70375282282138,-1.,0.996009819772518));
#45183=CARTESIAN_POINT('Ctrl Pts',(3.70375282282138,1.,0.996009819772518));
#45184=CARTESIAN_POINT('Ctrl Pts',(3.69738123415662,-1.,0.992802218332011));
#45185=CARTESIAN_POINT('Ctrl Pts',(3.69738123415662,1.,0.992802218332011));
#45186=CARTESIAN_POINT('Ctrl Pts',(3.69102682138846,-1.,0.989676715398559));
#45187=CARTESIAN_POINT('Ctrl Pts',(3.69102682138846,1.,0.989676715398559));
#45188=CARTESIAN_POINT('Ctrl Pts',(3.68455317926068,-1.,0.986602639863838));
#45189=CARTESIAN_POINT('Ctrl Pts',(3.68455317926068,1.,0.986602639863838));
#45190=CARTESIAN_POINT('Ctrl Pts',(3.67782408841715,-1.,0.98355079147042));
#45191=CARTESIAN_POINT('Ctrl Pts',(3.67782408841715,1.,0.98355079147042));
#45192=CARTESIAN_POINT('Ctrl Pts',(3.67074983340361,-1.,0.980505922458267));
#45193=CARTESIAN_POINT('Ctrl Pts',(3.67074983340361,1.,0.980505922458267));
#45194=CARTESIAN_POINT('Ctrl Pts',(3.66333049637475,-1.,0.977478312751618));
#45195=CARTESIAN_POINT('Ctrl Pts',(3.66333049637475,1.,0.977478312751618));
#45196=CARTESIAN_POINT('Ctrl Pts',(3.65571576735126,-1.,0.974519971354849));
#45197=CARTESIAN_POINT('Ctrl Pts',(3.65571576735126,1.,0.974519971354849));
#45198=CARTESIAN_POINT('Ctrl Pts',(3.64819756447455,-1.,0.971722122061341));
#45199=CARTESIAN_POINT('Ctrl Pts',(3.64819756447455,1.,0.971722122061341));
#45200=CARTESIAN_POINT('Ctrl Pts',(3.64113946505766,-1.,0.969195124675866));
#45201=CARTESIAN_POINT('Ctrl Pts',(3.64113946505766,1.,0.969195124675866));
#45202=CARTESIAN_POINT('Ctrl Pts',(3.63492122081143,-1.,0.967052554541386));
#45203=CARTESIAN_POINT('Ctrl Pts',(3.63492122081143,1.,0.967052554541386));
#45204=CARTESIAN_POINT('Ctrl Pts',(3.62988252139846,-1.,0.965395153165294));
#45205=CARTESIAN_POINT('Ctrl Pts',(3.62988252139846,1.,0.965395153165294));
#45206=CARTESIAN_POINT('Ctrl Pts',(3.62625391254797,-1.,0.964291001273288));
#45207=CARTESIAN_POINT('Ctrl Pts',(3.62625391254797,1.,0.964291001273288));
#45208=CARTESIAN_POINT('Ctrl Pts',(3.6245656860652,-1.,0.96387577453062));
#45209=CARTESIAN_POINT('Ctrl Pts',(3.6245656860652,1.,0.96387577453062));
#45210=CARTESIAN_POINT('Ctrl Pts',(3.62399933639914,-1.,0.963832486395052));
#45211=CARTESIAN_POINT('Ctrl Pts',(3.62399933639914,1.,0.963832486395052));
#45212=CARTESIAN_POINT('Ctrl Pts',(3.62393257642052,-1.,0.963922720982194));
#45213=CARTESIAN_POINT('Ctrl Pts',(3.62393257642052,1.,0.963922720982194));
#45214=CARTESIAN_POINT('Ctrl Pts',(3.62397690409552,-1.,0.963997613369571));
#45215=CARTESIAN_POINT('Ctrl Pts',(3.62397690409552,1.,0.963997613369571));
#45216=CARTESIAN_POINT('',(4.01728681790024,1.,1.22531898815164));
#45217=CARTESIAN_POINT('Ctrl Pts',(4.01728681790024,1.,1.22531898815164));
#45218=CARTESIAN_POINT('Ctrl Pts',(4.0161454457032,1.,1.22423716681447));
#45219=CARTESIAN_POINT('Ctrl Pts',(4.01386104434674,1.,1.22207656456199));
#45220=CARTESIAN_POINT('Ctrl Pts',(4.01042947142681,1.,1.21884478244983));
#45221=CARTESIAN_POINT('Ctrl Pts',(4.00584409524937,1.,1.21455398918813));
#45222=CARTESIAN_POINT('Ctrl Pts',(4.00009577952534,1.,1.20922097030107));
#45223=CARTESIAN_POINT('Ctrl Pts',(3.99433084800649,1.,1.2039185237544));
#45224=CARTESIAN_POINT('Ctrl Pts',(3.98854928957287,1.,1.19864679609596));
#45225=CARTESIAN_POINT('Ctrl Pts',(3.98275111052015,1.,1.19340598349307));
#45226=CARTESIAN_POINT('Ctrl Pts',(3.97693634766926,1.,1.18819633715285));
#45227=CARTESIAN_POINT('Ctrl Pts',(3.9711050516465,1.,1.18301815039596));
#45228=CARTESIAN_POINT('Ctrl Pts',(3.96525726357682,1.,1.17787174135446));
#45229=CARTESIAN_POINT('Ctrl Pts',(3.95939299213164,1.,1.17275743590327));
#45230=CARTESIAN_POINT('Ctrl Pts',(3.95351219510062,1.,1.16767555244495));
#45231=CARTESIAN_POINT('Ctrl Pts',(3.9476147478092,1.,1.16262637999261));
#45232=CARTESIAN_POINT('Ctrl Pts',(3.94170046685542,1.,1.15761018341061));
#45233=CARTESIAN_POINT('Ctrl Pts',(3.9357691705651,1.,1.15262722716391));
#45234=CARTESIAN_POINT('Ctrl Pts',(3.92982073294334,1.,1.14767779451147));
#45235=CARTESIAN_POINT('Ctrl Pts',(3.92385513133937,1.,1.14276220561575));
#45236=CARTESIAN_POINT('Ctrl Pts',(3.91787251936688,1.,1.13788084225511));
#45237=CARTESIAN_POINT('Ctrl Pts',(3.91187321145495,1.,1.13303414693849));
#45238=CARTESIAN_POINT('Ctrl Pts',(3.90585753318622,1.,1.12822258281518));
#45239=CARTESIAN_POINT('Ctrl Pts',(3.89982569749978,1.,1.12344660099029));
#45240=CARTESIAN_POINT('Ctrl Pts',(3.89377768340362,1.,1.11870660794609));
#45241=CARTESIAN_POINT('Ctrl Pts',(3.88771308285229,1.,1.11400292434447));
#45242=CARTESIAN_POINT('Ctrl Pts',(3.88163105531791,1.,1.10933577224029));
#45243=CARTESIAN_POINT('Ctrl Pts',(3.87553067187566,1.,1.10470536603303));
#45244=CARTESIAN_POINT('Ctrl Pts',(3.86941120134872,1.,1.10011198761203));
#45245=CARTESIAN_POINT('Ctrl Pts',(3.86327241021242,1.,1.09555606505012));
#45246=CARTESIAN_POINT('Ctrl Pts',(3.85711487933911,1.,1.09103825516288));
#45247=CARTESIAN_POINT('Ctrl Pts',(3.8509402522269,1.,1.08655950846377));
#45248=CARTESIAN_POINT('Ctrl Pts',(3.84475048030615,1.,1.08212087917986));
#45249=CARTESIAN_POINT('Ctrl Pts',(3.83854714117486,1.,1.07772335353856));
#45250=CARTESIAN_POINT('Ctrl Pts',(3.83233071195145,1.,1.0733676663346));
#45251=CARTESIAN_POINT('Ctrl Pts',(3.82609989967278,1.,1.0690541318036));
#45252=CARTESIAN_POINT('Ctrl Pts',(3.81985083953012,1.,1.06478244038931));
#45253=CARTESIAN_POINT('Ctrl Pts',(3.81357866117485,1.,1.06055206187298));
#45254=CARTESIAN_POINT('Ctrl Pts',(3.80727913637784,1.,1.05636266918643));
#45255=CARTESIAN_POINT('Ctrl Pts',(3.80095039790678,1.,1.05221457990015));
#45256=CARTESIAN_POINT('Ctrl Pts',(3.79459440308793,1.,1.04810913267641));
#45257=CARTESIAN_POINT('Ctrl Pts',(3.78821910787195,1.,1.04404924374426));
#45258=CARTESIAN_POINT('Ctrl Pts',(3.78183535008192,1.,1.04003862055804));
#45259=CARTESIAN_POINT('Ctrl Pts',(3.77545283140445,1.,1.03608074678013));
#45260=CARTESIAN_POINT('Ctrl Pts',(3.76907609832522,1.,1.0321778660492));
#45261=CARTESIAN_POINT('Ctrl Pts',(3.76270122291232,1.,1.02833014458181));
#45262=CARTESIAN_POINT('Ctrl Pts',(3.75631037456194,1.,1.0245342944466));
#45263=CARTESIAN_POINT('Ctrl Pts',(3.74987777155834,1.,1.02078510487428));
#45264=CARTESIAN_POINT('Ctrl Pts',(3.74337942504959,1.,1.01707794311079));
#45265=CARTESIAN_POINT('Ctrl Pts',(3.73680245055734,1.,1.01341114319903));
#45266=CARTESIAN_POINT('Ctrl Pts',(3.73015276704426,1.,1.00978798539496));
#45267=CARTESIAN_POINT('Ctrl Pts',(3.72346803750595,1.,1.0062200073571));
#45268=CARTESIAN_POINT('Ctrl Pts',(3.71680667125118,1.,1.00272423396822));
#45269=CARTESIAN_POINT('Ctrl Pts',(3.71022439713938,1.,0.999317260756531));
#45270=CARTESIAN_POINT('Ctrl Pts',(3.70375282282138,1.,0.996009819772518));
#45271=CARTESIAN_POINT('Ctrl Pts',(3.69738123415662,1.,0.992802218332011));
#45272=CARTESIAN_POINT('Ctrl Pts',(3.69102682138846,1.,0.989676715398559));
#45273=CARTESIAN_POINT('Ctrl Pts',(3.68455317926068,1.,0.986602639863838));
#45274=CARTESIAN_POINT('Ctrl Pts',(3.67782408841715,1.,0.98355079147042));
#45275=CARTESIAN_POINT('Ctrl Pts',(3.67074983340361,1.,0.980505922458267));
#45276=CARTESIAN_POINT('Ctrl Pts',(3.66333049637475,1.,0.977478312751618));
#45277=CARTESIAN_POINT('Ctrl Pts',(3.65571576735126,1.,0.974519971354849));
#45278=CARTESIAN_POINT('Ctrl Pts',(3.64819756447455,1.,0.971722122061341));
#45279=CARTESIAN_POINT('Ctrl Pts',(3.64113946505766,1.,0.969195124675866));
#45280=CARTESIAN_POINT('Ctrl Pts',(3.63492122081143,1.,0.967052554541386));
#45281=CARTESIAN_POINT('Ctrl Pts',(3.62988252139846,1.,0.965395153165294));
#45282=CARTESIAN_POINT('Ctrl Pts',(3.62652618145335,1.,0.964373850166458));
#45283=CARTESIAN_POINT('Ctrl Pts',(3.62489305727662,1.,0.963957782642844));
#45284=CARTESIAN_POINT('Ctrl Pts',(3.62424461507588,1.,0.963861297423241));
#45285=CARTESIAN_POINT('Ctrl Pts',(3.6240482887845,1.,0.963880158555582));
#45286=CARTESIAN_POINT('Ctrl Pts',(3.62400312501245,1.,0.963899035117249));
#45287=CARTESIAN_POINT('',(4.01728681790024,0.,1.22531898815164));
#45288=CARTESIAN_POINT('Ctrl Pts',(3.49848248301936,-1.,1.35022972712301));
#45289=CARTESIAN_POINT('Ctrl Pts',(3.49848248301936,1.,1.35022972712301));
#45290=CARTESIAN_POINT('Ctrl Pts',(3.4984026005375,-1.,1.35026426118402));
#45291=CARTESIAN_POINT('Ctrl Pts',(3.4984026005375,1.,1.35026426118402));
#45292=CARTESIAN_POINT('Ctrl Pts',(3.49840357193736,-1.,1.35037650303019));
#45293=CARTESIAN_POINT('Ctrl Pts',(3.49840357193736,1.,1.35037650303019));
#45294=CARTESIAN_POINT('Ctrl Pts',(3.49888720257132,-1.,1.35067437417484));
#45295=CARTESIAN_POINT('Ctrl Pts',(3.49888720257132,1.,1.35067437417484));
#45296=CARTESIAN_POINT('Ctrl Pts',(3.5004970706414,-1.,1.3513307633124));
#45297=CARTESIAN_POINT('Ctrl Pts',(3.5004970706414,1.,1.3513307633124));
#45298=CARTESIAN_POINT('Ctrl Pts',(3.50408168106261,-1.,1.35257032843486));
#45299=CARTESIAN_POINT('Ctrl Pts',(3.50408168106261,1.,1.35257032843486));
#45300=CARTESIAN_POINT('Ctrl Pts',(3.50913227059999,-1.,1.35419113575956));
#45301=CARTESIAN_POINT('Ctrl Pts',(3.50913227059999,1.,1.35419113575956));
#45302=CARTESIAN_POINT('Ctrl Pts',(3.51542230699556,-1.,1.35611275237152));
#45303=CARTESIAN_POINT('Ctrl Pts',(3.51542230699556,1.,1.35611275237152));
#45304=CARTESIAN_POINT('Ctrl Pts',(3.52261776116748,-1.,1.35821701528836));
#45305=CARTESIAN_POINT('Ctrl Pts',(3.52261776116748,1.,1.35821701528836));
#45306=CARTESIAN_POINT('Ctrl Pts',(3.530344649616,-1.,1.36037259643734));
#45307=CARTESIAN_POINT('Ctrl Pts',(3.530344649616,1.,1.36037259643734));
#45308=CARTESIAN_POINT('Ctrl Pts',(3.53824396424961,-1.,1.36245507339307));
#45309=CARTESIAN_POINT('Ctrl Pts',(3.53824396424961,1.,1.36245507339307));
#45310=CARTESIAN_POINT('Ctrl Pts',(3.54602591832973,-1.,1.36436666257598));
#45311=CARTESIAN_POINT('Ctrl Pts',(3.54602591832973,1.,1.36436666257598));
#45312=CARTESIAN_POINT('Ctrl Pts',(3.55353883995949,-1.,1.3660614545677));
#45313=CARTESIAN_POINT('Ctrl Pts',(3.55353883995949,1.,1.3660614545677));
#45314=CARTESIAN_POINT('Ctrl Pts',(3.56077662028649,-1.,1.36754771771233));
#45315=CARTESIAN_POINT('Ctrl Pts',(3.56077662028649,1.,1.36754771771233));
#45316=CARTESIAN_POINT('Ctrl Pts',(3.5678208030466,-1.,1.36886584973389));
#45317=CARTESIAN_POINT('Ctrl Pts',(3.5678208030466,1.,1.36886584973389));
#45318=CARTESIAN_POINT('Ctrl Pts',(3.57479875549486,-1.,1.37007229485659));
#45319=CARTESIAN_POINT('Ctrl Pts',(3.57479875549486,1.,1.37007229485659));
#45320=CARTESIAN_POINT('Ctrl Pts',(3.58183885982715,-1.,1.37122241663062));
#45321=CARTESIAN_POINT('Ctrl Pts',(3.58183885982715,1.,1.37122241663062));
#45322=CARTESIAN_POINT('Ctrl Pts',(3.58901853846365,-1.,1.37235053660976));
#45323=CARTESIAN_POINT('Ctrl Pts',(3.58901853846365,1.,1.37235053660976));
#45324=CARTESIAN_POINT('Ctrl Pts',(3.59634627869048,-1.,1.37346320103157));
#45325=CARTESIAN_POINT('Ctrl Pts',(3.59634627869048,1.,1.37346320103157));
#45326=CARTESIAN_POINT('Ctrl Pts',(3.60379020123988,-1.,1.37455051379623));
#45327=CARTESIAN_POINT('Ctrl Pts',(3.60379020123988,1.,1.37455051379623));
#45328=CARTESIAN_POINT('Ctrl Pts',(3.61129546591064,-1.,1.37559314436634));
#45329=CARTESIAN_POINT('Ctrl Pts',(3.61129546591064,1.,1.37559314436634));
#45330=CARTESIAN_POINT('Ctrl Pts',(3.6188048116042,-1.,1.37657053403107));
#45331=CARTESIAN_POINT('Ctrl Pts',(3.6188048116042,1.,1.37657053403107));
#45332=CARTESIAN_POINT('Ctrl Pts',(3.62628098665145,-1.,1.37746987919881));
#45333=CARTESIAN_POINT('Ctrl Pts',(3.62628098665145,1.,1.37746987919881));
#45334=CARTESIAN_POINT('Ctrl Pts',(3.63371727442486,-1.,1.37829035457339));
#45335=CARTESIAN_POINT('Ctrl Pts',(3.63371727442486,1.,1.37829035457339));
#45336=CARTESIAN_POINT('Ctrl Pts',(3.64112507791141,-1.,1.37903818567359));
#45337=CARTESIAN_POINT('Ctrl Pts',(3.64112507791141,1.,1.37903818567359));
#45338=CARTESIAN_POINT('Ctrl Pts',(3.64852652756456,-1.,1.37972372481603));
#45339=CARTESIAN_POINT('Ctrl Pts',(3.64852652756456,1.,1.37972372481603));
#45340=CARTESIAN_POINT('Ctrl Pts',(3.6559455440439,-1.,1.38035791051213));
#45341=CARTESIAN_POINT('Ctrl Pts',(3.6559455440439,1.,1.38035791051213));
#45342=CARTESIAN_POINT('Ctrl Pts',(3.66339848520857,-1.,1.38094856333552));
#45343=CARTESIAN_POINT('Ctrl Pts',(3.66339848520857,1.,1.38094856333552));
#45344=CARTESIAN_POINT('Ctrl Pts',(3.67088843112262,-1.,1.38149812653868));
#45345=CARTESIAN_POINT('Ctrl Pts',(3.67088843112262,1.,1.38149812653868));
#45346=CARTESIAN_POINT('Ctrl Pts',(3.67841038482414,-1.,1.3820057429062));
#45347=CARTESIAN_POINT('Ctrl Pts',(3.67841038482414,1.,1.3820057429062));
#45348=CARTESIAN_POINT('Ctrl Pts',(3.68595444983837,-1.,1.38246852827182));
#45349=CARTESIAN_POINT('Ctrl Pts',(3.68595444983837,1.,1.38246852827182));
#45350=CARTESIAN_POINT('Ctrl Pts',(3.69350967899526,-1.,1.38288311171651));
#45351=CARTESIAN_POINT('Ctrl Pts',(3.69350967899526,1.,1.38288311171651));
#45352=CARTESIAN_POINT('Ctrl Pts',(3.701067921679,-1.,1.38324717612865));
#45353=CARTESIAN_POINT('Ctrl Pts',(3.701067921679,1.,1.38324717612865));
#45354=CARTESIAN_POINT('Ctrl Pts',(3.70862680753347,-1.,1.38356065402124));
#45355=CARTESIAN_POINT('Ctrl Pts',(3.70862680753347,1.,1.38356065402124));
#45356=CARTESIAN_POINT('Ctrl Pts',(3.7161876605181,-1.,1.38382489984586));
#45357=CARTESIAN_POINT('Ctrl Pts',(3.7161876605181,1.,1.38382489984586));
#45358=CARTESIAN_POINT('Ctrl Pts',(3.72375409358803,-1.,1.3840421342895));
#45359=CARTESIAN_POINT('Ctrl Pts',(3.72375409358803,1.,1.3840421342895));
#45360=CARTESIAN_POINT('Ctrl Pts',(3.73133035859282,-1.,1.38421479111531));
#45361=CARTESIAN_POINT('Ctrl Pts',(3.73133035859282,1.,1.38421479111531));
#45362=CARTESIAN_POINT('Ctrl Pts',(3.73891976418104,-1.,1.38434489156458));
#45363=CARTESIAN_POINT('Ctrl Pts',(3.73891976418104,1.,1.38434489156458));
#45364=CARTESIAN_POINT('Ctrl Pts',(3.74652317167876,-1.,1.38443344984394));
#45365=CARTESIAN_POINT('Ctrl Pts',(3.74652317167876,1.,1.38443344984394));
#45366=CARTESIAN_POINT('Ctrl Pts',(3.7541397631875,-1.,1.38448077997163));
#45367=CARTESIAN_POINT('Ctrl Pts',(3.7541397631875,1.,1.38448077997163));
#45368=CARTESIAN_POINT('Ctrl Pts',(3.76176768271367,-1.,1.3844867525335));
#45369=CARTESIAN_POINT('Ctrl Pts',(3.76176768271367,1.,1.3844867525335));
#45370=CARTESIAN_POINT('Ctrl Pts',(3.76940473185779,-1.,1.38445107339518));
#45371=CARTESIAN_POINT('Ctrl Pts',(3.76940473185779,1.,1.38445107339518));
#45372=CARTESIAN_POINT('Ctrl Pts',(3.77704902230418,-1.,1.38437354551428));
#45373=CARTESIAN_POINT('Ctrl Pts',(3.77704902230418,1.,1.38437354551428));
#45374=CARTESIAN_POINT('Ctrl Pts',(3.78469969805082,-1.,1.38425435883756));
#45375=CARTESIAN_POINT('Ctrl Pts',(3.78469969805082,1.,1.38425435883756));
#45376=CARTESIAN_POINT('Ctrl Pts',(3.79235669640841,-1.,1.38409399694566));
#45377=CARTESIAN_POINT('Ctrl Pts',(3.79235669640841,1.,1.38409399694566));
#45378=CARTESIAN_POINT('Ctrl Pts',(3.80002044322111,-1.,1.38389311766682));
#45379=CARTESIAN_POINT('Ctrl Pts',(3.80002044322111,1.,1.38389311766682));
#45380=CARTESIAN_POINT('Ctrl Pts',(3.80769156398411,-1.,1.3836524404622));
#45381=CARTESIAN_POINT('Ctrl Pts',(3.80769156398411,1.,1.3836524404622));
#45382=CARTESIAN_POINT('Ctrl Pts',(3.81537060817811,-1.,1.38337263902782));
#45383=CARTESIAN_POINT('Ctrl Pts',(3.81537060817811,1.,1.38337263902782));
#45384=CARTESIAN_POINT('Ctrl Pts',(3.82305771743829,-1.,1.38305421262763));
#45385=CARTESIAN_POINT('Ctrl Pts',(3.82305771743829,1.,1.38305421262763));
#45386=CARTESIAN_POINT('Ctrl Pts',(3.8307526698229,-1.,1.38269750245138));
#45387=CARTESIAN_POINT('Ctrl Pts',(3.8307526698229,1.,1.38269750245138));
#45388=CARTESIAN_POINT('Ctrl Pts',(3.83845502790746,-1.,1.38230274828822));
#45389=CARTESIAN_POINT('Ctrl Pts',(3.83845502790746,1.,1.38230274828822));
#45390=CARTESIAN_POINT('Ctrl Pts',(3.84616425605764,-1.,1.38187013346109));
#45391=CARTESIAN_POINT('Ctrl Pts',(3.84616425605764,1.,1.38187013346109));
#45392=CARTESIAN_POINT('Ctrl Pts',(3.85387983979481,-1.,1.3813998311505));
#45393=CARTESIAN_POINT('Ctrl Pts',(3.85387983979481,1.,1.3813998311505));
#45394=CARTESIAN_POINT('Ctrl Pts',(3.86160143043959,-1.,1.3808920599299));
#45395=CARTESIAN_POINT('Ctrl Pts',(3.86160143043959,1.,1.3808920599299));
#45396=CARTESIAN_POINT('Ctrl Pts',(3.86932885813068,-1.,1.38034709213014));
#45397=CARTESIAN_POINT('Ctrl Pts',(3.86932885813068,1.,1.38034709213014));
#45398=CARTESIAN_POINT('Ctrl Pts',(3.87706205830532,-1.,1.37976523097073));
#45399=CARTESIAN_POINT('Ctrl Pts',(3.87706205830532,1.,1.37976523097073));
#45400=CARTESIAN_POINT('Ctrl Pts',(3.88480102249277,-1.,1.37914679719383));
#45401=CARTESIAN_POINT('Ctrl Pts',(3.88480102249277,1.,1.37914679719383));
#45402=CARTESIAN_POINT('Ctrl Pts',(3.89254574338496,-1.,1.3784921128802));
#45403=CARTESIAN_POINT('Ctrl Pts',(3.89254574338496,1.,1.3784921128802));
#45404=CARTESIAN_POINT('Ctrl Pts',(3.90029615196727,-1.,1.37780148512792));
#45405=CARTESIAN_POINT('Ctrl Pts',(3.90029615196727,1.,1.37780148512792));
#45406=CARTESIAN_POINT('Ctrl Pts',(3.90805209523486,-1.,1.3770751963402));
#45407=CARTESIAN_POINT('Ctrl Pts',(3.90805209523486,1.,1.3770751963402));
#45408=CARTESIAN_POINT('Ctrl Pts',(3.91581337462644,-1.,1.37631350505797));
#45409=CARTESIAN_POINT('Ctrl Pts',(3.91581337462644,1.,1.37631350505797));
#45410=CARTESIAN_POINT('Ctrl Pts',(3.92357976987672,-1.,1.37551664448242));
#45411=CARTESIAN_POINT('Ctrl Pts',(3.92357976987672,1.,1.37551664448242));
#45412=CARTESIAN_POINT('Ctrl Pts',(3.93135106761844,-1.,1.37468482215751));
#45413=CARTESIAN_POINT('Ctrl Pts',(3.93135106761844,1.,1.37468482215751));
#45414=CARTESIAN_POINT('Ctrl Pts',(3.93912709040818,-1.,1.37381821967165));
#45415=CARTESIAN_POINT('Ctrl Pts',(3.93912709040818,1.,1.37381821967165));
#45416=CARTESIAN_POINT('Ctrl Pts',(3.94690771785133,-1.,1.37291699202807));
#45417=CARTESIAN_POINT('Ctrl Pts',(3.94690771785133,1.,1.37291699202807));
#45418=CARTESIAN_POINT('Ctrl Pts',(3.95469287280914,-1.,1.37198126432386));
#45419=CARTESIAN_POINT('Ctrl Pts',(3.95469287280914,1.,1.37198126432386));
#45420=CARTESIAN_POINT('Ctrl Pts',(3.96092458506535,-1.,1.3712051561502));
#45421=CARTESIAN_POINT('Ctrl Pts',(3.96092458506535,1.,1.3712051561502));
#45422=CARTESIAN_POINT('Ctrl Pts',(3.96560037974645,-1.,1.37060761745635));
#45423=CARTESIAN_POINT('Ctrl Pts',(3.96560037974645,1.,1.37060761745635));
#45424=CARTESIAN_POINT('Ctrl Pts',(3.9687184694131,-1.,1.37020239094614));
#45425=CARTESIAN_POINT('Ctrl Pts',(3.9687184694131,1.,1.37020239094614));
#45426=CARTESIAN_POINT('Ctrl Pts',(3.97027773754922,-1.,1.36999806084573));
#45427=CARTESIAN_POINT('Ctrl Pts',(3.97027773754922,1.,1.36999806084573));
#45428=CARTESIAN_POINT('',(3.4984457533445,1.,1.35032489087101));
#45429=CARTESIAN_POINT('Ctrl Pts',(3.4984457533445,-1.,1.35032489087101));
#45430=CARTESIAN_POINT('Ctrl Pts',(3.4984457533445,-0.666666666666667,1.35032489087101));
#45431=CARTESIAN_POINT('Ctrl Pts',(3.4984457533445,-0.333333333333333,1.35032489087101));
#45432=CARTESIAN_POINT('Ctrl Pts',(3.4984457533445,0.333333333333333,1.35032489087101));
#45433=CARTESIAN_POINT('Ctrl Pts',(3.4984457533445,0.666666666666667,1.35032489087101));
#45434=CARTESIAN_POINT('Ctrl Pts',(3.4984457533445,1.,1.35032489087101));
#45435=CARTESIAN_POINT('',(3.97027773754922,1.,1.36999806084573));
#45436=CARTESIAN_POINT('',(3.97027773754922,0.,1.36999806084573));
#45437=CARTESIAN_POINT('Ctrl Pts',(3.4984457533445,1.,1.35032489087101));
#45438=CARTESIAN_POINT('Ctrl Pts',(3.49847119623846,1.,1.35036670892966));
#45439=CARTESIAN_POINT('Ctrl Pts',(3.49861894124827,1.,1.35049736560527));
#45440=CARTESIAN_POINT('Ctrl Pts',(3.49920025459723,1.,1.35080045218587));
#45441=CARTESIAN_POINT('Ctrl Pts',(3.5007660381649,1.,1.35142377279517));
#45442=CARTESIAN_POINT('Ctrl Pts',(3.50408168106261,1.,1.35257032843486));
#45443=CARTESIAN_POINT('Ctrl Pts',(3.50913227059999,1.,1.35419113575956));
#45444=CARTESIAN_POINT('Ctrl Pts',(3.51542230699556,1.,1.35611275237152));
#45445=CARTESIAN_POINT('Ctrl Pts',(3.52261776116748,1.,1.35821701528836));
#45446=CARTESIAN_POINT('Ctrl Pts',(3.530344649616,1.,1.36037259643734));
#45447=CARTESIAN_POINT('Ctrl Pts',(3.53824396424961,1.,1.36245507339307));
#45448=CARTESIAN_POINT('Ctrl Pts',(3.54602591832973,1.,1.36436666257598));
#45449=CARTESIAN_POINT('Ctrl Pts',(3.55353883995949,1.,1.3660614545677));
#45450=CARTESIAN_POINT('Ctrl Pts',(3.56077662028649,1.,1.36754771771233));
#45451=CARTESIAN_POINT('Ctrl Pts',(3.5678208030466,1.,1.36886584973389));
#45452=CARTESIAN_POINT('Ctrl Pts',(3.57479875549486,1.,1.37007229485659));
#45453=CARTESIAN_POINT('Ctrl Pts',(3.58183885982715,1.,1.37122241663062));
#45454=CARTESIAN_POINT('Ctrl Pts',(3.58901853846365,1.,1.37235053660976));
#45455=CARTESIAN_POINT('Ctrl Pts',(3.59634627869048,1.,1.37346320103157));
#45456=CARTESIAN_POINT('Ctrl Pts',(3.60379020123988,1.,1.37455051379623));
#45457=CARTESIAN_POINT('Ctrl Pts',(3.61129546591064,1.,1.37559314436634));
#45458=CARTESIAN_POINT('Ctrl Pts',(3.6188048116042,1.,1.37657053403107));
#45459=CARTESIAN_POINT('Ctrl Pts',(3.62628098665145,1.,1.37746987919881));
#45460=CARTESIAN_POINT('Ctrl Pts',(3.63371727442486,1.,1.37829035457339));
#45461=CARTESIAN_POINT('Ctrl Pts',(3.64112507791141,1.,1.37903818567359));
#45462=CARTESIAN_POINT('Ctrl Pts',(3.64852652756456,1.,1.37972372481603));
#45463=CARTESIAN_POINT('Ctrl Pts',(3.6559455440439,1.,1.38035791051213));
#45464=CARTESIAN_POINT('Ctrl Pts',(3.66339848520857,1.,1.38094856333552));
#45465=CARTESIAN_POINT('Ctrl Pts',(3.67088843112262,1.,1.38149812653868));
#45466=CARTESIAN_POINT('Ctrl Pts',(3.67841038482414,1.,1.3820057429062));
#45467=CARTESIAN_POINT('Ctrl Pts',(3.68595444983837,1.,1.38246852827182));
#45468=CARTESIAN_POINT('Ctrl Pts',(3.69350967899526,1.,1.38288311171651));
#45469=CARTESIAN_POINT('Ctrl Pts',(3.701067921679,1.,1.38324717612865));
#45470=CARTESIAN_POINT('Ctrl Pts',(3.70862680753347,1.,1.38356065402124));
#45471=CARTESIAN_POINT('Ctrl Pts',(3.7161876605181,1.,1.38382489984586));
#45472=CARTESIAN_POINT('Ctrl Pts',(3.72375409358803,1.,1.3840421342895));
#45473=CARTESIAN_POINT('Ctrl Pts',(3.73133035859282,1.,1.38421479111531));
#45474=CARTESIAN_POINT('Ctrl Pts',(3.73891976418104,1.,1.38434489156458));
#45475=CARTESIAN_POINT('Ctrl Pts',(3.74652317167876,1.,1.38443344984394));
#45476=CARTESIAN_POINT('Ctrl Pts',(3.7541397631875,1.,1.38448077997163));
#45477=CARTESIAN_POINT('Ctrl Pts',(3.76176768271367,1.,1.3844867525335));
#45478=CARTESIAN_POINT('Ctrl Pts',(3.76940473185779,1.,1.38445107339518));
#45479=CARTESIAN_POINT('Ctrl Pts',(3.77704902230418,1.,1.38437354551428));
#45480=CARTESIAN_POINT('Ctrl Pts',(3.78469969805082,1.,1.38425435883756));
#45481=CARTESIAN_POINT('Ctrl Pts',(3.79235669640841,1.,1.38409399694566));
#45482=CARTESIAN_POINT('Ctrl Pts',(3.80002044322111,1.,1.38389311766682));
#45483=CARTESIAN_POINT('Ctrl Pts',(3.80769156398411,1.,1.3836524404622));
#45484=CARTESIAN_POINT('Ctrl Pts',(3.81537060817811,1.,1.38337263902782));
#45485=CARTESIAN_POINT('Ctrl Pts',(3.82305771743829,1.,1.38305421262763));
#45486=CARTESIAN_POINT('Ctrl Pts',(3.8307526698229,1.,1.38269750245138));
#45487=CARTESIAN_POINT('Ctrl Pts',(3.83845502790746,1.,1.38230274828822));
#45488=CARTESIAN_POINT('Ctrl Pts',(3.84616425605764,1.,1.38187013346109));
#45489=CARTESIAN_POINT('Ctrl Pts',(3.85387983979481,1.,1.3813998311505));
#45490=CARTESIAN_POINT('Ctrl Pts',(3.86160143043959,1.,1.3808920599299));
#45491=CARTESIAN_POINT('Ctrl Pts',(3.86932885813068,1.,1.38034709213014));
#45492=CARTESIAN_POINT('Ctrl Pts',(3.87706205830532,1.,1.37976523097073));
#45493=CARTESIAN_POINT('Ctrl Pts',(3.88480102249277,1.,1.37914679719383));
#45494=CARTESIAN_POINT('Ctrl Pts',(3.89254574338496,1.,1.3784921128802));
#45495=CARTESIAN_POINT('Ctrl Pts',(3.90029615196727,1.,1.37780148512792));
#45496=CARTESIAN_POINT('Ctrl Pts',(3.90805209523486,1.,1.3770751963402));
#45497=CARTESIAN_POINT('Ctrl Pts',(3.91581337462644,1.,1.37631350505797));
#45498=CARTESIAN_POINT('Ctrl Pts',(3.92357976987672,1.,1.37551664448242));
#45499=CARTESIAN_POINT('Ctrl Pts',(3.93135106761844,1.,1.37468482215751));
#45500=CARTESIAN_POINT('Ctrl Pts',(3.93912709040818,1.,1.37381821967165));
#45501=CARTESIAN_POINT('Ctrl Pts',(3.94690771785133,1.,1.37291699202807));
#45502=CARTESIAN_POINT('Ctrl Pts',(3.95469287280914,1.,1.37198126432386));
#45503=CARTESIAN_POINT('Ctrl Pts',(3.96092458506535,1.,1.3712051561502));
#45504=CARTESIAN_POINT('Ctrl Pts',(3.96560037974645,1.,1.37060761745635));
#45505=CARTESIAN_POINT('Ctrl Pts',(3.9687184694131,1.,1.37020239094614));
#45506=CARTESIAN_POINT('Ctrl Pts',(3.97027773754922,1.,1.36999806084573));
#45507=CARTESIAN_POINT('Origin',(3.97027773754922,0.,1.36999806084573));
#45508=CARTESIAN_POINT('',(4.01728681790024,1.,1.22531898815164));
#45509=CARTESIAN_POINT('Origin',(0.,0.,0.));
#45510=CARTESIAN_POINT('',(3.42859860294378,1.,1.51895082866166));
#45511=CARTESIAN_POINT('Origin',(0.,1.,0.));
#45512=CARTESIAN_POINT('Ctrl Pts',(3.42859860294378,1.,1.51895082866166));
#45513=CARTESIAN_POINT('Ctrl Pts',(3.42859860294378,0.666666666666667,1.51895082866166));
#45514=CARTESIAN_POINT('Ctrl Pts',(3.42859860294378,0.333333333333333,1.51895082866166));
#45515=CARTESIAN_POINT('Ctrl Pts',(3.42859860294378,-0.333333333333333,
1.51895082866166));
#45516=CARTESIAN_POINT('Ctrl Pts',(3.42859860294378,-0.666666666666667,
1.51895082866166));
#45517=CARTESIAN_POINT('Ctrl Pts',(3.42859860294378,-1.,1.51895082866166));
#45518=CARTESIAN_POINT('Ctrl Pts',(3.77614523045147,-1.,1.83867539237861));
#45519=CARTESIAN_POINT('Ctrl Pts',(3.77614523045147,1.,1.83867539237861));
#45520=CARTESIAN_POINT('Ctrl Pts',(3.77518714458232,-1.,1.83742834010821));
#45521=CARTESIAN_POINT('Ctrl Pts',(3.77518714458232,1.,1.83742834010821));
#45522=CARTESIAN_POINT('Ctrl Pts',(3.77326886065484,-1.,1.83493697935064));
#45523=CARTESIAN_POINT('Ctrl Pts',(3.77326886065484,1.,1.83493697935064));
#45524=CARTESIAN_POINT('Ctrl Pts',(3.77038509819777,-1.,1.83120816956515));
#45525=CARTESIAN_POINT('Ctrl Pts',(3.77038509819777,1.,1.83120816956515));
#45526=CARTESIAN_POINT('Ctrl Pts',(3.76652740355856,-1.,1.82625289221933));
#45527=CARTESIAN_POINT('Ctrl Pts',(3.76652740355856,1.,1.82625289221933));
#45528=CARTESIAN_POINT('Ctrl Pts',(3.76168412709652,-1.,1.82008629694924));
#45529=CARTESIAN_POINT('Ctrl Pts',(3.76168412709652,1.,1.82008629694924));
#45530=CARTESIAN_POINT('Ctrl Pts',(3.75681965683995,-1.,1.81394729834032));
#45531=CARTESIAN_POINT('Ctrl Pts',(3.75681965683995,1.,1.81394729834032));
#45532=CARTESIAN_POINT('Ctrl Pts',(3.75193395888069,-1.,1.80783603939662));
#45533=CARTESIAN_POINT('Ctrl Pts',(3.75193395888069,1.,1.80783603939662));
#45534=CARTESIAN_POINT('Ctrl Pts',(3.74702700874954,-1.,1.80175271485519));
#45535=CARTESIAN_POINT('Ctrl Pts',(3.74702700874954,1.,1.80175271485519));
#45536=CARTESIAN_POINT('Ctrl Pts',(3.74209880351667,-1.,1.79569757859041));
#45537=CARTESIAN_POINT('Ctrl Pts',(3.74209880351667,1.,1.79569757859041));
#45538=CARTESIAN_POINT('Ctrl Pts',(3.73714934729962,-1.,1.78967092823139));
#45539=CARTESIAN_POINT('Ctrl Pts',(3.73714934729962,1.,1.78967092823139));
#45540=CARTESIAN_POINT('Ctrl Pts',(3.73217863095022,-1.,1.78367308442682));
#45541=CARTESIAN_POINT('Ctrl Pts',(3.73217863095022,1.,1.78367308442682));
#45542=CARTESIAN_POINT('Ctrl Pts',(3.72718661205504,-1.,1.77770437039606));
#45543=CARTESIAN_POINT('Ctrl Pts',(3.72718661205504,1.,1.77770437039606));
#45544=CARTESIAN_POINT('Ctrl Pts',(3.72217319911429,-1.,1.77176509401846));
#45545=CARTESIAN_POINT('Ctrl Pts',(3.72217319911429,1.,1.77176509401846));
#45546=CARTESIAN_POINT('Ctrl Pts',(3.71713822377675,-1.,1.76585552124549));
#45547=CARTESIAN_POINT('Ctrl Pts',(3.71713822377675,1.,1.76585552124549));
#45548=CARTESIAN_POINT('Ctrl Pts',(3.71208146346454,-1.,1.75997588499021));
#45549=CARTESIAN_POINT('Ctrl Pts',(3.71208146346454,1.,1.75997588499021));
#45550=CARTESIAN_POINT('Ctrl Pts',(3.70700269736876,-1.,1.75412641804148));
#45551=CARTESIAN_POINT('Ctrl Pts',(3.70700269736876,1.,1.75412641804148));
#45552=CARTESIAN_POINT('Ctrl Pts',(3.70190175673422,-1.,1.74830738046092));
#45553=CARTESIAN_POINT('Ctrl Pts',(3.70190175673422,1.,1.74830738046092));
#45554=CARTESIAN_POINT('Ctrl Pts',(3.6967785691046,-1.,1.74251908492589));
#45555=CARTESIAN_POINT('Ctrl Pts',(3.6967785691046,1.,1.74251908492589));
#45556=CARTESIAN_POINT('Ctrl Pts',(3.69163322647906,-1.,1.73676193254493));
#45557=CARTESIAN_POINT('Ctrl Pts',(3.69163322647906,1.,1.73676193254493));
#45558=CARTESIAN_POINT('Ctrl Pts',(3.68646597019188,-1.,1.73103640956647));
#45559=CARTESIAN_POINT('Ctrl Pts',(3.68646597019188,1.,1.73103640956647));
#45560=CARTESIAN_POINT('Ctrl Pts',(3.68127704936472,-1.,1.72534302437003));
#45561=CARTESIAN_POINT('Ctrl Pts',(3.68127704936472,1.,1.72534302437003));
#45562=CARTESIAN_POINT('Ctrl Pts',(3.67606660374665,-1.,1.71968225581787));
#45563=CARTESIAN_POINT('Ctrl Pts',(3.67606660374665,1.,1.71968225581787));
#45564=CARTESIAN_POINT('Ctrl Pts',(3.67083454901629,-1.,1.71405450210392));
#45565=CARTESIAN_POINT('Ctrl Pts',(3.67083454901629,1.,1.71405450210392));
#45566=CARTESIAN_POINT('Ctrl Pts',(3.6655804319893,-1.,1.70846001610983));
#45567=CARTESIAN_POINT('Ctrl Pts',(3.6655804319893,1.,1.70846001610983));
#45568=CARTESIAN_POINT('Ctrl Pts',(3.6603033877491,-1.,1.70289888566904));
#45569=CARTESIAN_POINT('Ctrl Pts',(3.6603033877491,1.,1.70289888566904));
#45570=CARTESIAN_POINT('Ctrl Pts',(3.65500246526798,-1.,1.69737117722559));
#45571=CARTESIAN_POINT('Ctrl Pts',(3.65500246526798,1.,1.69737117722559));
#45572=CARTESIAN_POINT('Ctrl Pts',(3.64967689827393,-1.,1.691877054817));
#45573=CARTESIAN_POINT('Ctrl Pts',(3.64967689827393,1.,1.691877054817));
#45574=CARTESIAN_POINT('Ctrl Pts',(3.64432638915199,-1.,1.68641690471455));
#45575=CARTESIAN_POINT('Ctrl Pts',(3.64432638915199,1.,1.68641690471455));
#45576=CARTESIAN_POINT('Ctrl Pts',(3.63895140887443,-1.,1.68099146651577));
#45577=CARTESIAN_POINT('Ctrl Pts',(3.63895140887443,1.,1.68099146651577));
#45578=CARTESIAN_POINT('Ctrl Pts',(3.63355343201211,-1.,1.67560193613145));
#45579=CARTESIAN_POINT('Ctrl Pts',(3.63355343201211,1.,1.67560193613145));
#45580=CARTESIAN_POINT('Ctrl Pts',(3.62813422105257,-1.,1.67024966008037));
#45581=CARTESIAN_POINT('Ctrl Pts',(3.62813422105257,1.,1.67024966008037));
#45582=CARTESIAN_POINT('Ctrl Pts',(3.62269517989104,-1.,1.66493585923853));
#45583=CARTESIAN_POINT('Ctrl Pts',(3.62269517989104,1.,1.66493585923853));
#45584=CARTESIAN_POINT('Ctrl Pts',(3.61723666482457,-1.,1.65966133399186));
#45585=CARTESIAN_POINT('Ctrl Pts',(3.61723666482457,1.,1.65966133399186));
#45586=CARTESIAN_POINT('Ctrl Pts',(3.61175734965129,-1.,1.65442619244327));
#45587=CARTESIAN_POINT('Ctrl Pts',(3.61175734965129,1.,1.65442619244327));
#45588=CARTESIAN_POINT('Ctrl Pts',(3.60625346556992,-1.,1.64922952425833));
#45589=CARTESIAN_POINT('Ctrl Pts',(3.60625346556992,1.,1.64922952425833));
#45590=CARTESIAN_POINT('Ctrl Pts',(3.6007202851384,-1.,1.6440700438558));
#45591=CARTESIAN_POINT('Ctrl Pts',(3.6007202851384,1.,1.6440700438558));
#45592=CARTESIAN_POINT('Ctrl Pts',(3.59515368334887,-1.,1.63894676675349));
#45593=CARTESIAN_POINT('Ctrl Pts',(3.59515368334887,1.,1.63894676675349));
#45594=CARTESIAN_POINT('Ctrl Pts',(3.58955176627876,-1.,1.63385971451259));
#45595=CARTESIAN_POINT('Ctrl Pts',(3.58955176627876,1.,1.63385971451259));
#45596=CARTESIAN_POINT('Ctrl Pts',(3.5839162577435,-1.,1.62881051550748));
#45597=CARTESIAN_POINT('Ctrl Pts',(3.5839162577435,1.,1.62881051550748));
#45598=CARTESIAN_POINT('Ctrl Pts',(3.57825455954405,-1.,1.62380329464851));
#45599=CARTESIAN_POINT('Ctrl Pts',(3.57825455954405,1.,1.62380329464851));
#45600=CARTESIAN_POINT('Ctrl Pts',(3.57257679609826,-1.,1.61884340915412));
#45601=CARTESIAN_POINT('Ctrl Pts',(3.57257679609826,1.,1.61884340915412));
#45602=CARTESIAN_POINT('Ctrl Pts',(3.56689200468404,-1.,1.61393581747522));
#45603=CARTESIAN_POINT('Ctrl Pts',(3.56689200468404,1.,1.61393581747522));
#45604=CARTESIAN_POINT('Ctrl Pts',(3.56120432482986,-1.,1.60908344685459));
#45605=CARTESIAN_POINT('Ctrl Pts',(3.56120432482986,1.,1.60908344685459));
#45606=CARTESIAN_POINT('Ctrl Pts',(3.55550985096117,-1.,1.60428584699848));
#45607=CARTESIAN_POINT('Ctrl Pts',(3.55550985096117,1.,1.60428584699848));
#45608=CARTESIAN_POINT('Ctrl Pts',(3.54979148634426,-1.,1.59953698113444));
#45609=CARTESIAN_POINT('Ctrl Pts',(3.54979148634426,1.,1.59953698113444));
#45610=CARTESIAN_POINT('Ctrl Pts',(3.544024581823,-1.,1.5948276694975));
#45611=CARTESIAN_POINT('Ctrl Pts',(3.544024581823,1.,1.5948276694975));
#45612=CARTESIAN_POINT('Ctrl Pts',(3.53818616861045,-1.,1.59014958368725));
#45613=CARTESIAN_POINT('Ctrl Pts',(3.53818616861045,1.,1.59014958368725));
#45614=CARTESIAN_POINT('Ctrl Pts',(3.53226378147068,-1.,1.58549906268083));
#45615=CARTESIAN_POINT('Ctrl Pts',(3.53226378147068,1.,1.58549906268083));
#45616=CARTESIAN_POINT('Ctrl Pts',(3.52626275334899,-1.,1.58088027227856));
#45617=CARTESIAN_POINT('Ctrl Pts',(3.52626275334899,1.,1.58088027227856));
#45618=CARTESIAN_POINT('Ctrl Pts',(3.52021847865961,-1.,1.5763104998818));
#45619=CARTESIAN_POINT('Ctrl Pts',(3.52021847865961,1.,1.5763104998818));
#45620=CARTESIAN_POINT('Ctrl Pts',(3.51418598431733,-1.,1.57181569799774));
#45621=CARTESIAN_POINT('Ctrl Pts',(3.51418598431733,1.,1.57181569799774));
#45622=CARTESIAN_POINT('Ctrl Pts',(3.50821771695427,-1.,1.56742097575041));
#45623=CARTESIAN_POINT('Ctrl Pts',(3.50821771695427,1.,1.56742097575041));
#45624=CARTESIAN_POINT('Ctrl Pts',(3.50234321621607,-1.,1.56314187758689));
#45625=CARTESIAN_POINT('Ctrl Pts',(3.50234321621607,1.,1.56314187758689));
#45626=CARTESIAN_POINT('Ctrl Pts',(3.49655185179623,-1.,1.55897703097859));
#45627=CARTESIAN_POINT('Ctrl Pts',(3.49655185179623,1.,1.55897703097859));
#45628=CARTESIAN_POINT('Ctrl Pts',(3.49076460877317,-1.,1.5548959590107));
#45629=CARTESIAN_POINT('Ctrl Pts',(3.49076460877317,1.,1.5548959590107));
#45630=CARTESIAN_POINT('Ctrl Pts',(3.48485155928414,-1.,1.55084702970382));
#45631=CARTESIAN_POINT('Ctrl Pts',(3.48485155928414,1.,1.55084702970382));
#45632=CARTESIAN_POINT('Ctrl Pts',(3.47868272898599,-1.,1.54678009290207));
#45633=CARTESIAN_POINT('Ctrl Pts',(3.47868272898599,1.,1.54678009290207));
#45634=CARTESIAN_POINT('Ctrl Pts',(3.47217189224576,-1.,1.54266605398152));
#45635=CARTESIAN_POINT('Ctrl Pts',(3.47217189224576,1.,1.54266605398152));
#45636=CARTESIAN_POINT('Ctrl Pts',(3.46531752207222,-1.,1.53851507915533));
#45637=CARTESIAN_POINT('Ctrl Pts',(3.46531752207222,1.,1.53851507915533));
#45638=CARTESIAN_POINT('Ctrl Pts',(3.45825932955273,-1.,1.53440195378902));
#45639=CARTESIAN_POINT('Ctrl Pts',(3.45825932955273,1.,1.53440195378902));
#45640=CARTESIAN_POINT('Ctrl Pts',(3.45127136828667,-1.,1.530462444618));
#45641=CARTESIAN_POINT('Ctrl Pts',(3.45127136828667,1.,1.530462444618));
#45642=CARTESIAN_POINT('Ctrl Pts',(3.44469547527,-1.,1.52686242875717));
#45643=CARTESIAN_POINT('Ctrl Pts',(3.44469547527,1.,1.52686242875717));
#45644=CARTESIAN_POINT('Ctrl Pts',(3.43888895974182,-1.,1.52377348950429));
#45645=CARTESIAN_POINT('Ctrl Pts',(3.43888895974182,1.,1.52377348950429));
#45646=CARTESIAN_POINT('Ctrl Pts',(3.43417156977749,-1.,1.52134826724227));
#45647=CARTESIAN_POINT('Ctrl Pts',(3.43417156977749,1.,1.52134826724227));
#45648=CARTESIAN_POINT('Ctrl Pts',(3.43076036253384,-1.,1.51969006980792));
#45649=CARTESIAN_POINT('Ctrl Pts',(3.43076036253384,1.,1.51969006980792));
#45650=CARTESIAN_POINT('Ctrl Pts',(3.42915787669388,-1.,1.51901585838879));
#45651=CARTESIAN_POINT('Ctrl Pts',(3.42915787669388,1.,1.51901585838879));
#45652=CARTESIAN_POINT('Ctrl Pts',(3.42860527148835,-1.,1.51888450659497));
#45653=CARTESIAN_POINT('Ctrl Pts',(3.42860527148835,1.,1.51888450659497));
#45654=CARTESIAN_POINT('Ctrl Pts',(3.42852521763648,-1.,1.51896318668306));
#45655=CARTESIAN_POINT('Ctrl Pts',(3.42852521763648,1.,1.51896318668306));
#45656=CARTESIAN_POINT('Ctrl Pts',(3.42855728381368,-1.,1.519044091397));
#45657=CARTESIAN_POINT('Ctrl Pts',(3.42855728381368,1.,1.519044091397));
#45658=CARTESIAN_POINT('',(3.77614523045147,1.,1.83867539237861));
#45659=CARTESIAN_POINT('Ctrl Pts',(3.77614523045147,1.,1.83867539237861));
#45660=CARTESIAN_POINT('Ctrl Pts',(3.77518714458232,1.,1.83742834010821));
#45661=CARTESIAN_POINT('Ctrl Pts',(3.77326886065484,1.,1.83493697935064));
#45662=CARTESIAN_POINT('Ctrl Pts',(3.77038509819777,1.,1.83120816956515));
#45663=CARTESIAN_POINT('Ctrl Pts',(3.76652740355856,1.,1.82625289221933));
#45664=CARTESIAN_POINT('Ctrl Pts',(3.76168412709652,1.,1.82008629694924));
#45665=CARTESIAN_POINT('Ctrl Pts',(3.75681965683995,1.,1.81394729834032));
#45666=CARTESIAN_POINT('Ctrl Pts',(3.75193395888069,1.,1.80783603939662));
#45667=CARTESIAN_POINT('Ctrl Pts',(3.74702700874954,1.,1.80175271485519));
#45668=CARTESIAN_POINT('Ctrl Pts',(3.74209880351667,1.,1.79569757859041));
#45669=CARTESIAN_POINT('Ctrl Pts',(3.73714934729962,1.,1.78967092823139));
#45670=CARTESIAN_POINT('Ctrl Pts',(3.73217863095022,1.,1.78367308442682));
#45671=CARTESIAN_POINT('Ctrl Pts',(3.72718661205504,1.,1.77770437039606));
#45672=CARTESIAN_POINT('Ctrl Pts',(3.72217319911429,1.,1.77176509401846));
#45673=CARTESIAN_POINT('Ctrl Pts',(3.71713822377675,1.,1.76585552124549));
#45674=CARTESIAN_POINT('Ctrl Pts',(3.71208146346454,1.,1.75997588499021));
#45675=CARTESIAN_POINT('Ctrl Pts',(3.70700269736876,1.,1.75412641804148));
#45676=CARTESIAN_POINT('Ctrl Pts',(3.70190175673422,1.,1.74830738046092));
#45677=CARTESIAN_POINT('Ctrl Pts',(3.6967785691046,1.,1.74251908492589));
#45678=CARTESIAN_POINT('Ctrl Pts',(3.69163322647906,1.,1.73676193254493));
#45679=CARTESIAN_POINT('Ctrl Pts',(3.68646597019188,1.,1.73103640956647));
#45680=CARTESIAN_POINT('Ctrl Pts',(3.68127704936472,1.,1.72534302437003));
#45681=CARTESIAN_POINT('Ctrl Pts',(3.67606660374665,1.,1.71968225581787));
#45682=CARTESIAN_POINT('Ctrl Pts',(3.67083454901629,1.,1.71405450210392));
#45683=CARTESIAN_POINT('Ctrl Pts',(3.6655804319893,1.,1.70846001610983));
#45684=CARTESIAN_POINT('Ctrl Pts',(3.6603033877491,1.,1.70289888566904));
#45685=CARTESIAN_POINT('Ctrl Pts',(3.65500246526798,1.,1.69737117722559));
#45686=CARTESIAN_POINT('Ctrl Pts',(3.64967689827393,1.,1.691877054817));
#45687=CARTESIAN_POINT('Ctrl Pts',(3.64432638915199,1.,1.68641690471455));
#45688=CARTESIAN_POINT('Ctrl Pts',(3.63895140887443,1.,1.68099146651577));
#45689=CARTESIAN_POINT('Ctrl Pts',(3.63355343201211,1.,1.67560193613145));
#45690=CARTESIAN_POINT('Ctrl Pts',(3.62813422105257,1.,1.67024966008037));
#45691=CARTESIAN_POINT('Ctrl Pts',(3.62269517989104,1.,1.66493585923853));
#45692=CARTESIAN_POINT('Ctrl Pts',(3.61723666482457,1.,1.65966133399186));
#45693=CARTESIAN_POINT('Ctrl Pts',(3.61175734965129,1.,1.65442619244327));
#45694=CARTESIAN_POINT('Ctrl Pts',(3.60625346556992,1.,1.64922952425833));
#45695=CARTESIAN_POINT('Ctrl Pts',(3.6007202851384,1.,1.6440700438558));
#45696=CARTESIAN_POINT('Ctrl Pts',(3.59515368334887,1.,1.63894676675349));
#45697=CARTESIAN_POINT('Ctrl Pts',(3.58955176627876,1.,1.63385971451259));
#45698=CARTESIAN_POINT('Ctrl Pts',(3.5839162577435,1.,1.62881051550748));
#45699=CARTESIAN_POINT('Ctrl Pts',(3.57825455954405,1.,1.62380329464851));
#45700=CARTESIAN_POINT('Ctrl Pts',(3.57257679609826,1.,1.61884340915412));
#45701=CARTESIAN_POINT('Ctrl Pts',(3.56689200468404,1.,1.61393581747522));
#45702=CARTESIAN_POINT('Ctrl Pts',(3.56120432482986,1.,1.60908344685459));
#45703=CARTESIAN_POINT('Ctrl Pts',(3.55550985096117,1.,1.60428584699848));
#45704=CARTESIAN_POINT('Ctrl Pts',(3.54979148634426,1.,1.59953698113444));
#45705=CARTESIAN_POINT('Ctrl Pts',(3.544024581823,1.,1.5948276694975));
#45706=CARTESIAN_POINT('Ctrl Pts',(3.53818616861045,1.,1.59014958368725));
#45707=CARTESIAN_POINT('Ctrl Pts',(3.53226378147068,1.,1.58549906268083));
#45708=CARTESIAN_POINT('Ctrl Pts',(3.52626275334899,1.,1.58088027227856));
#45709=CARTESIAN_POINT('Ctrl Pts',(3.52021847865961,1.,1.5763104998818));
#45710=CARTESIAN_POINT('Ctrl Pts',(3.51418598431733,1.,1.57181569799774));
#45711=CARTESIAN_POINT('Ctrl Pts',(3.50821771695427,1.,1.56742097575041));
#45712=CARTESIAN_POINT('Ctrl Pts',(3.50234321621607,1.,1.56314187758689));
#45713=CARTESIAN_POINT('Ctrl Pts',(3.49655185179623,1.,1.55897703097859));
#45714=CARTESIAN_POINT('Ctrl Pts',(3.49076460877317,1.,1.5548959590107));
#45715=CARTESIAN_POINT('Ctrl Pts',(3.48485155928414,1.,1.55084702970382));
#45716=CARTESIAN_POINT('Ctrl Pts',(3.47868272898599,1.,1.54678009290207));
#45717=CARTESIAN_POINT('Ctrl Pts',(3.47217189224576,1.,1.54266605398152));
#45718=CARTESIAN_POINT('Ctrl Pts',(3.46531752207222,1.,1.53851507915533));
#45719=CARTESIAN_POINT('Ctrl Pts',(3.45825932955273,1.,1.53440195378902));
#45720=CARTESIAN_POINT('Ctrl Pts',(3.45127136828667,1.,1.530462444618));
#45721=CARTESIAN_POINT('Ctrl Pts',(3.44469547527,1.,1.52686242875717));
#45722=CARTESIAN_POINT('Ctrl Pts',(3.43888895974182,1.,1.52377348950429));
#45723=CARTESIAN_POINT('Ctrl Pts',(3.43417156977749,1.,1.52134826724227));
#45724=CARTESIAN_POINT('Ctrl Pts',(3.4310163189349,1.,1.5198144909343));
#45725=CARTESIAN_POINT('Ctrl Pts',(3.42946838852728,1.,1.51914806898539));
#45726=CARTESIAN_POINT('Ctrl Pts',(3.42884302333978,1.,1.51895133295017));
#45727=CARTESIAN_POINT('Ctrl Pts',(3.42864616361967,1.,1.51893924967231));
#45728=CARTESIAN_POINT('Ctrl Pts',(3.42859860294378,1.,1.51895082866166));
#45729=CARTESIAN_POINT('',(3.77614523045147,0.,1.83867539237861));
#45730=CARTESIAN_POINT('Ctrl Pts',(3.24418789321065,-1.,1.88088939428811));
#45731=CARTESIAN_POINT('Ctrl Pts',(3.24418789321065,1.,1.88088939428811));
#45732=CARTESIAN_POINT('Ctrl Pts',(3.24410359189733,-1.,1.8809110068042));
#45733=CARTESIAN_POINT('Ctrl Pts',(3.24410359189733,1.,1.8809110068042));
#45734=CARTESIAN_POINT('Ctrl Pts',(3.24408699284449,-1.,1.8810220187274));
#45735=CARTESIAN_POINT('Ctrl Pts',(3.24408699284449,1.,1.8810220187274));
#45736=CARTESIAN_POINT('Ctrl Pts',(3.24451807186964,-1.,1.88139187908347));
#45737=CARTESIAN_POINT('Ctrl Pts',(3.24451807186964,1.,1.88139187908347));
#45738=CARTESIAN_POINT('Ctrl Pts',(3.24600543790876,-1.,1.88229202583187));
#45739=CARTESIAN_POINT('Ctrl Pts',(3.24600543790876,1.,1.88229202583187));
#45740=CARTESIAN_POINT('Ctrl Pts',(3.24935200512055,-1.,1.88407708646435));
#45741=CARTESIAN_POINT('Ctrl Pts',(3.24935200512055,1.,1.88407708646435));
#45742=CARTESIAN_POINT('Ctrl Pts',(3.25408686339298,-1.,1.88646802523372));
#45743=CARTESIAN_POINT('Ctrl Pts',(3.25408686339298,1.,1.88646802523372));
#45744=CARTESIAN_POINT('Ctrl Pts',(3.2599988519361,-1.,1.88934996203508));
#45745=CARTESIAN_POINT('Ctrl Pts',(3.2599988519361,1.,1.88934996203508));
#45746=CARTESIAN_POINT('Ctrl Pts',(3.2667765388833,-1.,1.89255393500769));
#45747=CARTESIAN_POINT('Ctrl Pts',(3.2667765388833,1.,1.89255393500769));
#45748=CARTESIAN_POINT('Ctrl Pts',(3.27407108932908,-1.,1.89589172903662));
#45749=CARTESIAN_POINT('Ctrl Pts',(3.27407108932908,1.,1.89589172903662));
#45750=CARTESIAN_POINT('Ctrl Pts',(3.28154737912287,-1.,1.89918429230425));
#45751=CARTESIAN_POINT('Ctrl Pts',(3.28154737912287,1.,1.89918429230425));
#45752=CARTESIAN_POINT('Ctrl Pts',(3.28893448600364,-1.,1.9022897124757));
#45753=CARTESIAN_POINT('Ctrl Pts',(3.28893448600364,1.,1.9022897124757));
#45754=CARTESIAN_POINT('Ctrl Pts',(3.29608978722258,-1.,1.9051389186417));
#45755=CARTESIAN_POINT('Ctrl Pts',(3.29608978722258,1.,1.9051389186417));
#45756=CARTESIAN_POINT('Ctrl Pts',(3.30300595568341,-1.,1.90773912171424));
#45757=CARTESIAN_POINT('Ctrl Pts',(3.30300595568341,1.,1.90773912171424));
#45758=CARTESIAN_POINT('Ctrl Pts',(3.30975721158694,-1.,1.91014297830502));
#45759=CARTESIAN_POINT('Ctrl Pts',(3.30975721158694,1.,1.91014297830502));
#45760=CARTESIAN_POINT('Ctrl Pts',(3.31646052426395,-1.,1.91242616234459));
#45761=CARTESIAN_POINT('Ctrl Pts',(3.31646052426395,1.,1.91242616234459));
#45762=CARTESIAN_POINT('Ctrl Pts',(3.32323403454507,-1.,1.91466343916612));
#45763=CARTESIAN_POINT('Ctrl Pts',(3.32323403454507,1.,1.91466343916612));
#45764=CARTESIAN_POINT('Ctrl Pts',(3.33014884257812,-1.,1.91690081930297));
#45765=CARTESIAN_POINT('Ctrl Pts',(3.33014884257812,1.,1.91690081930297));
#45766=CARTESIAN_POINT('Ctrl Pts',(3.33721230709948,-1.,1.91914609610173));
#45767=CARTESIAN_POINT('Ctrl Pts',(3.33721230709948,1.,1.91914609610173));
#45768=CARTESIAN_POINT('Ctrl Pts',(3.34439448941915,-1.,1.92138450828378));
#45769=CARTESIAN_POINT('Ctrl Pts',(3.34439448941915,1.,1.92138450828378));
#45770=CARTESIAN_POINT('Ctrl Pts',(3.35164424847206,-1.,1.92358838440518));
#45771=CARTESIAN_POINT('Ctrl Pts',(3.35164424847206,1.,1.92358838440518));
#45772=CARTESIAN_POINT('Ctrl Pts',(3.35890824422976,-1.,1.92572846125763));
#45773=CARTESIAN_POINT('Ctrl Pts',(3.35890824422976,1.,1.92572846125763));
#45774=CARTESIAN_POINT('Ctrl Pts',(3.36615168657597,-1.,1.92778626543803));
#45775=CARTESIAN_POINT('Ctrl Pts',(3.36615168657597,1.,1.92778626543803));
#45776=CARTESIAN_POINT('Ctrl Pts',(3.37336807068078,-1.,1.92975993109897));
#45777=CARTESIAN_POINT('Ctrl Pts',(3.37336807068078,1.,1.92975993109897));
#45778=CARTESIAN_POINT('Ctrl Pts',(3.38056768525577,-1.,1.93165739093292));
#45779=CARTESIAN_POINT('Ctrl Pts',(3.38056768525577,1.,1.93165739093292));
#45780=CARTESIAN_POINT('Ctrl Pts',(3.38777076883267,-1.,1.93349233176794));
#45781=CARTESIAN_POINT('Ctrl Pts',(3.38777076883267,1.,1.93349233176794));
#45782=CARTESIAN_POINT('Ctrl Pts',(3.39499923640789,-1.,1.93527929945982));
#45783=CARTESIAN_POINT('Ctrl Pts',(3.39499923640789,1.,1.93527929945982));
#45784=CARTESIAN_POINT('Ctrl Pts',(3.40226802104093,-1.,1.93702857723089));
#45785=CARTESIAN_POINT('Ctrl Pts',(3.40226802104093,1.,1.93702857723089));
#45786=CARTESIAN_POINT('Ctrl Pts',(3.40957978266622,-1.,1.93874306008132));
#45787=CARTESIAN_POINT('Ctrl Pts',(3.40957978266622,1.,1.93874306008132));
#45788=CARTESIAN_POINT('Ctrl Pts',(3.41692971994082,-1.,1.94042111965237));
#45789=CARTESIAN_POINT('Ctrl Pts',(3.41692971994082,1.,1.94042111965237));
#45790=CARTESIAN_POINT('Ctrl Pts',(3.42430850941497,-1.,1.94205835913692));
#45791=CARTESIAN_POINT('Ctrl Pts',(3.42430850941497,1.,1.94205835913692));
#45792=CARTESIAN_POINT('Ctrl Pts',(3.43170586602436,-1.,1.94364973660285));
#45793=CARTESIAN_POINT('Ctrl Pts',(3.43170586602436,1.,1.94364973660285));
#45794=CARTESIAN_POINT('Ctrl Pts',(3.43911410197693,-1.,1.94519168842883));
#45795=CARTESIAN_POINT('Ctrl Pts',(3.43911410197693,1.,1.94519168842883));
#45796=CARTESIAN_POINT('Ctrl Pts',(3.44653088665685,-1.,1.94668377715332));
#45797=CARTESIAN_POINT('Ctrl Pts',(3.44653088665685,1.,1.94668377715332));
#45798=CARTESIAN_POINT('Ctrl Pts',(3.45395731584051,-1.,1.94812754766524));
#45799=CARTESIAN_POINT('Ctrl Pts',(3.45395731584051,1.,1.94812754766524));
#45800=CARTESIAN_POINT('Ctrl Pts',(3.46139661060959,-1.,1.94952575850196));
#45801=CARTESIAN_POINT('Ctrl Pts',(3.46139661060959,1.,1.94952575850196));
#45802=CARTESIAN_POINT('Ctrl Pts',(3.4688525897419,-1.,1.95088147859876));
#45803=CARTESIAN_POINT('Ctrl Pts',(3.4688525897419,1.,1.95088147859876));
#45804=CARTESIAN_POINT('Ctrl Pts',(3.47632820495926,-1.,1.95219722189878));
#45805=CARTESIAN_POINT('Ctrl Pts',(3.47632820495926,1.,1.95219722189878));
#45806=CARTESIAN_POINT('Ctrl Pts',(3.48382414832648,-1.,1.95347412486316));
#45807=CARTESIAN_POINT('Ctrl Pts',(3.48382414832648,1.,1.95347412486316));
#45808=CARTESIAN_POINT('Ctrl Pts',(3.49133956289154,-1.,1.95471236969653));
#45809=CARTESIAN_POINT('Ctrl Pts',(3.49133956289154,1.,1.95471236969653));
#45810=CARTESIAN_POINT('Ctrl Pts',(3.49887263575602,-1.,1.9559115382367));
#45811=CARTESIAN_POINT('Ctrl Pts',(3.49887263575602,1.,1.9559115382367));
#45812=CARTESIAN_POINT('Ctrl Pts',(3.50642124159913,-1.,1.95707099606514));
#45813=CARTESIAN_POINT('Ctrl Pts',(3.50642124159913,1.,1.95707099606514));
#45814=CARTESIAN_POINT('Ctrl Pts',(3.51398354617772,-1.,1.95819025316768));
#45815=CARTESIAN_POINT('Ctrl Pts',(3.51398354617772,1.,1.95819025316768));
#45816=CARTESIAN_POINT('Ctrl Pts',(3.52155867431438,-1.,1.95926936324436));
#45817=CARTESIAN_POINT('Ctrl Pts',(3.52155867431438,1.,1.95926936324436));
#45818=CARTESIAN_POINT('Ctrl Pts',(3.52914648844289,-1.,1.96030879411534));
#45819=CARTESIAN_POINT('Ctrl Pts',(3.52914648844289,1.,1.96030879411534));
#45820=CARTESIAN_POINT('Ctrl Pts',(3.53674730625759,-1.,1.96130926212661));
#45821=CARTESIAN_POINT('Ctrl Pts',(3.53674730625759,1.,1.96130926212661));
#45822=CARTESIAN_POINT('Ctrl Pts',(3.54436163300425,-1.,1.96227157573058));
#45823=CARTESIAN_POINT('Ctrl Pts',(3.54436163300425,1.,1.96227157573058));
#45824=CARTESIAN_POINT('Ctrl Pts',(3.55198990600929,-1.,1.96319648628667));
#45825=CARTESIAN_POINT('Ctrl Pts',(3.55198990600929,1.,1.96319648628667));
#45826=CARTESIAN_POINT('Ctrl Pts',(3.55963218706201,-1.,1.96408450906868));
#45827=CARTESIAN_POINT('Ctrl Pts',(3.55963218706201,1.,1.96408450906868));
#45828=CARTESIAN_POINT('Ctrl Pts',(3.56728820357933,-1.,1.96493594634643));
#45829=CARTESIAN_POINT('Ctrl Pts',(3.56728820357933,1.,1.96493594634643));
#45830=CARTESIAN_POINT('Ctrl Pts',(3.57495748601088,-1.,1.96575096652857));
#45831=CARTESIAN_POINT('Ctrl Pts',(3.57495748601088,1.,1.96575096652857));
#45832=CARTESIAN_POINT('Ctrl Pts',(3.58263947663884,-1.,1.9665296668894));
#45833=CARTESIAN_POINT('Ctrl Pts',(3.58263947663884,1.,1.9665296668894));
#45834=CARTESIAN_POINT('Ctrl Pts',(3.5903336402273,-1.,1.96727213799507));
#45835=CARTESIAN_POINT('Ctrl Pts',(3.5903336402273,1.,1.96727213799507));
#45836=CARTESIAN_POINT('Ctrl Pts',(3.59803959819725,-1.,1.96797854118257));
#45837=CARTESIAN_POINT('Ctrl Pts',(3.59803959819725,1.,1.96797854118257));
#45838=CARTESIAN_POINT('Ctrl Pts',(3.60575714017676,-1.,1.96864911885775));
#45839=CARTESIAN_POINT('Ctrl Pts',(3.60575714017676,1.,1.96864911885775));
#45840=CARTESIAN_POINT('Ctrl Pts',(3.61348615496393,-1.,1.96928416040712));
#45841=CARTESIAN_POINT('Ctrl Pts',(3.61348615496393,1.,1.96928416040712));
#45842=CARTESIAN_POINT('Ctrl Pts',(3.62122658401722,-1.,1.96988398129888));
#45843=CARTESIAN_POINT('Ctrl Pts',(3.62122658401722,1.,1.96988398129888));
#45844=CARTESIAN_POINT('Ctrl Pts',(3.62897836973397,-1.,1.97044889850518));
#45845=CARTESIAN_POINT('Ctrl Pts',(3.62897836973397,1.,1.97044889850518));
#45846=CARTESIAN_POINT('Ctrl Pts',(3.63674139590853,-1.,1.97097920454698));
#45847=CARTESIAN_POINT('Ctrl Pts',(3.63674139590853,1.,1.97097920454698));
#45848=CARTESIAN_POINT('Ctrl Pts',(3.64451546724221,-1.,1.97147515441539));
#45849=CARTESIAN_POINT('Ctrl Pts',(3.64451546724221,1.,1.97147515441539));
#45850=CARTESIAN_POINT('Ctrl Pts',(3.65230034717364,-1.,1.97193697240645));
#45851=CARTESIAN_POINT('Ctrl Pts',(3.65230034717364,1.,1.97193697240645));
#45852=CARTESIAN_POINT('Ctrl Pts',(3.66009578166865,-1.,1.97236485439317));
#45853=CARTESIAN_POINT('Ctrl Pts',(3.66009578166865,1.,1.97236485439317));
#45854=CARTESIAN_POINT('Ctrl Pts',(3.66790152751984,-1.,1.9727589719863));
#45855=CARTESIAN_POINT('Ctrl Pts',(3.66790152751984,1.,1.9727589719863));
#45856=CARTESIAN_POINT('Ctrl Pts',(3.67571738106175,-1.,1.97311947678035));
#45857=CARTESIAN_POINT('Ctrl Pts',(3.67571738106175,1.,1.97311947678035));
#45858=CARTESIAN_POINT('Ctrl Pts',(3.68354319913416,-1.,1.97344650303631));
#45859=CARTESIAN_POINT('Ctrl Pts',(3.68354319913416,1.,1.97344650303631));
#45860=CARTESIAN_POINT('Ctrl Pts',(3.69137888597855,-1.,1.97374016224397));
#45861=CARTESIAN_POINT('Ctrl Pts',(3.69137888597855,1.,1.97374016224397));
#45862=CARTESIAN_POINT('Ctrl Pts',(3.69765528558292,-1.,1.97394846382289));
#45863=CARTESIAN_POINT('Ctrl Pts',(3.69765528558292,1.,1.97394846382289));
#45864=CARTESIAN_POINT('Ctrl Pts',(3.70236698911837,-1.,1.97408973726149));
#45865=CARTESIAN_POINT('Ctrl Pts',(3.70236698911837,1.,1.97408973726149));
#45866=CARTESIAN_POINT('Ctrl Pts',(3.7055100813194,-1.,1.974177276451));
#45867=CARTESIAN_POINT('Ctrl Pts',(3.7055100813194,1.,1.974177276451));
#45868=CARTESIAN_POINT('Ctrl Pts',(3.70708211654725,-1.,1.97421938526992));
#45869=CARTESIAN_POINT('Ctrl Pts',(3.70708211654725,1.,1.97421938526992));
#45870=CARTESIAN_POINT('',(3.24413672884902,1.,1.88097764062542));
#45871=CARTESIAN_POINT('Ctrl Pts',(3.24413672884902,-1.,1.88097764062542));
#45872=CARTESIAN_POINT('Ctrl Pts',(3.24413672884902,-0.666666666666667,
1.88097764062542));
#45873=CARTESIAN_POINT('Ctrl Pts',(3.24413672884902,-0.333333333333333,
1.88097764062542));
#45874=CARTESIAN_POINT('Ctrl Pts',(3.24413672884902,0.333333333333333,1.88097764062542));
#45875=CARTESIAN_POINT('Ctrl Pts',(3.24413672884902,0.666666666666667,1.88097764062541));
#45876=CARTESIAN_POINT('Ctrl Pts',(3.24413672884902,1.,1.88097764062541));
#45877=CARTESIAN_POINT('',(3.70708211654725,1.,1.97421938526992));
#45878=CARTESIAN_POINT('',(3.70708211654725,0.,1.97421938526992));
#45879=CARTESIAN_POINT('Ctrl Pts',(3.24413672884902,1.,1.88097764062542));
#45880=CARTESIAN_POINT('Ctrl Pts',(3.24415531671311,1.,1.88102292397987));
#45881=CARTESIAN_POINT('Ctrl Pts',(3.24428080352952,1.,1.88117508446657));
#45882=CARTESIAN_POINT('Ctrl Pts',(3.24480754675942,1.,1.88156537699118));
#45883=CARTESIAN_POINT('Ctrl Pts',(3.24625654410705,1.,1.88242596600422));
#45884=CARTESIAN_POINT('Ctrl Pts',(3.24935200512055,1.,1.88407708646435));
#45885=CARTESIAN_POINT('Ctrl Pts',(3.25408686339298,1.,1.88646802523372));
#45886=CARTESIAN_POINT('Ctrl Pts',(3.2599988519361,1.,1.88934996203508));
#45887=CARTESIAN_POINT('Ctrl Pts',(3.2667765388833,1.,1.89255393500769));
#45888=CARTESIAN_POINT('Ctrl Pts',(3.27407108932908,1.,1.89589172903662));
#45889=CARTESIAN_POINT('Ctrl Pts',(3.28154737912287,1.,1.89918429230425));
#45890=CARTESIAN_POINT('Ctrl Pts',(3.28893448600364,1.,1.9022897124757));
#45891=CARTESIAN_POINT('Ctrl Pts',(3.29608978722258,1.,1.9051389186417));
#45892=CARTESIAN_POINT('Ctrl Pts',(3.30300595568341,1.,1.90773912171424));
#45893=CARTESIAN_POINT('Ctrl Pts',(3.30975721158694,1.,1.91014297830502));
#45894=CARTESIAN_POINT('Ctrl Pts',(3.31646052426395,1.,1.91242616234459));
#45895=CARTESIAN_POINT('Ctrl Pts',(3.32323403454507,1.,1.91466343916612));
#45896=CARTESIAN_POINT('Ctrl Pts',(3.33014884257812,1.,1.91690081930297));
#45897=CARTESIAN_POINT('Ctrl Pts',(3.33721230709948,1.,1.91914609610173));
#45898=CARTESIAN_POINT('Ctrl Pts',(3.34439448941915,1.,1.92138450828378));
#45899=CARTESIAN_POINT('Ctrl Pts',(3.35164424847206,1.,1.92358838440518));
#45900=CARTESIAN_POINT('Ctrl Pts',(3.35890824422976,1.,1.92572846125763));
#45901=CARTESIAN_POINT('Ctrl Pts',(3.36615168657597,1.,1.92778626543803));
#45902=CARTESIAN_POINT('Ctrl Pts',(3.37336807068078,1.,1.92975993109897));
#45903=CARTESIAN_POINT('Ctrl Pts',(3.38056768525577,1.,1.93165739093292));
#45904=CARTESIAN_POINT('Ctrl Pts',(3.38777076883267,1.,1.93349233176794));
#45905=CARTESIAN_POINT('Ctrl Pts',(3.39499923640789,1.,1.93527929945982));
#45906=CARTESIAN_POINT('Ctrl Pts',(3.40226802104093,1.,1.93702857723089));
#45907=CARTESIAN_POINT('Ctrl Pts',(3.40957978266622,1.,1.93874306008132));
#45908=CARTESIAN_POINT('Ctrl Pts',(3.41692971994082,1.,1.94042111965237));
#45909=CARTESIAN_POINT('Ctrl Pts',(3.42430850941497,1.,1.94205835913692));
#45910=CARTESIAN_POINT('Ctrl Pts',(3.43170586602436,1.,1.94364973660285));
#45911=CARTESIAN_POINT('Ctrl Pts',(3.43911410197693,1.,1.94519168842883));
#45912=CARTESIAN_POINT('Ctrl Pts',(3.44653088665685,1.,1.94668377715332));
#45913=CARTESIAN_POINT('Ctrl Pts',(3.45395731584051,1.,1.94812754766524));
#45914=CARTESIAN_POINT('Ctrl Pts',(3.46139661060959,1.,1.94952575850196));
#45915=CARTESIAN_POINT('Ctrl Pts',(3.4688525897419,1.,1.95088147859876));
#45916=CARTESIAN_POINT('Ctrl Pts',(3.47632820495926,1.,1.95219722189878));
#45917=CARTESIAN_POINT('Ctrl Pts',(3.48382414832648,1.,1.95347412486316));
#45918=CARTESIAN_POINT('Ctrl Pts',(3.49133956289154,1.,1.95471236969653));
#45919=CARTESIAN_POINT('Ctrl Pts',(3.49887263575602,1.,1.9559115382367));
#45920=CARTESIAN_POINT('Ctrl Pts',(3.50642124159913,1.,1.95707099606514));
#45921=CARTESIAN_POINT('Ctrl Pts',(3.51398354617772,1.,1.95819025316768));
#45922=CARTESIAN_POINT('Ctrl Pts',(3.52155867431438,1.,1.95926936324436));
#45923=CARTESIAN_POINT('Ctrl Pts',(3.52914648844289,1.,1.96030879411534));
#45924=CARTESIAN_POINT('Ctrl Pts',(3.53674730625759,1.,1.96130926212661));
#45925=CARTESIAN_POINT('Ctrl Pts',(3.54436163300425,1.,1.96227157573058));
#45926=CARTESIAN_POINT('Ctrl Pts',(3.55198990600929,1.,1.96319648628667));
#45927=CARTESIAN_POINT('Ctrl Pts',(3.55963218706201,1.,1.96408450906868));
#45928=CARTESIAN_POINT('Ctrl Pts',(3.56728820357933,1.,1.96493594634643));
#45929=CARTESIAN_POINT('Ctrl Pts',(3.57495748601088,1.,1.96575096652857));
#45930=CARTESIAN_POINT('Ctrl Pts',(3.58263947663884,1.,1.9665296668894));
#45931=CARTESIAN_POINT('Ctrl Pts',(3.5903336402273,1.,1.96727213799507));
#45932=CARTESIAN_POINT('Ctrl Pts',(3.59803959819725,1.,1.96797854118257));
#45933=CARTESIAN_POINT('Ctrl Pts',(3.60575714017676,1.,1.96864911885775));
#45934=CARTESIAN_POINT('Ctrl Pts',(3.61348615496393,1.,1.96928416040712));
#45935=CARTESIAN_POINT('Ctrl Pts',(3.62122658401722,1.,1.96988398129888));
#45936=CARTESIAN_POINT('Ctrl Pts',(3.62897836973397,1.,1.97044889850518));
#45937=CARTESIAN_POINT('Ctrl Pts',(3.63674139590853,1.,1.97097920454698));
#45938=CARTESIAN_POINT('Ctrl Pts',(3.64451546724221,1.,1.97147515441539));
#45939=CARTESIAN_POINT('Ctrl Pts',(3.65230034717364,1.,1.97193697240645));
#45940=CARTESIAN_POINT('Ctrl Pts',(3.66009578166865,1.,1.97236485439317));
#45941=CARTESIAN_POINT('Ctrl Pts',(3.66790152751984,1.,1.9727589719863));
#45942=CARTESIAN_POINT('Ctrl Pts',(3.67571738106175,1.,1.97311947678035));
#45943=CARTESIAN_POINT('Ctrl Pts',(3.68354319913416,1.,1.97344650303631));
#45944=CARTESIAN_POINT('Ctrl Pts',(3.69137888597855,1.,1.97374016224397));
#45945=CARTESIAN_POINT('Ctrl Pts',(3.69765528558292,1.,1.97394846382289));
#45946=CARTESIAN_POINT('Ctrl Pts',(3.70236698911837,1.,1.97408973726149));
#45947=CARTESIAN_POINT('Ctrl Pts',(3.7055100813194,1.,1.974177276451));
#45948=CARTESIAN_POINT('Ctrl Pts',(3.70708211654725,1.,1.97421938526992));
#45949=CARTESIAN_POINT('Origin',(3.70708211654725,0.,1.97421938526992));
#45950=CARTESIAN_POINT('',(3.77614523045147,1.,1.83867539237861));
#45951=CARTESIAN_POINT('Origin',(0.,0.,0.));
#45952=CARTESIAN_POINT('',(3.14877060440425,1.,2.03660101169564));
#45953=CARTESIAN_POINT('Origin',(0.,1.,0.));
#45954=CARTESIAN_POINT('Ctrl Pts',(3.14877060440425,1.,2.03660101169564));
#45955=CARTESIAN_POINT('Ctrl Pts',(3.14877060440425,0.666666666666667,2.03660101169564));
#45956=CARTESIAN_POINT('Ctrl Pts',(3.14877060440425,0.333333333333333,2.03660101169564));
#45957=CARTESIAN_POINT('Ctrl Pts',(3.14877060440425,-0.333333333333333,
2.03660101169564));
#45958=CARTESIAN_POINT('Ctrl Pts',(3.14877060440425,-0.666666666666667,
2.03660101169564));
#45959=CARTESIAN_POINT('Ctrl Pts',(3.14877060440425,-1.,2.03660101169564));
#45960=CARTESIAN_POINT('Ctrl Pts',(3.44202241512147,-1.,2.40675750623143));
#45961=CARTESIAN_POINT('Ctrl Pts',(3.44202241512147,1.,2.40675750623143));
#45962=CARTESIAN_POINT('Ctrl Pts',(3.44127120683402,-1.,2.40537592959345));
#45963=CARTESIAN_POINT('Ctrl Pts',(3.44127120683402,1.,2.40537592959345));
#45964=CARTESIAN_POINT('Ctrl Pts',(3.43976627485223,-1.,2.40261515590099));
#45965=CARTESIAN_POINT('Ctrl Pts',(3.43976627485223,1.,2.40261515590099));
#45966=CARTESIAN_POINT('Ctrl Pts',(3.43750133066036,-1.,2.39848113411429));
#45967=CARTESIAN_POINT('Ctrl Pts',(3.43750133066036,1.,2.39848113411429));
#45968=CARTESIAN_POINT('Ctrl Pts',(3.43446630680436,-1.,2.39298338805823));
#45969=CARTESIAN_POINT('Ctrl Pts',(3.43446630680436,1.,2.39298338805823));
#45970=CARTESIAN_POINT('Ctrl Pts',(3.43064732714472,-1.,2.38613505844641));
#45971=CARTESIAN_POINT('Ctrl Pts',(3.43064732714472,1.,2.38613505844641));
#45972=CARTESIAN_POINT('Ctrl Pts',(3.42680309755241,-1.,2.37931067029517));
#45973=CARTESIAN_POINT('Ctrl Pts',(3.42680309755241,1.,2.37931067029517));
#45974=CARTESIAN_POINT('Ctrl Pts',(3.42293356216595,-1.,2.37251035954351));
#45975=CARTESIAN_POINT('Ctrl Pts',(3.42293356216595,1.,2.37251035954351));
#45976=CARTESIAN_POINT('Ctrl Pts',(3.41903866635384,-1.,2.36573431470314));
#45977=CARTESIAN_POINT('Ctrl Pts',(3.41903866635384,1.,2.36573431470314));
#45978=CARTESIAN_POINT('Ctrl Pts',(3.4151183675076,-1.,2.35898278606449));
#45979=CARTESIAN_POINT('Ctrl Pts',(3.4151183675076,1.,2.35898278606449));
#45980=CARTESIAN_POINT('Ctrl Pts',(3.41117262313464,-1.,2.35225606823649));
#45981=CARTESIAN_POINT('Ctrl Pts',(3.41117262313464,1.,2.35225606823649));
#45982=CARTESIAN_POINT('Ctrl Pts',(3.40720137403888,-1.,2.34555447648901));
#45983=CARTESIAN_POINT('Ctrl Pts',(3.40720137403888,1.,2.34555447648901));
#45984=CARTESIAN_POINT('Ctrl Pts',(3.40320452776646,-1.,2.33887832342715));
#45985=CARTESIAN_POINT('Ctrl Pts',(3.40320452776646,1.,2.33887832342715));
#45986=CARTESIAN_POINT('Ctrl Pts',(3.39918194578115,-1.,2.33222789882601));
#45987=CARTESIAN_POINT('Ctrl Pts',(3.39918194578115,1.,2.33222789882601));
#45988=CARTESIAN_POINT('Ctrl Pts',(3.39513342020045,-1.,2.32560343902683));
#45989=CARTESIAN_POINT('Ctrl Pts',(3.39513342020045,1.,2.32560343902683));
#45990=CARTESIAN_POINT('Ctrl Pts',(3.39105869475112,-1.,2.31900513925627));
#45991=CARTESIAN_POINT('Ctrl Pts',(3.39105869475112,1.,2.31900513925627));
#45992=CARTESIAN_POINT('Ctrl Pts',(3.38695751492659,-1.,2.31243319489505));
#45993=CARTESIAN_POINT('Ctrl Pts',(3.38695751492659,1.,2.31243319489505));
#45994=CARTESIAN_POINT('Ctrl Pts',(3.38282967336676,-1.,2.30588783640389));
#45995=CARTESIAN_POINT('Ctrl Pts',(3.38282967336676,1.,2.30588783640389));
#45996=CARTESIAN_POINT('Ctrl Pts',(3.37867504959382,-1.,2.29936936127588));
#45997=CARTESIAN_POINT('Ctrl Pts',(3.37867504959382,1.,2.29936936127588));
#45998=CARTESIAN_POINT('Ctrl Pts',(3.37449367172707,-1.,2.2928781800731));
#45999=CARTESIAN_POINT('Ctrl Pts',(3.37449367172707,1.,2.2928781800731));
#46000=CARTESIAN_POINT('Ctrl Pts',(3.37028570206357,-1.,2.28641481081045));
#46001=CARTESIAN_POINT('Ctrl Pts',(3.37028570206357,1.,2.28641481081045));
#46002=CARTESIAN_POINT('Ctrl Pts',(3.36605130712978,-1.,2.27997979457968));
#46003=CARTESIAN_POINT('Ctrl Pts',(3.36605130712978,1.,2.27997979457968));
#46004=CARTESIAN_POINT('Ctrl Pts',(3.36179055004369,-1.,2.27357362620902));
#46005=CARTESIAN_POINT('Ctrl Pts',(3.36179055004369,1.,2.27357362620902));
#46006=CARTESIAN_POINT('Ctrl Pts',(3.35750328523077,-1.,2.26719668579921));
#46007=CARTESIAN_POINT('Ctrl Pts',(3.35750328523077,1.,2.26719668579921));
#46008=CARTESIAN_POINT('Ctrl Pts',(3.35318902552676,-1.,2.26084915222484));
#46009=CARTESIAN_POINT('Ctrl Pts',(3.35318902552676,1.,2.26084915222484));
#46010=CARTESIAN_POINT('Ctrl Pts',(3.34884690292342,-1.,2.25453097693524));
#46011=CARTESIAN_POINT('Ctrl Pts',(3.34884690292342,1.,2.25453097693524));
#46012=CARTESIAN_POINT('Ctrl Pts',(3.34447596770768,-1.,2.24824207678288));
#46013=CARTESIAN_POINT('Ctrl Pts',(3.34447596770768,1.,2.24824207678288));
#46014=CARTESIAN_POINT('Ctrl Pts',(3.34007543738044,-1.,2.24198249391437));
#46015=CARTESIAN_POINT('Ctrl Pts',(3.34007543738044,1.,2.24198249391437));
#46016=CARTESIAN_POINT('Ctrl Pts',(3.33564495756478,-1.,2.2357525632881));
#46017=CARTESIAN_POINT('Ctrl Pts',(3.33564495756478,1.,2.2357525632881));
#46018=CARTESIAN_POINT('Ctrl Pts',(3.33118487773593,-1.,2.22955308907221));
#46019=CARTESIAN_POINT('Ctrl Pts',(3.33118487773593,1.,2.22955308907221));
#46020=CARTESIAN_POINT('Ctrl Pts',(3.32669646722871,-1.,2.22338548312759));
#46021=CARTESIAN_POINT('Ctrl Pts',(3.32669646722871,1.,2.22338548312759));
#46022=CARTESIAN_POINT('Ctrl Pts',(3.32218125618955,-1.,2.21725135110889));
#46023=CARTESIAN_POINT('Ctrl Pts',(3.32218125618955,1.,2.21725135110889));
#46024=CARTESIAN_POINT('Ctrl Pts',(3.31764044024231,-1.,2.21115211847872));
#46025=CARTESIAN_POINT('Ctrl Pts',(3.31764044024231,1.,2.21115211847872));
#46026=CARTESIAN_POINT('Ctrl Pts',(3.3130742460895,-1.,2.20508863150608));
#46027=CARTESIAN_POINT('Ctrl Pts',(3.3130742460895,1.,2.20508863150608));
#46028=CARTESIAN_POINT('Ctrl Pts',(3.30848134694596,-1.,2.19906078949925));
#46029=CARTESIAN_POINT('Ctrl Pts',(3.30848134694596,1.,2.19906078949925));
#46030=CARTESIAN_POINT('Ctrl Pts',(3.30385816281831,-1.,2.19306710376112));
#46031=CARTESIAN_POINT('Ctrl Pts',(3.30385816281831,1.,2.19306710376112));
#46032=CARTESIAN_POINT('Ctrl Pts',(3.29920022557635,-1.,2.18710556500325));
#46033=CARTESIAN_POINT('Ctrl Pts',(3.29920022557635,1.,2.18710556500325));
#46034=CARTESIAN_POINT('Ctrl Pts',(3.29450361500484,-1.,2.18117455557062));
#46035=CARTESIAN_POINT('Ctrl Pts',(3.29450361500484,1.,2.18117455557062));
#46036=CARTESIAN_POINT('Ctrl Pts',(3.28976645712566,-1.,2.17527380048422));
#46037=CARTESIAN_POINT('Ctrl Pts',(3.28976645712566,1.,2.17527380048422));
#46038=CARTESIAN_POINT('Ctrl Pts',(3.2849901997973,-1.,2.16940517773459));
#46039=CARTESIAN_POINT('Ctrl Pts',(3.2849901997973,1.,2.16940517773459));
#46040=CARTESIAN_POINT('Ctrl Pts',(3.28018150841414,-1.,2.16357391934434));
#46041=CARTESIAN_POINT('Ctrl Pts',(3.28018150841414,1.,2.16357391934434));
#46042=CARTESIAN_POINT('Ctrl Pts',(3.27534954469206,-1.,2.15778690038359));
#46043=CARTESIAN_POINT('Ctrl Pts',(3.27534954469206,1.,2.15778690038359));
#46044=CARTESIAN_POINT('Ctrl Pts',(3.27050245897244,-1.,2.15205043199818));
#46045=CARTESIAN_POINT('Ctrl Pts',(3.27050245897244,1.,2.15205043199818));
#46046=CARTESIAN_POINT('Ctrl Pts',(3.26564388189764,-1.,2.14636805295663));
#46047=CARTESIAN_POINT('Ctrl Pts',(3.26564388189764,1.,2.14636805295663));
#46048=CARTESIAN_POINT('Ctrl Pts',(3.26077002641868,-1.,2.14073870754258));
#46049=CARTESIAN_POINT('Ctrl Pts',(3.26077002641868,1.,2.14073870754258));
#46050=CARTESIAN_POINT('Ctrl Pts',(3.25586495065027,-1.,2.13515375878786));
#46051=CARTESIAN_POINT('Ctrl Pts',(3.25586495065027,1.,2.13515375878786));
#46052=CARTESIAN_POINT('Ctrl Pts',(3.25090574493994,-1.,2.1296002839681));
#46053=CARTESIAN_POINT('Ctrl Pts',(3.25090574493994,1.,2.1296002839681));
#46054=CARTESIAN_POINT('Ctrl Pts',(3.24587102613347,-1.,2.12406646410943));
#46055=CARTESIAN_POINT('Ctrl Pts',(3.24587102613347,1.,2.12406646410943));
#46056=CARTESIAN_POINT('Ctrl Pts',(3.24074905517282,-1.,2.11854673326972));
#46057=CARTESIAN_POINT('Ctrl Pts',(3.24074905517282,1.,2.11854673326972));
#46058=CARTESIAN_POINT('Ctrl Pts',(3.23554444767115,-1.,2.11304604021784));
#46059=CARTESIAN_POINT('Ctrl Pts',(3.23554444767115,1.,2.11304604021784));
#46060=CARTESIAN_POINT('Ctrl Pts',(3.23028945793334,-1.,2.1075869964248));
#46061=CARTESIAN_POINT('Ctrl Pts',(3.23028945793334,1.,2.1075869964248));
#46062=CARTESIAN_POINT('Ctrl Pts',(3.22503437553496,-1.,2.10220384298534));
#46063=CARTESIAN_POINT('Ctrl Pts',(3.22503437553496,1.,2.10220384298534));
#46064=CARTESIAN_POINT('Ctrl Pts',(3.21982707347067,-1.,2.09692958434933));
#46065=CARTESIAN_POINT('Ctrl Pts',(3.21982707347067,1.,2.09692958434933));
#46066=CARTESIAN_POINT('Ctrl Pts',(3.2146942960168,-1.,2.0917841946046));
#46067=CARTESIAN_POINT('Ctrl Pts',(3.2146942960168,1.,2.0917841946046));
#46068=CARTESIAN_POINT('Ctrl Pts',(3.20962575845433,-1.,2.08676465517435));
#46069=CARTESIAN_POINT('Ctrl Pts',(3.20962575845433,1.,2.08676465517435));
#46070=CARTESIAN_POINT('Ctrl Pts',(3.20454818630635,-1.,2.08182850370816));
#46071=CARTESIAN_POINT('Ctrl Pts',(3.20454818630635,1.,2.08182850370816));
#46072=CARTESIAN_POINT('Ctrl Pts',(3.19934132835879,-1.,2.0769044187063));
#46073=CARTESIAN_POINT('Ctrl Pts',(3.19934132835879,1.,2.0769044187063));
#46074=CARTESIAN_POINT('Ctrl Pts',(3.19388465568113,-1.,2.07192253497765));
#46075=CARTESIAN_POINT('Ctrl Pts',(3.19388465568113,1.,2.07192253497765));
#46076=CARTESIAN_POINT('Ctrl Pts',(3.18809755562297,-1.,2.06684062744065));
#46077=CARTESIAN_POINT('Ctrl Pts',(3.18809755562297,1.,2.06684062744065));
#46078=CARTESIAN_POINT('Ctrl Pts',(3.18197692964677,-1.,2.06166849827143));
#46079=CARTESIAN_POINT('Ctrl Pts',(3.18197692964677,1.,2.06166849827143));
#46080=CARTESIAN_POINT('Ctrl Pts',(3.17564906975592,-1.,2.05650186773279));
#46081=CARTESIAN_POINT('Ctrl Pts',(3.17564906975592,1.,2.05650186773279));
#46082=CARTESIAN_POINT('Ctrl Pts',(3.16936341689859,-1.,2.05151770247452));
#46083=CARTESIAN_POINT('Ctrl Pts',(3.16936341689859,1.,2.05151770247452));
#46084=CARTESIAN_POINT('Ctrl Pts',(3.16343165059235,-1.,2.0469333124766));
#46085=CARTESIAN_POINT('Ctrl Pts',(3.16343165059235,1.,2.0469333124766));
#46086=CARTESIAN_POINT('Ctrl Pts',(3.15817983946525,-1.,2.04297406404132));
#46087=CARTESIAN_POINT('Ctrl Pts',(3.15817983946525,1.,2.04297406404132));
#46088=CARTESIAN_POINT('Ctrl Pts',(3.1538999167466,-1.,2.03984073791432));
#46089=CARTESIAN_POINT('Ctrl Pts',(3.1538999167466,1.,2.03984073791432));
#46090=CARTESIAN_POINT('Ctrl Pts',(3.15079010635326,-1.,2.03766932526171));
#46091=CARTESIAN_POINT('Ctrl Pts',(3.15079010635326,1.,2.03766932526171));
#46092=CARTESIAN_POINT('Ctrl Pts',(3.14931281967585,-1.,2.03675273048882));
#46093=CARTESIAN_POINT('Ctrl Pts',(3.14931281967585,1.,2.03675273048882));
#46094=CARTESIAN_POINT('Ctrl Pts',(3.14878756590499,-1.,2.03653654935384));
#46095=CARTESIAN_POINT('Ctrl Pts',(3.14878756590499,1.,2.03653654935384));
#46096=CARTESIAN_POINT('Ctrl Pts',(3.14869618937138,-1.,2.036601737578));
#46097=CARTESIAN_POINT('Ctrl Pts',(3.14869618937138,1.,2.036601737578));
#46098=CARTESIAN_POINT('Ctrl Pts',(3.1487152044751,-1.,2.03668666247593));
#46099=CARTESIAN_POINT('Ctrl Pts',(3.1487152044751,1.,2.03668666247593));
#46100=CARTESIAN_POINT('',(3.44202241512147,1.,2.40675750623143));
#46101=CARTESIAN_POINT('Ctrl Pts',(3.44202241512147,1.,2.40675750623143));
#46102=CARTESIAN_POINT('Ctrl Pts',(3.44127120683402,1.,2.40537592959345));
#46103=CARTESIAN_POINT('Ctrl Pts',(3.43976627485223,1.,2.40261515590099));
#46104=CARTESIAN_POINT('Ctrl Pts',(3.43750133066036,1.,2.39848113411429));
#46105=CARTESIAN_POINT('Ctrl Pts',(3.43446630680436,1.,2.39298338805823));
#46106=CARTESIAN_POINT('Ctrl Pts',(3.43064732714472,1.,2.38613505844641));
#46107=CARTESIAN_POINT('Ctrl Pts',(3.42680309755241,1.,2.37931067029517));
#46108=CARTESIAN_POINT('Ctrl Pts',(3.42293356216595,1.,2.37251035954351));
#46109=CARTESIAN_POINT('Ctrl Pts',(3.41903866635384,1.,2.36573431470314));
#46110=CARTESIAN_POINT('Ctrl Pts',(3.4151183675076,1.,2.35898278606449));
#46111=CARTESIAN_POINT('Ctrl Pts',(3.41117262313464,1.,2.35225606823649));
#46112=CARTESIAN_POINT('Ctrl Pts',(3.40720137403888,1.,2.34555447648901));
#46113=CARTESIAN_POINT('Ctrl Pts',(3.40320452776646,1.,2.33887832342715));
#46114=CARTESIAN_POINT('Ctrl Pts',(3.39918194578115,1.,2.33222789882601));
#46115=CARTESIAN_POINT('Ctrl Pts',(3.39513342020045,1.,2.32560343902683));
#46116=CARTESIAN_POINT('Ctrl Pts',(3.39105869475112,1.,2.31900513925627));
#46117=CARTESIAN_POINT('Ctrl Pts',(3.38695751492659,1.,2.31243319489505));
#46118=CARTESIAN_POINT('Ctrl Pts',(3.38282967336676,1.,2.30588783640389));
#46119=CARTESIAN_POINT('Ctrl Pts',(3.37867504959382,1.,2.29936936127588));
#46120=CARTESIAN_POINT('Ctrl Pts',(3.37449367172707,1.,2.2928781800731));
#46121=CARTESIAN_POINT('Ctrl Pts',(3.37028570206357,1.,2.28641481081045));
#46122=CARTESIAN_POINT('Ctrl Pts',(3.36605130712978,1.,2.27997979457968));
#46123=CARTESIAN_POINT('Ctrl Pts',(3.36179055004369,1.,2.27357362620902));
#46124=CARTESIAN_POINT('Ctrl Pts',(3.35750328523077,1.,2.26719668579921));
#46125=CARTESIAN_POINT('Ctrl Pts',(3.35318902552676,1.,2.26084915222484));
#46126=CARTESIAN_POINT('Ctrl Pts',(3.34884690292342,1.,2.25453097693524));
#46127=CARTESIAN_POINT('Ctrl Pts',(3.34447596770768,1.,2.24824207678288));
#46128=CARTESIAN_POINT('Ctrl Pts',(3.34007543738044,1.,2.24198249391437));
#46129=CARTESIAN_POINT('Ctrl Pts',(3.33564495756478,1.,2.2357525632881));
#46130=CARTESIAN_POINT('Ctrl Pts',(3.33118487773593,1.,2.22955308907221));
#46131=CARTESIAN_POINT('Ctrl Pts',(3.32669646722871,1.,2.22338548312759));
#46132=CARTESIAN_POINT('Ctrl Pts',(3.32218125618955,1.,2.21725135110889));
#46133=CARTESIAN_POINT('Ctrl Pts',(3.31764044024231,1.,2.21115211847872));
#46134=CARTESIAN_POINT('Ctrl Pts',(3.3130742460895,1.,2.20508863150608));
#46135=CARTESIAN_POINT('Ctrl Pts',(3.30848134694596,1.,2.19906078949925));
#46136=CARTESIAN_POINT('Ctrl Pts',(3.30385816281831,1.,2.19306710376112));
#46137=CARTESIAN_POINT('Ctrl Pts',(3.29920022557635,1.,2.18710556500325));
#46138=CARTESIAN_POINT('Ctrl Pts',(3.29450361500484,1.,2.18117455557062));
#46139=CARTESIAN_POINT('Ctrl Pts',(3.28976645712566,1.,2.17527380048422));
#46140=CARTESIAN_POINT('Ctrl Pts',(3.2849901997973,1.,2.16940517773459));
#46141=CARTESIAN_POINT('Ctrl Pts',(3.28018150841414,1.,2.16357391934434));
#46142=CARTESIAN_POINT('Ctrl Pts',(3.27534954469206,1.,2.15778690038359));
#46143=CARTESIAN_POINT('Ctrl Pts',(3.27050245897244,1.,2.15205043199818));
#46144=CARTESIAN_POINT('Ctrl Pts',(3.26564388189764,1.,2.14636805295663));
#46145=CARTESIAN_POINT('Ctrl Pts',(3.26077002641868,1.,2.14073870754258));
#46146=CARTESIAN_POINT('Ctrl Pts',(3.25586495065027,1.,2.13515375878786));
#46147=CARTESIAN_POINT('Ctrl Pts',(3.25090574493994,1.,2.1296002839681));
#46148=CARTESIAN_POINT('Ctrl Pts',(3.24587102613347,1.,2.12406646410943));
#46149=CARTESIAN_POINT('Ctrl Pts',(3.24074905517282,1.,2.11854673326972));
#46150=CARTESIAN_POINT('Ctrl Pts',(3.23554444767115,1.,2.11304604021784));
#46151=CARTESIAN_POINT('Ctrl Pts',(3.23028945793334,1.,2.1075869964248));
#46152=CARTESIAN_POINT('Ctrl Pts',(3.22503437553496,1.,2.10220384298534));
#46153=CARTESIAN_POINT('Ctrl Pts',(3.21982707347067,1.,2.09692958434933));
#46154=CARTESIAN_POINT('Ctrl Pts',(3.2146942960168,1.,2.0917841946046));
#46155=CARTESIAN_POINT('Ctrl Pts',(3.20962575845433,1.,2.08676465517435));
#46156=CARTESIAN_POINT('Ctrl Pts',(3.20454818630635,1.,2.08182850370816));
#46157=CARTESIAN_POINT('Ctrl Pts',(3.19934132835879,1.,2.0769044187063));
#46158=CARTESIAN_POINT('Ctrl Pts',(3.19388465568113,1.,2.07192253497765));
#46159=CARTESIAN_POINT('Ctrl Pts',(3.18809755562297,1.,2.06684062744065));
#46160=CARTESIAN_POINT('Ctrl Pts',(3.18197692964677,1.,2.06166849827143));
#46161=CARTESIAN_POINT('Ctrl Pts',(3.17564906975592,1.,2.05650186773279));
#46162=CARTESIAN_POINT('Ctrl Pts',(3.16936341689859,1.,2.05151770247452));
#46163=CARTESIAN_POINT('Ctrl Pts',(3.16343165059235,1.,2.0469333124766));
#46164=CARTESIAN_POINT('Ctrl Pts',(3.15817983946525,1.,2.04297406404132));
#46165=CARTESIAN_POINT('Ctrl Pts',(3.1538999167466,1.,2.03984073791432));
#46166=CARTESIAN_POINT('Ctrl Pts',(3.15102344775396,1.,2.03783225496023));
#46167=CARTESIAN_POINT('Ctrl Pts',(3.14959882629936,1.,2.03693188810614));
#46168=CARTESIAN_POINT('Ctrl Pts',(3.14901193669147,1.,2.03663974554941));
#46169=CARTESIAN_POINT('Ctrl Pts',(3.1488193908823,1.,2.03659701539175));
#46170=CARTESIAN_POINT('Ctrl Pts',(3.14877060440425,1.,2.03660101169564));
#46171=CARTESIAN_POINT('',(3.44202241512147,0.,2.40675750623143));
#46172=CARTESIAN_POINT('Ctrl Pts',(2.91001063062876,-1.,2.36523532225181));
#46173=CARTESIAN_POINT('Ctrl Pts',(2.91001063062876,1.,2.36523532225181));
#46174=CARTESIAN_POINT('Ctrl Pts',(2.90992398626211,-1.,2.36524348105112));
#46175=CARTESIAN_POINT('Ctrl Pts',(2.90992398626211,1.,2.36524348105112));
#46176=CARTESIAN_POINT('Ctrl Pts',(2.90989022548032,-1.,2.36535052956938));
#46177=CARTESIAN_POINT('Ctrl Pts',(2.90989022548032,1.,2.36535052956938));
#46178=CARTESIAN_POINT('Ctrl Pts',(2.91025813830041,-1.,2.36578327194741));
#46179=CARTESIAN_POINT('Ctrl Pts',(2.91025813830041,1.,2.36578327194741));
#46180=CARTESIAN_POINT('Ctrl Pts',(2.9115863784204,-1.,2.36690501170627));
#46181=CARTESIAN_POINT('Ctrl Pts',(2.9115863784204,1.,2.36690501170627));
#46182=CARTESIAN_POINT('Ctrl Pts',(2.9146124988314,-1.,2.36919161373173));
#46183=CARTESIAN_POINT('Ctrl Pts',(2.9146124988314,1.,2.36919161373173));
#46184=CARTESIAN_POINT('Ctrl Pts',(2.91891503791411,-1.,2.37229381109821));
#46185=CARTESIAN_POINT('Ctrl Pts',(2.91891503791411,1.,2.37229381109821));
#46186=CARTESIAN_POINT('Ctrl Pts',(2.92430340582608,-1.,2.3760651052403));
#46187=CARTESIAN_POINT('Ctrl Pts',(2.92430340582608,1.,2.3760651052403));
#46188=CARTESIAN_POINT('Ctrl Pts',(2.93049643640206,-1.,2.38028989582073));
#46189=CARTESIAN_POINT('Ctrl Pts',(2.93049643640206,1.,2.38028989582073));
#46190=CARTESIAN_POINT('Ctrl Pts',(2.93717903280391,-1.,2.38472771516311));
#46191=CARTESIAN_POINT('Ctrl Pts',(2.93717903280391,1.,2.38472771516311));
#46192=CARTESIAN_POINT('Ctrl Pts',(2.94404820669076,-1.,2.38914929090759));
#46193=CARTESIAN_POINT('Ctrl Pts',(2.94404820669076,1.,2.38914929090759));
#46194=CARTESIAN_POINT('Ctrl Pts',(2.95085857128439,-1.,2.39337207631667));
#46195=CARTESIAN_POINT('Ctrl Pts',(2.95085857128439,1.,2.39337207631667));
#46196=CARTESIAN_POINT('Ctrl Pts',(2.95748006482942,-1.,2.39730553974517));
#46197=CARTESIAN_POINT('Ctrl Pts',(2.95748006482942,1.,2.39730553974517));
#46198=CARTESIAN_POINT('Ctrl Pts',(2.96390432240312,-1.,2.4009556571164));
#46199=CARTESIAN_POINT('Ctrl Pts',(2.96390432240312,1.,2.4009556571164));
#46200=CARTESIAN_POINT('Ctrl Pts',(2.9701964131236,-1.,2.40438604734919));
#46201=CARTESIAN_POINT('Ctrl Pts',(2.9701964131236,1.,2.40438604734919));
#46202=CARTESIAN_POINT('Ctrl Pts',(2.97646002822422,-1.,2.40768975073713));
#46203=CARTESIAN_POINT('Ctrl Pts',(2.97646002822422,1.,2.40768975073713));
#46204=CARTESIAN_POINT('Ctrl Pts',(2.98280015815107,-1.,2.41095909342571));
#46205=CARTESIAN_POINT('Ctrl Pts',(2.98280015815107,1.,2.41095909342571));
#46206=CARTESIAN_POINT('Ctrl Pts',(2.98927983005796,-1.,2.41425064199586));
#46207=CARTESIAN_POINT('Ctrl Pts',(2.98927983005796,1.,2.41425064199586));
#46208=CARTESIAN_POINT('Ctrl Pts',(2.99590509293503,-1.,2.41757324500514));
#46209=CARTESIAN_POINT('Ctrl Pts',(2.99590509293503,1.,2.41757324500514));
#46210=CARTESIAN_POINT('Ctrl Pts',(3.00264868585996,-1.,2.42090763946779));
#46211=CARTESIAN_POINT('Ctrl Pts',(3.00264868585996,1.,2.42090763946779));
#46212=CARTESIAN_POINT('Ctrl Pts',(3.00946442616658,-1.,2.42421849439613));
#46213=CARTESIAN_POINT('Ctrl Pts',(3.00946442616658,1.,2.42421849439613));
#46214=CARTESIAN_POINT('Ctrl Pts',(3.01630420830504,-1.,2.42746856264168));
#46215=CARTESIAN_POINT('Ctrl Pts',(3.01630420830504,1.,2.42746856264168));
#46216=CARTESIAN_POINT('Ctrl Pts',(3.02313656036004,-1.,2.43063415586637));
#46217=CARTESIAN_POINT('Ctrl Pts',(3.02313656036004,1.,2.43063415586637));
#46218=CARTESIAN_POINT('Ctrl Pts',(3.02995534946978,-1.,2.43371241361488));
#46219=CARTESIAN_POINT('Ctrl Pts',(3.02995534946978,1.,2.43371241361488));
#46220=CARTESIAN_POINT('Ctrl Pts',(3.03676949672821,-1.,2.43671278042414));
#46221=CARTESIAN_POINT('Ctrl Pts',(3.03676949672821,1.,2.43671278042414));
#46222=CARTESIAN_POINT('Ctrl Pts',(3.04359685040555,-1.,2.43965194061857));
#46223=CARTESIAN_POINT('Ctrl Pts',(3.04359685040555,1.,2.43965194061857));
#46224=CARTESIAN_POINT('Ctrl Pts',(3.05045678021504,-1.,2.44254768923105));
#46225=CARTESIAN_POINT('Ctrl Pts',(3.05045678021504,1.,2.44254768923105));
#46226=CARTESIAN_POINT('Ctrl Pts',(3.05736242671506,-1.,2.44541251892556));
#46227=CARTESIAN_POINT('Ctrl Pts',(3.05736242671506,1.,2.44541251892556));
#46228=CARTESIAN_POINT('Ctrl Pts',(3.06431596421405,-1.,2.44824970516544));
#46229=CARTESIAN_POINT('Ctrl Pts',(3.06431596421405,1.,2.44824970516544));
#46230=CARTESIAN_POINT('Ctrl Pts',(3.07131290521297,-1.,2.45105688854422));
#46231=CARTESIAN_POINT('Ctrl Pts',(3.07131290521297,1.,2.45105688854422));
#46232=CARTESIAN_POINT('Ctrl Pts',(3.07834472886139,-1.,2.4538282678779));
#46233=CARTESIAN_POINT('Ctrl Pts',(3.07834472886139,1.,2.4538282678779));
#46234=CARTESIAN_POINT('Ctrl Pts',(3.08540206545315,-1.,2.45655725437039));
#46235=CARTESIAN_POINT('Ctrl Pts',(3.08540206545315,1.,2.45655725437039));
#46236=CARTESIAN_POINT('Ctrl Pts',(3.09247787931887,-1.,2.4592391256388));
#46237=CARTESIAN_POINT('Ctrl Pts',(3.09247787931887,1.,2.4592391256388));
#46238=CARTESIAN_POINT('Ctrl Pts',(3.09956993697052,-1.,2.46187308501884));
#46239=CARTESIAN_POINT('Ctrl Pts',(3.09956993697052,1.,2.46187308501884));
#46240=CARTESIAN_POINT('Ctrl Pts',(3.1066790790198,-1.,2.46446082979646));
#46241=CARTESIAN_POINT('Ctrl Pts',(3.1066790790198,1.,2.46446082979646));
#46242=CARTESIAN_POINT('Ctrl Pts',(3.11380805536122,-1.,2.46700558843506));
#46243=CARTESIAN_POINT('Ctrl Pts',(3.11380805536122,1.,2.46700558843506));
#46244=CARTESIAN_POINT('Ctrl Pts',(3.12096015766983,-1.,2.46951098947469));
#46245=CARTESIAN_POINT('Ctrl Pts',(3.12096015766983,1.,2.46951098947469));
#46246=CARTESIAN_POINT('Ctrl Pts',(3.12813790805952,-1.,2.47197997765871));
#46247=CARTESIAN_POINT('Ctrl Pts',(3.12813790805952,1.,2.47197997765871));
#46248=CARTESIAN_POINT('Ctrl Pts',(3.13534181229295,-1.,2.47441378371932));
#46249=CARTESIAN_POINT('Ctrl Pts',(3.13534181229295,1.,2.47441378371932));
#46250=CARTESIAN_POINT('Ctrl Pts',(3.1425709954655,-1.,2.47681245356109));
#46251=CARTESIAN_POINT('Ctrl Pts',(3.1425709954655,1.,2.47681245356109));
#46252=CARTESIAN_POINT('Ctrl Pts',(3.14982373241352,-1.,2.47917529057029));
#46253=CARTESIAN_POINT('Ctrl Pts',(3.14982373241352,1.,2.47917529057029));
#46254=CARTESIAN_POINT('Ctrl Pts',(3.15709802322739,-1.,2.48150133566571));
#46255=CARTESIAN_POINT('Ctrl Pts',(3.15709802322739,1.,2.48150133566571));
#46256=CARTESIAN_POINT('Ctrl Pts',(3.16439213290161,-1.,2.48378981792725));
#46257=CARTESIAN_POINT('Ctrl Pts',(3.16439213290161,1.,2.48378981792725));
#46258=CARTESIAN_POINT('Ctrl Pts',(3.17170518863313,-1.,2.48604065348587));
#46259=CARTESIAN_POINT('Ctrl Pts',(3.17170518863313,1.,2.48604065348587));
#46260=CARTESIAN_POINT('Ctrl Pts',(3.17903698136622,-1.,2.48825428288201));
#46261=CARTESIAN_POINT('Ctrl Pts',(3.17903698136622,1.,2.48825428288201));
#46262=CARTESIAN_POINT('Ctrl Pts',(3.18638771282266,-1.,2.49043146334059));
#46263=CARTESIAN_POINT('Ctrl Pts',(3.18638771282266,1.,2.49043146334059));
#46264=CARTESIAN_POINT('Ctrl Pts',(3.19375775555798,-1.,2.49257307239848));
#46265=CARTESIAN_POINT('Ctrl Pts',(3.19375775555798,1.,2.49257307239848));
#46266=CARTESIAN_POINT('Ctrl Pts',(3.20114742397588,-1.,2.49467992057755));
#46267=CARTESIAN_POINT('Ctrl Pts',(3.20114742397588,1.,2.49467992057755));
#46268=CARTESIAN_POINT('Ctrl Pts',(3.20855669849836,-1.,2.4967525264737));
#46269=CARTESIAN_POINT('Ctrl Pts',(3.20855669849836,1.,2.4967525264737));
#46270=CARTESIAN_POINT('Ctrl Pts',(3.21598526261286,-1.,2.4987911459939));
#46271=CARTESIAN_POINT('Ctrl Pts',(3.21598526261286,1.,2.4987911459939));
#46272=CARTESIAN_POINT('Ctrl Pts',(3.22343262620503,-1.,2.50079587201958));
#46273=CARTESIAN_POINT('Ctrl Pts',(3.22343262620503,1.,2.50079587201958));
#46274=CARTESIAN_POINT('Ctrl Pts',(3.23089822320646,-1.,2.50276671338111));
#46275=CARTESIAN_POINT('Ctrl Pts',(3.23089822320646,1.,2.50276671338111));
#46276=CARTESIAN_POINT('Ctrl Pts',(3.23838151080319,-1.,2.5047036758003));
#46277=CARTESIAN_POINT('Ctrl Pts',(3.23838151080319,1.,2.5047036758003));
#46278=CARTESIAN_POINT('Ctrl Pts',(3.24588208983849,-1.,2.506606859405));
#46279=CARTESIAN_POINT('Ctrl Pts',(3.24588208983849,1.,2.506606859405));
#46280=CARTESIAN_POINT('Ctrl Pts',(3.25339971460982,-1.,2.50847647070723));
#46281=CARTESIAN_POINT('Ctrl Pts',(3.25339971460982,1.,2.50847647070723));
#46282=CARTESIAN_POINT('Ctrl Pts',(3.26093423001434,-1.,2.51031277813486));
#46283=CARTESIAN_POINT('Ctrl Pts',(3.26093423001434,1.,2.51031277813486));
#46284=CARTESIAN_POINT('Ctrl Pts',(3.26848552888115,-1.,2.51211608411423));
#46285=CARTESIAN_POINT('Ctrl Pts',(3.26848552888115,1.,2.51211608411423));
#46286=CARTESIAN_POINT('Ctrl Pts',(3.27605350473142,-1.,2.513886692704));
#46287=CARTESIAN_POINT('Ctrl Pts',(3.27605350473142,1.,2.513886692704));
#46288=CARTESIAN_POINT('Ctrl Pts',(3.28363799702982,-1.,2.51562487464514));
#46289=CARTESIAN_POINT('Ctrl Pts',(3.28363799702982,1.,2.51562487464514));
#46290=CARTESIAN_POINT('Ctrl Pts',(3.2912387729927,-1.,2.51733085123797));
#46291=CARTESIAN_POINT('Ctrl Pts',(3.2912387729927,1.,2.51733085123797));
#46292=CARTESIAN_POINT('Ctrl Pts',(3.29885556388352,-1.,2.51900480701069));
#46293=CARTESIAN_POINT('Ctrl Pts',(3.29885556388352,1.,2.51900480701069));
#46294=CARTESIAN_POINT('Ctrl Pts',(3.30648808815442,-1.,2.52064689568511));
#46295=CARTESIAN_POINT('Ctrl Pts',(3.30648808815442,1.,2.52064689568511));
#46296=CARTESIAN_POINT('Ctrl Pts',(3.31413607874645,-1.,2.52225724871313));
#46297=CARTESIAN_POINT('Ctrl Pts',(3.31413607874645,1.,2.52225724871313));
#46298=CARTESIAN_POINT('Ctrl Pts',(3.32179931078699,-1.,2.5238359839626));
#46299=CARTESIAN_POINT('Ctrl Pts',(3.32179931078699,1.,2.5238359839626));
#46300=CARTESIAN_POINT('Ctrl Pts',(3.32947762187533,-1.,2.52538321164634));
#46301=CARTESIAN_POINT('Ctrl Pts',(3.32947762187533,1.,2.52538321164634));
#46302=CARTESIAN_POINT('Ctrl Pts',(3.33717089999103,-1.,2.52689902690158));
#46303=CARTESIAN_POINT('Ctrl Pts',(3.33717089999103,1.,2.52689902690158));
#46304=CARTESIAN_POINT('Ctrl Pts',(3.34333744115511,-1.,2.52808660915689));
#46305=CARTESIAN_POINT('Ctrl Pts',(3.34333744115511,1.,2.52808660915689));
#46306=CARTESIAN_POINT('Ctrl Pts',(3.34796903576663,-1.,2.52896321610703));
#46307=CARTESIAN_POINT('Ctrl Pts',(3.34796903576663,1.,2.52896321610703));
#46308=CARTESIAN_POINT('Ctrl Pts',(3.35105973714071,-1.,2.5295413654909));
#46309=CARTESIAN_POINT('Ctrl Pts',(3.35105973714071,1.,2.5295413654909));
#46310=CARTESIAN_POINT('Ctrl Pts',(3.35260583073571,-1.,2.52982887637028));
#46311=CARTESIAN_POINT('Ctrl Pts',(3.35260583073571,1.,2.52982887637028));
#46312=CARTESIAN_POINT('',(2.90994629141676,1.,2.36531447826073));
#46313=CARTESIAN_POINT('Ctrl Pts',(2.90994629141676,-1.,2.36531447826073));
#46314=CARTESIAN_POINT('Ctrl Pts',(2.90994629141676,-0.666666666666667,
2.36531447826073));
#46315=CARTESIAN_POINT('Ctrl Pts',(2.90994629141676,-0.333333333333333,
2.36531447826073));
#46316=CARTESIAN_POINT('Ctrl Pts',(2.90994629141676,0.333333333333333,2.36531447826073));
#46317=CARTESIAN_POINT('Ctrl Pts',(2.90994629141676,0.666666666666667,2.36531447826073));
#46318=CARTESIAN_POINT('Ctrl Pts',(2.90994629141676,1.,2.36531447826073));
#46319=CARTESIAN_POINT('',(3.35260583073571,1.,2.52982887637028));
#46320=CARTESIAN_POINT('',(3.35260583073571,0.,2.52982887637028));
#46321=CARTESIAN_POINT('Ctrl Pts',(2.90994629141676,1.,2.36531447826073));
#46322=CARTESIAN_POINT('Ctrl Pts',(2.90995756655606,1.,2.36536211188453));
#46323=CARTESIAN_POINT('Ctrl Pts',(2.91005770527719,1.,2.36553202948613));
#46324=CARTESIAN_POINT('Ctrl Pts',(2.91051690822156,1.,2.36599991765749));
#46325=CARTESIAN_POINT('Ctrl Pts',(2.91181344022548,1.,2.36707658451664));
#46326=CARTESIAN_POINT('Ctrl Pts',(2.9146124988314,1.,2.36919161373173));
#46327=CARTESIAN_POINT('Ctrl Pts',(2.91891503791411,1.,2.37229381109821));
#46328=CARTESIAN_POINT('Ctrl Pts',(2.92430340582608,1.,2.3760651052403));
#46329=CARTESIAN_POINT('Ctrl Pts',(2.93049643640206,1.,2.38028989582073));
#46330=CARTESIAN_POINT('Ctrl Pts',(2.93717903280391,1.,2.38472771516311));
#46331=CARTESIAN_POINT('Ctrl Pts',(2.94404820669076,1.,2.38914929090759));
#46332=CARTESIAN_POINT('Ctrl Pts',(2.95085857128439,1.,2.39337207631667));
#46333=CARTESIAN_POINT('Ctrl Pts',(2.95748006482942,1.,2.39730553974517));
#46334=CARTESIAN_POINT('Ctrl Pts',(2.96390432240312,1.,2.4009556571164));
#46335=CARTESIAN_POINT('Ctrl Pts',(2.9701964131236,1.,2.40438604734919));
#46336=CARTESIAN_POINT('Ctrl Pts',(2.97646002822422,1.,2.40768975073713));
#46337=CARTESIAN_POINT('Ctrl Pts',(2.98280015815107,1.,2.41095909342571));
#46338=CARTESIAN_POINT('Ctrl Pts',(2.98927983005796,1.,2.41425064199586));
#46339=CARTESIAN_POINT('Ctrl Pts',(2.99590509293503,1.,2.41757324500514));
#46340=CARTESIAN_POINT('Ctrl Pts',(3.00264868585996,1.,2.42090763946779));
#46341=CARTESIAN_POINT('Ctrl Pts',(3.00946442616658,1.,2.42421849439613));
#46342=CARTESIAN_POINT('Ctrl Pts',(3.01630420830504,1.,2.42746856264168));
#46343=CARTESIAN_POINT('Ctrl Pts',(3.02313656036004,1.,2.43063415586637));
#46344=CARTESIAN_POINT('Ctrl Pts',(3.02995534946978,1.,2.43371241361488));
#46345=CARTESIAN_POINT('Ctrl Pts',(3.03676949672821,1.,2.43671278042414));
#46346=CARTESIAN_POINT('Ctrl Pts',(3.04359685040555,1.,2.43965194061857));
#46347=CARTESIAN_POINT('Ctrl Pts',(3.05045678021504,1.,2.44254768923105));
#46348=CARTESIAN_POINT('Ctrl Pts',(3.05736242671506,1.,2.44541251892556));
#46349=CARTESIAN_POINT('Ctrl Pts',(3.06431596421405,1.,2.44824970516544));
#46350=CARTESIAN_POINT('Ctrl Pts',(3.07131290521297,1.,2.45105688854422));
#46351=CARTESIAN_POINT('Ctrl Pts',(3.07834472886139,1.,2.4538282678779));
#46352=CARTESIAN_POINT('Ctrl Pts',(3.08540206545315,1.,2.45655725437039));
#46353=CARTESIAN_POINT('Ctrl Pts',(3.09247787931887,1.,2.4592391256388));
#46354=CARTESIAN_POINT('Ctrl Pts',(3.09956993697052,1.,2.46187308501884));
#46355=CARTESIAN_POINT('Ctrl Pts',(3.1066790790198,1.,2.46446082979646));
#46356=CARTESIAN_POINT('Ctrl Pts',(3.11380805536122,1.,2.46700558843506));
#46357=CARTESIAN_POINT('Ctrl Pts',(3.12096015766983,1.,2.46951098947469));
#46358=CARTESIAN_POINT('Ctrl Pts',(3.12813790805952,1.,2.47197997765871));
#46359=CARTESIAN_POINT('Ctrl Pts',(3.13534181229295,1.,2.47441378371932));
#46360=CARTESIAN_POINT('Ctrl Pts',(3.1425709954655,1.,2.47681245356109));
#46361=CARTESIAN_POINT('Ctrl Pts',(3.14982373241352,1.,2.47917529057029));
#46362=CARTESIAN_POINT('Ctrl Pts',(3.15709802322739,1.,2.48150133566571));
#46363=CARTESIAN_POINT('Ctrl Pts',(3.16439213290161,1.,2.48378981792725));
#46364=CARTESIAN_POINT('Ctrl Pts',(3.17170518863313,1.,2.48604065348587));
#46365=CARTESIAN_POINT('Ctrl Pts',(3.17903698136622,1.,2.48825428288201));
#46366=CARTESIAN_POINT('Ctrl Pts',(3.18638771282266,1.,2.49043146334059));
#46367=CARTESIAN_POINT('Ctrl Pts',(3.19375775555798,1.,2.49257307239848));
#46368=CARTESIAN_POINT('Ctrl Pts',(3.20114742397588,1.,2.49467992057755));
#46369=CARTESIAN_POINT('Ctrl Pts',(3.20855669849836,1.,2.4967525264737));
#46370=CARTESIAN_POINT('Ctrl Pts',(3.21598526261286,1.,2.4987911459939));
#46371=CARTESIAN_POINT('Ctrl Pts',(3.22343262620503,1.,2.50079587201958));
#46372=CARTESIAN_POINT('Ctrl Pts',(3.23089822320646,1.,2.50276671338111));
#46373=CARTESIAN_POINT('Ctrl Pts',(3.23838151080319,1.,2.5047036758003));
#46374=CARTESIAN_POINT('Ctrl Pts',(3.24588208983849,1.,2.506606859405));
#46375=CARTESIAN_POINT('Ctrl Pts',(3.25339971460982,1.,2.50847647070723));
#46376=CARTESIAN_POINT('Ctrl Pts',(3.26093423001434,1.,2.51031277813486));
#46377=CARTESIAN_POINT('Ctrl Pts',(3.26848552888115,1.,2.51211608411423));
#46378=CARTESIAN_POINT('Ctrl Pts',(3.27605350473142,1.,2.513886692704));
#46379=CARTESIAN_POINT('Ctrl Pts',(3.28363799702982,1.,2.51562487464514));
#46380=CARTESIAN_POINT('Ctrl Pts',(3.2912387729927,1.,2.51733085123797));
#46381=CARTESIAN_POINT('Ctrl Pts',(3.29885556388352,1.,2.51900480701069));
#46382=CARTESIAN_POINT('Ctrl Pts',(3.30648808815442,1.,2.52064689568511));
#46383=CARTESIAN_POINT('Ctrl Pts',(3.31413607874645,1.,2.52225724871313));
#46384=CARTESIAN_POINT('Ctrl Pts',(3.32179931078699,1.,2.5238359839626));
#46385=CARTESIAN_POINT('Ctrl Pts',(3.32947762187533,1.,2.52538321164634));
#46386=CARTESIAN_POINT('Ctrl Pts',(3.33717089999103,1.,2.52689902690158));
#46387=CARTESIAN_POINT('Ctrl Pts',(3.34333744115511,1.,2.52808660915689));
#46388=CARTESIAN_POINT('Ctrl Pts',(3.34796903576663,1.,2.52896321610703));
#46389=CARTESIAN_POINT('Ctrl Pts',(3.35105973714071,1.,2.5295413654909));
#46390=CARTESIAN_POINT('Ctrl Pts',(3.35260583073571,1.,2.52982887637028));
#46391=CARTESIAN_POINT('Origin',(3.35260583073571,0.,2.52982887637028));
#46392=CARTESIAN_POINT('',(3.44202241512147,1.,2.40675750623143));
#46393=CARTESIAN_POINT('Origin',(0.,0.,0.));
#46394=CARTESIAN_POINT('',(2.79140942341378,1.,2.50410331873042));
#46395=CARTESIAN_POINT('Origin',(0.,1.,0.));
#46396=CARTESIAN_POINT('Ctrl Pts',(2.79140942341378,1.,2.50410331873043));
#46397=CARTESIAN_POINT('Ctrl Pts',(2.79140942341378,0.666666666666667,2.50410331873043));
#46398=CARTESIAN_POINT('Ctrl Pts',(2.79140942341378,0.333333333333333,2.50410331873042));
#46399=CARTESIAN_POINT('Ctrl Pts',(2.79140942341378,-0.333333333333333,
2.50410331873042));
#46400=CARTESIAN_POINT('Ctrl Pts',(2.79140942341378,-0.666666666666667,
2.50410331873042));
#46401=CARTESIAN_POINT('Ctrl Pts',(2.79140942341378,-1.,2.50410331873042));
#46402=CARTESIAN_POINT('Ctrl Pts',(3.02314558451372,-1.,2.91557726271063));
#46403=CARTESIAN_POINT('Ctrl Pts',(3.02314558451372,1.,2.91557726271063));
#46404=CARTESIAN_POINT('Ctrl Pts',(3.02261975104912,-1.,2.91409518070707));
#46405=CARTESIAN_POINT('Ctrl Pts',(3.02261975104912,1.,2.91409518070707));
#46406=CARTESIAN_POINT('Ctrl Pts',(3.02156522743299,-1.,2.91113297349052));
#46407=CARTESIAN_POINT('Ctrl Pts',(3.02156522743299,1.,2.91113297349052));
#46408=CARTESIAN_POINT('Ctrl Pts',(3.01997487194926,-1.,2.90669553303902));
#46409=CARTESIAN_POINT('Ctrl Pts',(3.01997487194926,1.,2.90669553303902));
#46410=CARTESIAN_POINT('Ctrl Pts',(3.01783725123646,-1.,2.90079069102661));
#46411=CARTESIAN_POINT('Ctrl Pts',(3.01783725123646,1.,2.90079069102661));
#46412=CARTESIAN_POINT('Ctrl Pts',(3.01513660433291,-1.,2.8934292556764));
#46413=CARTESIAN_POINT('Ctrl Pts',(3.01513660433291,1.,2.8934292556764));
#46414=CARTESIAN_POINT('Ctrl Pts',(3.01240727309568,-1.,2.88608751706796));
#46415=CARTESIAN_POINT('Ctrl Pts',(3.01240727309568,1.,2.88608751706796));
#46416=CARTESIAN_POINT('Ctrl Pts',(3.0096491810855,-1.,2.87876560072799));
#46417=CARTESIAN_POINT('Ctrl Pts',(3.0096491810855,1.,2.87876560072799));
#46418=CARTESIAN_POINT('Ctrl Pts',(3.00686224485374,-1.,2.87146368430104));
#46419=CARTESIAN_POINT('Ctrl Pts',(3.00686224485374,1.,2.87146368430104));
#46420=CARTESIAN_POINT('Ctrl Pts',(3.00404638316245,-1.,2.86418200833065));
#46421=CARTESIAN_POINT('Ctrl Pts',(3.00404638316245,1.,2.86418200833065));
#46422=CARTESIAN_POINT('Ctrl Pts',(3.0012015079552,-1.,2.85692085715129));
#46423=CARTESIAN_POINT('Ctrl Pts',(3.0012015079552,1.,2.85692085715129));
#46424=CARTESIAN_POINT('Ctrl Pts',(2.99832751144566,-1.,2.84968053289104));
#46425=CARTESIAN_POINT('Ctrl Pts',(2.99832751144566,1.,2.84968053289104));
#46426=CARTESIAN_POINT('Ctrl Pts',(2.995424253416,-1.,2.84246132984334));
#46427=CARTESIAN_POINT('Ctrl Pts',(2.995424253416,1.,2.84246132984334));
#46428=CARTESIAN_POINT('Ctrl Pts',(2.99249155170479,-1.,2.83526351254383));
#46429=CARTESIAN_POINT('Ctrl Pts',(2.99249155170479,1.,2.83526351254383));
#46430=CARTESIAN_POINT('Ctrl Pts',(2.98952916401699,-1.,2.82808728190402));
#46431=CARTESIAN_POINT('Ctrl Pts',(2.98952916401699,1.,2.82808728190402));
#46432=CARTESIAN_POINT('Ctrl Pts',(2.98653680669434,-1.,2.82093279065704));
#46433=CARTESIAN_POINT('Ctrl Pts',(2.98653680669434,1.,2.82093279065704));
#46434=CARTESIAN_POINT('Ctrl Pts',(2.9835141977994,-1.,2.81380019196454));
#46435=CARTESIAN_POINT('Ctrl Pts',(2.9835141977994,1.,2.81380019196454));
#46436=CARTESIAN_POINT('Ctrl Pts',(2.98046109647299,-1.,2.80668968101162));
#46437=CARTESIAN_POINT('Ctrl Pts',(2.98046109647299,1.,2.80668968101162));
#46438=CARTESIAN_POINT('Ctrl Pts',(2.97737733718242,-1.,2.79960153278186));
#46439=CARTESIAN_POINT('Ctrl Pts',(2.97737733718242,1.,2.79960153278186));
#46440=CARTESIAN_POINT('Ctrl Pts',(2.97426288347475,-1.,2.79253615718147));
#46441=CARTESIAN_POINT('Ctrl Pts',(2.97426288347475,1.,2.79253615718147));
#46442=CARTESIAN_POINT('Ctrl Pts',(2.97111781461349,-1.,2.78549409123657));
#46443=CARTESIAN_POINT('Ctrl Pts',(2.97111781461349,1.,2.78549409123657));
#46444=CARTESIAN_POINT('Ctrl Pts',(2.9679422104295,-1.,2.77847589542767));
#46445=CARTESIAN_POINT('Ctrl Pts',(2.9679422104295,1.,2.77847589542767));
#46446=CARTESIAN_POINT('Ctrl Pts',(2.96473605585548,-1.,2.77148206836464));
#46447=CARTESIAN_POINT('Ctrl Pts',(2.96473605585548,1.,2.77148206836464));
#46448=CARTESIAN_POINT('Ctrl Pts',(2.96149914764832,-1.,2.76451296269571));
#46449=CARTESIAN_POINT('Ctrl Pts',(2.96149914764832,1.,2.76451296269571));
#46450=CARTESIAN_POINT('Ctrl Pts',(2.9582309766594,-1.,2.75756867888393));
#46451=CARTESIAN_POINT('Ctrl Pts',(2.9582309766594,1.,2.75756867888393));
#46452=CARTESIAN_POINT('Ctrl Pts',(2.95493069316211,-1.,2.75064903318996));
#46453=CARTESIAN_POINT('Ctrl Pts',(2.95493069316211,1.,2.75064903318996));
#46454=CARTESIAN_POINT('Ctrl Pts',(2.95159737214304,-1.,2.7437537949221));
#46455=CARTESIAN_POINT('Ctrl Pts',(2.95159737214304,1.,2.7437537949221));
#46456=CARTESIAN_POINT('Ctrl Pts',(2.94823023414381,-1.,2.73688288329825));
#46457=CARTESIAN_POINT('Ctrl Pts',(2.94823023414381,1.,2.73688288329825));
#46458=CARTESIAN_POINT('Ctrl Pts',(2.94482887675139,-1.,2.73003657371613));
#46459=CARTESIAN_POINT('Ctrl Pts',(2.94482887675139,1.,2.73003657371613));
#46460=CARTESIAN_POINT('Ctrl Pts',(2.94139351933882,-1.,2.72321571511322));
#46461=CARTESIAN_POINT('Ctrl Pts',(2.94139351933882,1.,2.72321571511322));
#46462=CARTESIAN_POINT('Ctrl Pts',(2.93792519474955,-1.,2.71642190053575));
#46463=CARTESIAN_POINT('Ctrl Pts',(2.93792519474955,1.,2.71642190053575));
#46464=CARTESIAN_POINT('Ctrl Pts',(2.93442516311167,-1.,2.70965695523776));
#46465=CARTESIAN_POINT('Ctrl Pts',(2.93442516311167,1.,2.70965695523776));
#46466=CARTESIAN_POINT('Ctrl Pts',(2.93089438233746,-1.,2.70292247416881));
#46467=CARTESIAN_POINT('Ctrl Pts',(2.93089438233746,1.,2.70292247416881));
#46468=CARTESIAN_POINT('Ctrl Pts',(2.92733294395268,-1.,2.69621932864302));
#46469=CARTESIAN_POINT('Ctrl Pts',(2.92733294395268,1.,2.69621932864302));
#46470=CARTESIAN_POINT('Ctrl Pts',(2.92373955325876,-1.,2.68954721165342));
#46471=CARTESIAN_POINT('Ctrl Pts',(2.92373955325876,1.,2.68954721165342));
#46472=CARTESIAN_POINT('Ctrl Pts',(2.92011090722152,-1.,2.68290409279689));
#46473=CARTESIAN_POINT('Ctrl Pts',(2.92011090722152,1.,2.68290409279689));
#46474=CARTESIAN_POINT('Ctrl Pts',(2.91644290704281,-1.,2.67628728855309));
#46475=CARTESIAN_POINT('Ctrl Pts',(2.91644290704281,1.,2.67628728855309));
#46476=CARTESIAN_POINT('Ctrl Pts',(2.91273193382876,-1.,2.66969458792627));
#46477=CARTESIAN_POINT('Ctrl Pts',(2.91273193382876,1.,2.66969458792627));
#46478=CARTESIAN_POINT('Ctrl Pts',(2.90897617968921,-1.,2.66312542616809));
#46479=CARTESIAN_POINT('Ctrl Pts',(2.90897617968921,1.,2.66312542616809));
#46480=CARTESIAN_POINT('Ctrl Pts',(2.90517678087467,-1.,2.65658188464287));
#46481=CARTESIAN_POINT('Ctrl Pts',(2.90517678087467,1.,2.65658188464287));
#46482=CARTESIAN_POINT('Ctrl Pts',(2.90133950224879,-1.,2.65007017365576));
#46483=CARTESIAN_POINT('Ctrl Pts',(2.90133950224879,1.,2.65007017365576));
#46484=CARTESIAN_POINT('Ctrl Pts',(2.89747231723361,-1.,2.64359851684146));
#46485=CARTESIAN_POINT('Ctrl Pts',(2.89747231723361,1.,2.64359851684146));
#46486=CARTESIAN_POINT('Ctrl Pts',(2.89358228854557,-1.,2.63717442263944));
#46487=CARTESIAN_POINT('Ctrl Pts',(2.89358228854557,1.,2.63717442263944));
#46488=CARTESIAN_POINT('Ctrl Pts',(2.88967244854243,-1.,2.63080195420771));
#46489=CARTESIAN_POINT('Ctrl Pts',(2.88967244854243,1.,2.63080195420771));
#46490=CARTESIAN_POINT('Ctrl Pts',(2.88573922195049,-1.,2.62447947640253));
#46491=CARTESIAN_POINT('Ctrl Pts',(2.88573922195049,1.,2.62447947640253));
#46492=CARTESIAN_POINT('Ctrl Pts',(2.88176821427502,-1.,2.61819596473087));
#46493=CARTESIAN_POINT('Ctrl Pts',(2.88176821427502,1.,2.61819596473087));
#46494=CARTESIAN_POINT('Ctrl Pts',(2.87773881947885,-1.,2.61193507170928));
#46495=CARTESIAN_POINT('Ctrl Pts',(2.87773881947885,1.,2.61193507170928));
#46496=CARTESIAN_POINT('Ctrl Pts',(2.87363176656475,-1.,2.6056817788128));
#46497=CARTESIAN_POINT('Ctrl Pts',(2.87363176656475,1.,2.6056817788128));
#46498=CARTESIAN_POINT('Ctrl Pts',(2.86943633170712,-1.,2.59942875223202));
#46499=CARTESIAN_POINT('Ctrl Pts',(2.86943633170712,1.,2.59942875223202));
#46500=CARTESIAN_POINT('Ctrl Pts',(2.86515629953528,-1.,2.59318160184921));
#46501=CARTESIAN_POINT('Ctrl Pts',(2.86515629953528,1.,2.59318160184921));
#46502=CARTESIAN_POINT('Ctrl Pts',(2.86081999003668,-1.,2.5869677064356));
#46503=CARTESIAN_POINT('Ctrl Pts',(2.86081999003668,1.,2.5869677064356));
#46504=CARTESIAN_POINT('Ctrl Pts',(2.85647171715147,-1.,2.58082875254407));
#46505=CARTESIAN_POINT('Ctrl Pts',(2.85647171715147,1.,2.58082875254407));
#46506=CARTESIAN_POINT('Ctrl Pts',(2.85215360144482,-1.,2.57480482727128));
#46507=CARTESIAN_POINT('Ctrl Pts',(2.85215360144482,1.,2.57480482727128));
#46508=CARTESIAN_POINT('Ctrl Pts',(2.84788893329091,-1.,2.56891984251743));
#46509=CARTESIAN_POINT('Ctrl Pts',(2.84788893329091,1.,2.56891984251743));
#46510=CARTESIAN_POINT('Ctrl Pts',(2.84366802680211,-1.,2.56316920798489));
#46511=CARTESIAN_POINT('Ctrl Pts',(2.84366802680211,1.,2.56316920798489));
#46512=CARTESIAN_POINT('Ctrl Pts',(2.83942515220699,-1.,2.55749952145165));
#46513=CARTESIAN_POINT('Ctrl Pts',(2.83942515220699,1.,2.55749952145165));
#46514=CARTESIAN_POINT('Ctrl Pts',(2.83505269592412,-1.,2.55182152806964));
#46515=CARTESIAN_POINT('Ctrl Pts',(2.83505269592412,1.,2.55182152806964));
#46516=CARTESIAN_POINT('Ctrl Pts',(2.83044254225794,-1.,2.54604736792542));
#46517=CARTESIAN_POINT('Ctrl Pts',(2.83044254225794,1.,2.54604736792542));
#46518=CARTESIAN_POINT('Ctrl Pts',(2.82552167649157,-1.,2.54012272520141));
#46519=CARTESIAN_POINT('Ctrl Pts',(2.82552167649157,1.,2.54012272520141));
#46520=CARTESIAN_POINT('Ctrl Pts',(2.82028550483744,-1.,2.53405679667463));
#46521=CARTESIAN_POINT('Ctrl Pts',(2.82028550483744,1.,2.53405679667463));
#46522=CARTESIAN_POINT('Ctrl Pts',(2.8148437904867,-1.,2.52796388055457));
#46523=CARTESIAN_POINT('Ctrl Pts',(2.8148437904867,1.,2.52796388055457));
#46524=CARTESIAN_POINT('Ctrl Pts',(2.80941521967234,-1.,2.52205778589922));
#46525=CARTESIAN_POINT('Ctrl Pts',(2.80941521967234,1.,2.52205778589922));
#46526=CARTESIAN_POINT('Ctrl Pts',(2.80427363984939,-1.,2.51660190466067));
#46527=CARTESIAN_POINT('Ctrl Pts',(2.80427363984939,1.,2.51660190466067));
#46528=CARTESIAN_POINT('Ctrl Pts',(2.79970585014308,-1.,2.51186983687947));
#46529=CARTESIAN_POINT('Ctrl Pts',(2.79970585014308,1.,2.51186983687947));
#46530=CARTESIAN_POINT('Ctrl Pts',(2.7959687805717,-1.,2.50810555977564));
#46531=CARTESIAN_POINT('Ctrl Pts',(2.7959687805717,1.,2.50810555977564));
#46532=CARTESIAN_POINT('Ctrl Pts',(2.79323694088143,-1.,2.50547439929077));
#46533=CARTESIAN_POINT('Ctrl Pts',(2.79323694088143,1.,2.50547439929077));
#46534=CARTESIAN_POINT('Ctrl Pts',(2.79192122906739,-1.,2.50433799076945));
#46535=CARTESIAN_POINT('Ctrl Pts',(2.79192122906739,1.,2.50433799076945));
#46536=CARTESIAN_POINT('Ctrl Pts',(2.79143626022225,-1.,2.50404230339032));
#46537=CARTESIAN_POINT('Ctrl Pts',(2.79143626022225,1.,2.50404230339032));
#46538=CARTESIAN_POINT('Ctrl Pts',(2.79133581100044,-1.,2.50409239460011));
#46539=CARTESIAN_POINT('Ctrl Pts',(2.79133581100044,1.,2.50409239460011));
#46540=CARTESIAN_POINT('Ctrl Pts',(2.79134130681569,-1.,2.50417924854921));
#46541=CARTESIAN_POINT('Ctrl Pts',(2.79134130681569,1.,2.50417924854921));
#46542=CARTESIAN_POINT('',(3.02314558451372,1.,2.91557726271063));
#46543=CARTESIAN_POINT('Ctrl Pts',(3.02314558451372,1.,2.91557726271063));
#46544=CARTESIAN_POINT('Ctrl Pts',(3.02261975104912,1.,2.91409518070707));
#46545=CARTESIAN_POINT('Ctrl Pts',(3.02156522743299,1.,2.91113297349052));
#46546=CARTESIAN_POINT('Ctrl Pts',(3.01997487194926,1.,2.90669553303902));
#46547=CARTESIAN_POINT('Ctrl Pts',(3.01783725123646,1.,2.90079069102661));
#46548=CARTESIAN_POINT('Ctrl Pts',(3.01513660433291,1.,2.8934292556764));
#46549=CARTESIAN_POINT('Ctrl Pts',(3.01240727309568,1.,2.88608751706796));
#46550=CARTESIAN_POINT('Ctrl Pts',(3.0096491810855,1.,2.87876560072799));
#46551=CARTESIAN_POINT('Ctrl Pts',(3.00686224485374,1.,2.87146368430104));
#46552=CARTESIAN_POINT('Ctrl Pts',(3.00404638316245,1.,2.86418200833065));
#46553=CARTESIAN_POINT('Ctrl Pts',(3.0012015079552,1.,2.85692085715129));
#46554=CARTESIAN_POINT('Ctrl Pts',(2.99832751144566,1.,2.84968053289104));
#46555=CARTESIAN_POINT('Ctrl Pts',(2.995424253416,1.,2.84246132984334));
#46556=CARTESIAN_POINT('Ctrl Pts',(2.99249155170479,1.,2.83526351254383));
#46557=CARTESIAN_POINT('Ctrl Pts',(2.98952916401699,1.,2.82808728190402));
#46558=CARTESIAN_POINT('Ctrl Pts',(2.98653680669434,1.,2.82093279065704));
#46559=CARTESIAN_POINT('Ctrl Pts',(2.9835141977994,1.,2.81380019196454));
#46560=CARTESIAN_POINT('Ctrl Pts',(2.98046109647299,1.,2.80668968101162));
#46561=CARTESIAN_POINT('Ctrl Pts',(2.97737733718242,1.,2.79960153278186));
#46562=CARTESIAN_POINT('Ctrl Pts',(2.97426288347475,1.,2.79253615718147));
#46563=CARTESIAN_POINT('Ctrl Pts',(2.97111781461349,1.,2.78549409123657));
#46564=CARTESIAN_POINT('Ctrl Pts',(2.9679422104295,1.,2.77847589542767));
#46565=CARTESIAN_POINT('Ctrl Pts',(2.96473605585548,1.,2.77148206836464));
#46566=CARTESIAN_POINT('Ctrl Pts',(2.96149914764832,1.,2.76451296269571));
#46567=CARTESIAN_POINT('Ctrl Pts',(2.9582309766594,1.,2.75756867888393));
#46568=CARTESIAN_POINT('Ctrl Pts',(2.95493069316211,1.,2.75064903318996));
#46569=CARTESIAN_POINT('Ctrl Pts',(2.95159737214304,1.,2.7437537949221));
#46570=CARTESIAN_POINT('Ctrl Pts',(2.94823023414381,1.,2.73688288329825));
#46571=CARTESIAN_POINT('Ctrl Pts',(2.94482887675139,1.,2.73003657371613));
#46572=CARTESIAN_POINT('Ctrl Pts',(2.94139351933882,1.,2.72321571511322));
#46573=CARTESIAN_POINT('Ctrl Pts',(2.93792519474955,1.,2.71642190053575));
#46574=CARTESIAN_POINT('Ctrl Pts',(2.93442516311167,1.,2.70965695523776));
#46575=CARTESIAN_POINT('Ctrl Pts',(2.93089438233746,1.,2.70292247416881));
#46576=CARTESIAN_POINT('Ctrl Pts',(2.92733294395268,1.,2.69621932864302));
#46577=CARTESIAN_POINT('Ctrl Pts',(2.92373955325876,1.,2.68954721165342));
#46578=CARTESIAN_POINT('Ctrl Pts',(2.92011090722152,1.,2.68290409279689));
#46579=CARTESIAN_POINT('Ctrl Pts',(2.91644290704281,1.,2.67628728855309));
#46580=CARTESIAN_POINT('Ctrl Pts',(2.91273193382876,1.,2.66969458792627));
#46581=CARTESIAN_POINT('Ctrl Pts',(2.90897617968921,1.,2.66312542616809));
#46582=CARTESIAN_POINT('Ctrl Pts',(2.90517678087467,1.,2.65658188464287));
#46583=CARTESIAN_POINT('Ctrl Pts',(2.90133950224879,1.,2.65007017365576));
#46584=CARTESIAN_POINT('Ctrl Pts',(2.89747231723361,1.,2.64359851684146));
#46585=CARTESIAN_POINT('Ctrl Pts',(2.89358228854557,1.,2.63717442263944));
#46586=CARTESIAN_POINT('Ctrl Pts',(2.88967244854243,1.,2.63080195420771));
#46587=CARTESIAN_POINT('Ctrl Pts',(2.88573922195049,1.,2.62447947640253));
#46588=CARTESIAN_POINT('Ctrl Pts',(2.88176821427502,1.,2.61819596473087));
#46589=CARTESIAN_POINT('Ctrl Pts',(2.87773881947885,1.,2.61193507170928));
#46590=CARTESIAN_POINT('Ctrl Pts',(2.87363176656475,1.,2.6056817788128));
#46591=CARTESIAN_POINT('Ctrl Pts',(2.86943633170712,1.,2.59942875223202));
#46592=CARTESIAN_POINT('Ctrl Pts',(2.86515629953528,1.,2.59318160184921));
#46593=CARTESIAN_POINT('Ctrl Pts',(2.86081999003668,1.,2.5869677064356));
#46594=CARTESIAN_POINT('Ctrl Pts',(2.85647171715147,1.,2.58082875254407));
#46595=CARTESIAN_POINT('Ctrl Pts',(2.85215360144482,1.,2.57480482727128));
#46596=CARTESIAN_POINT('Ctrl Pts',(2.84788893329091,1.,2.56891984251743));
#46597=CARTESIAN_POINT('Ctrl Pts',(2.84366802680211,1.,2.56316920798489));
#46598=CARTESIAN_POINT('Ctrl Pts',(2.83942515220699,1.,2.55749952145165));
#46599=CARTESIAN_POINT('Ctrl Pts',(2.83505269592412,1.,2.55182152806964));
#46600=CARTESIAN_POINT('Ctrl Pts',(2.83044254225794,1.,2.54604736792542));
#46601=CARTESIAN_POINT('Ctrl Pts',(2.82552167649157,1.,2.54012272520141));
#46602=CARTESIAN_POINT('Ctrl Pts',(2.82028550483744,1.,2.53405679667463));
#46603=CARTESIAN_POINT('Ctrl Pts',(2.8148437904867,1.,2.52796388055457));
#46604=CARTESIAN_POINT('Ctrl Pts',(2.80941521967234,1.,2.52205778589922));
#46605=CARTESIAN_POINT('Ctrl Pts',(2.80427363984939,1.,2.51660190466067));
#46606=CARTESIAN_POINT('Ctrl Pts',(2.79970585014308,1.,2.51186983687947));
#46607=CARTESIAN_POINT('Ctrl Pts',(2.7959687805717,1.,2.50810555977564));
#46608=CARTESIAN_POINT('Ctrl Pts',(2.79344192164204,1.,2.50567182569153));
#46609=CARTESIAN_POINT('Ctrl Pts',(2.79217568804874,1.,2.50455968395235));
#46610=CARTESIAN_POINT('Ctrl Pts',(2.79164172519039,1.,2.50417932839344));
#46611=CARTESIAN_POINT('Ctrl Pts',(2.79145823440899,1.,2.50410700351426));
#46612=CARTESIAN_POINT('Ctrl Pts',(2.79140942341378,1.,2.50410331873042));
#46613=CARTESIAN_POINT('',(3.02314558451372,0.,2.91557726271063));
#46614=CARTESIAN_POINT('Ctrl Pts',(2.5041792485492,-1.,2.79134130681569));
#46615=CARTESIAN_POINT('Ctrl Pts',(2.5041792485492,1.,2.79134130681569));
#46616=CARTESIAN_POINT('Ctrl Pts',(2.50409239460108,-1.,2.7913358110015));
#46617=CARTESIAN_POINT('Ctrl Pts',(2.50409239460108,1.,2.7913358110015));
#46618=CARTESIAN_POINT('Ctrl Pts',(2.50404230339286,-1.,2.79143626022503));
#46619=CARTESIAN_POINT('Ctrl Pts',(2.50404230339286,1.,2.79143626022503));
#46620=CARTESIAN_POINT('Ctrl Pts',(2.5043379907732,-1.,2.79192122907148));
#46621=CARTESIAN_POINT('Ctrl Pts',(2.5043379907732,1.,2.79192122907148));
#46622=CARTESIAN_POINT('Ctrl Pts',(2.50547439929414,-1.,2.7932369408851));
#46623=CARTESIAN_POINT('Ctrl Pts',(2.50547439929414,1.,2.7932369408851));
#46624=CARTESIAN_POINT('Ctrl Pts',(2.5081055597767,-1.,2.79596878057287));
#46625=CARTESIAN_POINT('Ctrl Pts',(2.5081055597767,1.,2.79596878057287));
#46626=CARTESIAN_POINT('Ctrl Pts',(2.51186983687818,-1.,2.79970585014168));
#46627=CARTESIAN_POINT('Ctrl Pts',(2.51186983687818,1.,2.79970585014168));
#46628=CARTESIAN_POINT('Ctrl Pts',(2.51660190465805,-1.,2.80427363984653));
#46629=CARTESIAN_POINT('Ctrl Pts',(2.51660190465805,1.,2.80427363984653));
#46630=CARTESIAN_POINT('Ctrl Pts',(2.52205778589653,-1.,2.80941521966941));
#46631=CARTESIAN_POINT('Ctrl Pts',(2.52205778589653,1.,2.80941521966941));
#46632=CARTESIAN_POINT('Ctrl Pts',(2.52796388055278,-1.,2.81484379048475));
#46633=CARTESIAN_POINT('Ctrl Pts',(2.52796388055278,1.,2.81484379048475));
#46634=CARTESIAN_POINT('Ctrl Pts',(2.53405679667412,-1.,2.82028550483689));
#46635=CARTESIAN_POINT('Ctrl Pts',(2.53405679667412,1.,2.82028550483689));
#46636=CARTESIAN_POINT('Ctrl Pts',(2.54012272520199,-1.,2.8255216764922));
#46637=CARTESIAN_POINT('Ctrl Pts',(2.54012272520199,1.,2.8255216764922));
#46638=CARTESIAN_POINT('Ctrl Pts',(2.54604736792655,-1.,2.83044254225917));
#46639=CARTESIAN_POINT('Ctrl Pts',(2.54604736792655,1.,2.83044254225917));
#46640=CARTESIAN_POINT('Ctrl Pts',(2.55182152807077,-1.,2.83505269592536));
#46641=CARTESIAN_POINT('Ctrl Pts',(2.55182152807077,1.,2.83505269592536));
#46642=CARTESIAN_POINT('Ctrl Pts',(2.55749952145241,-1.,2.83942515220782));
#46643=CARTESIAN_POINT('Ctrl Pts',(2.55749952145241,1.,2.83942515220782));
#46644=CARTESIAN_POINT('Ctrl Pts',(2.56316920798513,-1.,2.84366802680237));
#46645=CARTESIAN_POINT('Ctrl Pts',(2.56316920798513,1.,2.84366802680237));
#46646=CARTESIAN_POINT('Ctrl Pts',(2.56891984251721,-1.,2.84788893329067));
#46647=CARTESIAN_POINT('Ctrl Pts',(2.56891984251721,1.,2.84788893329067));
#46648=CARTESIAN_POINT('Ctrl Pts',(2.57480482727081,-1.,2.85215360144431));
#46649=CARTESIAN_POINT('Ctrl Pts',(2.57480482727081,1.,2.85215360144431));
#46650=CARTESIAN_POINT('Ctrl Pts',(2.58082875254357,-1.,2.85647171715092));
#46651=CARTESIAN_POINT('Ctrl Pts',(2.58082875254357,1.,2.85647171715092));
#46652=CARTESIAN_POINT('Ctrl Pts',(2.58696770643524,-1.,2.86081999003629));
#46653=CARTESIAN_POINT('Ctrl Pts',(2.58696770643524,1.,2.86081999003629));
#46654=CARTESIAN_POINT('Ctrl Pts',(2.59318160184908,-1.,2.86515629953513));
#46655=CARTESIAN_POINT('Ctrl Pts',(2.59318160184908,1.,2.86515629953513));
#46656=CARTESIAN_POINT('Ctrl Pts',(2.5994287522321,-1.,2.86943633170722));
#46657=CARTESIAN_POINT('Ctrl Pts',(2.5994287522321,1.,2.86943633170722));
#46658=CARTESIAN_POINT('Ctrl Pts',(2.60568177881303,-1.,2.87363176656501));
#46659=CARTESIAN_POINT('Ctrl Pts',(2.60568177881303,1.,2.87363176656501));
#46660=CARTESIAN_POINT('Ctrl Pts',(2.61193507170955,-1.,2.87773881947916));
#46661=CARTESIAN_POINT('Ctrl Pts',(2.61193507170955,1.,2.87773881947916));
#46662=CARTESIAN_POINT('Ctrl Pts',(2.61819596473108,-1.,2.88176821427525));
#46663=CARTESIAN_POINT('Ctrl Pts',(2.61819596473108,1.,2.88176821427525));
#46664=CARTESIAN_POINT('Ctrl Pts',(2.62447947640262,-1.,2.88573922195059));
#46665=CARTESIAN_POINT('Ctrl Pts',(2.62447947640262,1.,2.88573922195059));
#46666=CARTESIAN_POINT('Ctrl Pts',(2.63080195420767,-1.,2.88967244854239));
#46667=CARTESIAN_POINT('Ctrl Pts',(2.63080195420767,1.,2.88967244854239));
#46668=CARTESIAN_POINT('Ctrl Pts',(2.63717442263932,-1.,2.89358228854544));
#46669=CARTESIAN_POINT('Ctrl Pts',(2.63717442263932,1.,2.89358228854544));
#46670=CARTESIAN_POINT('Ctrl Pts',(2.64359851684131,-1.,2.89747231723345));
#46671=CARTESIAN_POINT('Ctrl Pts',(2.64359851684131,1.,2.89747231723345));
#46672=CARTESIAN_POINT('Ctrl Pts',(2.65007017365564,-1.,2.90133950224867));
#46673=CARTESIAN_POINT('Ctrl Pts',(2.65007017365564,1.,2.90133950224867));
#46674=CARTESIAN_POINT('Ctrl Pts',(2.65658188464282,-1.,2.90517678087461));
#46675=CARTESIAN_POINT('Ctrl Pts',(2.65658188464282,1.,2.90517678087461));
#46676=CARTESIAN_POINT('Ctrl Pts',(2.6631254261681,-1.,2.90897617968923));
#46677=CARTESIAN_POINT('Ctrl Pts',(2.6631254261681,1.,2.90897617968923));
#46678=CARTESIAN_POINT('Ctrl Pts',(2.66969458792631,-1.,2.91273193382882));
#46679=CARTESIAN_POINT('Ctrl Pts',(2.66969458792631,1.,2.91273193382882));
#46680=CARTESIAN_POINT('Ctrl Pts',(2.67628728855312,-1.,2.91644290704285));
#46681=CARTESIAN_POINT('Ctrl Pts',(2.67628728855312,1.,2.91644290704285));
#46682=CARTESIAN_POINT('Ctrl Pts',(2.68290409279688,-1.,2.92011090722152));
#46683=CARTESIAN_POINT('Ctrl Pts',(2.68290409279688,1.,2.92011090722152));
#46684=CARTESIAN_POINT('Ctrl Pts',(2.68954721165339,-1.,2.92373955325875));
#46685=CARTESIAN_POINT('Ctrl Pts',(2.68954721165339,1.,2.92373955325875));
#46686=CARTESIAN_POINT('Ctrl Pts',(2.69621932864301,-1.,2.92733294395267));
#46687=CARTESIAN_POINT('Ctrl Pts',(2.69621932864301,1.,2.92733294395267));
#46688=CARTESIAN_POINT('Ctrl Pts',(2.70292247416885,-1.,2.9308943823375));
#46689=CARTESIAN_POINT('Ctrl Pts',(2.70292247416885,1.,2.9308943823375));
#46690=CARTESIAN_POINT('Ctrl Pts',(2.70965695523787,-1.,2.93442516311179));
#46691=CARTESIAN_POINT('Ctrl Pts',(2.70965695523787,1.,2.93442516311179));
#46692=CARTESIAN_POINT('Ctrl Pts',(2.71642190053592,-1.,2.93792519474972));
#46693=CARTESIAN_POINT('Ctrl Pts',(2.71642190053592,1.,2.93792519474972));
#46694=CARTESIAN_POINT('Ctrl Pts',(2.72321571511337,-1.,2.94139351933897));
#46695=CARTESIAN_POINT('Ctrl Pts',(2.72321571511337,1.,2.94139351933897));
#46696=CARTESIAN_POINT('Ctrl Pts',(2.73003657371616,-1.,2.94482887675143));
#46697=CARTESIAN_POINT('Ctrl Pts',(2.73003657371616,1.,2.94482887675143));
#46698=CARTESIAN_POINT('Ctrl Pts',(2.73688288329808,-1.,2.94823023414364));
#46699=CARTESIAN_POINT('Ctrl Pts',(2.73688288329808,1.,2.94823023414364));
#46700=CARTESIAN_POINT('Ctrl Pts',(2.74375379492172,-1.,2.95159737214266));
#46701=CARTESIAN_POINT('Ctrl Pts',(2.74375379492172,1.,2.95159737214266));
#46702=CARTESIAN_POINT('Ctrl Pts',(2.75064903318947,-1.,2.95493069316161));
#46703=CARTESIAN_POINT('Ctrl Pts',(2.75064903318947,1.,2.95493069316161));
#46704=CARTESIAN_POINT('Ctrl Pts',(2.7575686788835,-1.,2.95823097665896));
#46705=CARTESIAN_POINT('Ctrl Pts',(2.7575686788835,1.,2.95823097665896));
#46706=CARTESIAN_POINT('Ctrl Pts',(2.76451296269557,-1.,2.96149914764818));
#46707=CARTESIAN_POINT('Ctrl Pts',(2.76451296269557,1.,2.96149914764818));
#46708=CARTESIAN_POINT('Ctrl Pts',(2.77148206836498,-1.,2.96473605585583));
#46709=CARTESIAN_POINT('Ctrl Pts',(2.77148206836498,1.,2.96473605585583));
#46710=CARTESIAN_POINT('Ctrl Pts',(2.7784758954285,-1.,2.96794221043036));
#46711=CARTESIAN_POINT('Ctrl Pts',(2.7784758954285,1.,2.96794221043036));
#46712=CARTESIAN_POINT('Ctrl Pts',(2.78549409123769,-1.,2.97111781461465));
#46713=CARTESIAN_POINT('Ctrl Pts',(2.78549409123769,1.,2.97111781461465));
#46714=CARTESIAN_POINT('Ctrl Pts',(2.79253615718248,-1.,2.9742628834758));
#46715=CARTESIAN_POINT('Ctrl Pts',(2.79253615718248,1.,2.9742628834758));
#46716=CARTESIAN_POINT('Ctrl Pts',(2.7996015327823,-1.,2.97737733718287));
#46717=CARTESIAN_POINT('Ctrl Pts',(2.7996015327823,1.,2.97737733718287));
#46718=CARTESIAN_POINT('Ctrl Pts',(2.80668968101106,-1.,2.98046109647241));
#46719=CARTESIAN_POINT('Ctrl Pts',(2.80668968101106,1.,2.98046109647241));
#46720=CARTESIAN_POINT('Ctrl Pts',(2.81380019196286,-1.,2.98351419779767));
#46721=CARTESIAN_POINT('Ctrl Pts',(2.81380019196286,1.,2.98351419779767));
#46722=CARTESIAN_POINT('Ctrl Pts',(2.82093279065457,-1.,2.9865368066918));
#46723=CARTESIAN_POINT('Ctrl Pts',(2.82093279065457,1.,2.9865368066918));
#46724=CARTESIAN_POINT('Ctrl Pts',(2.82808728190157,-1.,2.98952916401446));
#46725=CARTESIAN_POINT('Ctrl Pts',(2.82808728190157,1.,2.98952916401446));
#46726=CARTESIAN_POINT('Ctrl Pts',(2.83526351254248,-1.,2.9924915517034));
#46727=CARTESIAN_POINT('Ctrl Pts',(2.83526351254248,1.,2.9924915517034));
#46728=CARTESIAN_POINT('Ctrl Pts',(2.84246132984415,-1.,2.99542425341685));
#46729=CARTESIAN_POINT('Ctrl Pts',(2.84246132984415,1.,2.99542425341685));
#46730=CARTESIAN_POINT('Ctrl Pts',(2.84968053289451,-1.,2.99832751144925));
#46731=CARTESIAN_POINT('Ctrl Pts',(2.84968053289451,1.,2.99832751144925));
#46732=CARTESIAN_POINT('Ctrl Pts',(2.85692085715685,-1.,3.00120150796095));
#46733=CARTESIAN_POINT('Ctrl Pts',(2.85692085715685,1.,3.00120150796095));
#46734=CARTESIAN_POINT('Ctrl Pts',(2.86418200833667,-1.,3.00404638316867));
#46735=CARTESIAN_POINT('Ctrl Pts',(2.86418200833667,1.,3.00404638316867));
#46736=CARTESIAN_POINT('Ctrl Pts',(2.87146368430501,-1.,3.00686224485784));
#46737=CARTESIAN_POINT('Ctrl Pts',(2.87146368430501,1.,3.00686224485784));
#46738=CARTESIAN_POINT('Ctrl Pts',(2.87876560072727,-1.,3.00964918108476));
#46739=CARTESIAN_POINT('Ctrl Pts',(2.87876560072727,1.,3.00964918108476));
#46740=CARTESIAN_POINT('Ctrl Pts',(2.8860875170608,-1.,3.01240727308829));
#46741=CARTESIAN_POINT('Ctrl Pts',(2.8860875170608,1.,3.01240727308829));
#46742=CARTESIAN_POINT('Ctrl Pts',(2.89342925566321,-1.,3.01513660431928));
#46743=CARTESIAN_POINT('Ctrl Pts',(2.89342925566321,1.,3.01513660431928));
#46744=CARTESIAN_POINT('Ctrl Pts',(2.9007906910105,-1.,3.01783725121981));
#46745=CARTESIAN_POINT('Ctrl Pts',(2.9007906910105,1.,3.01783725121981));
#46746=CARTESIAN_POINT('Ctrl Pts',(2.90669553302526,-1.,3.01997487193503));
#46747=CARTESIAN_POINT('Ctrl Pts',(2.90669553302526,1.,3.01997487193503));
#46748=CARTESIAN_POINT('Ctrl Pts',(2.91113297348212,-1.,3.02156522742431));
#46749=CARTESIAN_POINT('Ctrl Pts',(2.91113297348212,1.,3.02156522742431));
#46750=CARTESIAN_POINT('Ctrl Pts',(2.91409518070399,-1.,3.02261975104593));
#46751=CARTESIAN_POINT('Ctrl Pts',(2.91409518070399,1.,3.02261975104593));
#46752=CARTESIAN_POINT('Ctrl Pts',(2.91557726271063,-1.,3.02314558451372));
#46753=CARTESIAN_POINT('Ctrl Pts',(2.91557726271063,1.,3.02314558451372));
#46754=CARTESIAN_POINT('',(2.50410331873176,1.,2.79140942341258));
#46755=CARTESIAN_POINT('Ctrl Pts',(2.50410331873176,-1.,2.79140942341258));
#46756=CARTESIAN_POINT('Ctrl Pts',(2.50410331873176,-0.666666666666667,
2.79140942341258));
#46757=CARTESIAN_POINT('Ctrl Pts',(2.50410331873176,-0.333333333333333,
2.79140942341258));
#46758=CARTESIAN_POINT('Ctrl Pts',(2.50410331873176,0.333333333333333,2.79140942341258));
#46759=CARTESIAN_POINT('Ctrl Pts',(2.50410331873176,0.666666666666667,2.79140942341258));
#46760=CARTESIAN_POINT('Ctrl Pts',(2.50410331873176,1.,2.79140942341258));
#46761=CARTESIAN_POINT('',(2.91557726271063,1.,3.02314558451372));
#46762=CARTESIAN_POINT('',(2.91557726271063,0.,3.02314558451372));
#46763=CARTESIAN_POINT('Ctrl Pts',(2.50410331873176,1.,2.79140942341258));
#46764=CARTESIAN_POINT('Ctrl Pts',(2.50410700351493,1.,2.79145823440781));
#46765=CARTESIAN_POINT('Ctrl Pts',(2.50417932839313,1.,2.79164172518905));
#46766=CARTESIAN_POINT('Ctrl Pts',(2.50455968395146,1.,2.79217568804755));
#46767=CARTESIAN_POINT('Ctrl Pts',(2.50567182569081,1.,2.79344192164147));
#46768=CARTESIAN_POINT('Ctrl Pts',(2.5081055597767,1.,2.79596878057287));
#46769=CARTESIAN_POINT('Ctrl Pts',(2.51186983687818,1.,2.79970585014168));
#46770=CARTESIAN_POINT('Ctrl Pts',(2.51660190465805,1.,2.80427363984653));
#46771=CARTESIAN_POINT('Ctrl Pts',(2.52205778589653,1.,2.80941521966941));
#46772=CARTESIAN_POINT('Ctrl Pts',(2.52796388055278,1.,2.81484379048475));
#46773=CARTESIAN_POINT('Ctrl Pts',(2.53405679667412,1.,2.82028550483689));
#46774=CARTESIAN_POINT('Ctrl Pts',(2.54012272520199,1.,2.8255216764922));
#46775=CARTESIAN_POINT('Ctrl Pts',(2.54604736792655,1.,2.83044254225917));
#46776=CARTESIAN_POINT('Ctrl Pts',(2.55182152807077,1.,2.83505269592536));
#46777=CARTESIAN_POINT('Ctrl Pts',(2.55749952145241,1.,2.83942515220782));
#46778=CARTESIAN_POINT('Ctrl Pts',(2.56316920798513,1.,2.84366802680237));
#46779=CARTESIAN_POINT('Ctrl Pts',(2.56891984251721,1.,2.84788893329067));
#46780=CARTESIAN_POINT('Ctrl Pts',(2.57480482727081,1.,2.85215360144431));
#46781=CARTESIAN_POINT('Ctrl Pts',(2.58082875254357,1.,2.85647171715092));
#46782=CARTESIAN_POINT('Ctrl Pts',(2.58696770643524,1.,2.86081999003629));
#46783=CARTESIAN_POINT('Ctrl Pts',(2.59318160184908,1.,2.86515629953513));
#46784=CARTESIAN_POINT('Ctrl Pts',(2.5994287522321,1.,2.86943633170722));
#46785=CARTESIAN_POINT('Ctrl Pts',(2.60568177881303,1.,2.87363176656501));
#46786=CARTESIAN_POINT('Ctrl Pts',(2.61193507170955,1.,2.87773881947916));
#46787=CARTESIAN_POINT('Ctrl Pts',(2.61819596473108,1.,2.88176821427525));
#46788=CARTESIAN_POINT('Ctrl Pts',(2.62447947640262,1.,2.88573922195059));
#46789=CARTESIAN_POINT('Ctrl Pts',(2.63080195420767,1.,2.88967244854239));
#46790=CARTESIAN_POINT('Ctrl Pts',(2.63717442263932,1.,2.89358228854544));
#46791=CARTESIAN_POINT('Ctrl Pts',(2.64359851684131,1.,2.89747231723345));
#46792=CARTESIAN_POINT('Ctrl Pts',(2.65007017365564,1.,2.90133950224867));
#46793=CARTESIAN_POINT('Ctrl Pts',(2.65658188464282,1.,2.90517678087461));
#46794=CARTESIAN_POINT('Ctrl Pts',(2.6631254261681,1.,2.90897617968923));
#46795=CARTESIAN_POINT('Ctrl Pts',(2.66969458792631,1.,2.91273193382882));
#46796=CARTESIAN_POINT('Ctrl Pts',(2.67628728855312,1.,2.91644290704285));
#46797=CARTESIAN_POINT('Ctrl Pts',(2.68290409279688,1.,2.92011090722152));
#46798=CARTESIAN_POINT('Ctrl Pts',(2.68954721165339,1.,2.92373955325875));
#46799=CARTESIAN_POINT('Ctrl Pts',(2.69621932864301,1.,2.92733294395267));
#46800=CARTESIAN_POINT('Ctrl Pts',(2.70292247416885,1.,2.9308943823375));
#46801=CARTESIAN_POINT('Ctrl Pts',(2.70965695523787,1.,2.93442516311179));
#46802=CARTESIAN_POINT('Ctrl Pts',(2.71642190053592,1.,2.93792519474972));
#46803=CARTESIAN_POINT('Ctrl Pts',(2.72321571511337,1.,2.94139351933897));
#46804=CARTESIAN_POINT('Ctrl Pts',(2.73003657371616,1.,2.94482887675143));
#46805=CARTESIAN_POINT('Ctrl Pts',(2.73688288329808,1.,2.94823023414364));
#46806=CARTESIAN_POINT('Ctrl Pts',(2.74375379492172,1.,2.95159737214266));
#46807=CARTESIAN_POINT('Ctrl Pts',(2.75064903318947,1.,2.95493069316161));
#46808=CARTESIAN_POINT('Ctrl Pts',(2.7575686788835,1.,2.95823097665896));
#46809=CARTESIAN_POINT('Ctrl Pts',(2.76451296269557,1.,2.96149914764818));
#46810=CARTESIAN_POINT('Ctrl Pts',(2.77148206836498,1.,2.96473605585583));
#46811=CARTESIAN_POINT('Ctrl Pts',(2.7784758954285,1.,2.96794221043036));
#46812=CARTESIAN_POINT('Ctrl Pts',(2.78549409123769,1.,2.97111781461465));
#46813=CARTESIAN_POINT('Ctrl Pts',(2.79253615718248,1.,2.9742628834758));
#46814=CARTESIAN_POINT('Ctrl Pts',(2.7996015327823,1.,2.97737733718287));
#46815=CARTESIAN_POINT('Ctrl Pts',(2.80668968101106,1.,2.98046109647241));
#46816=CARTESIAN_POINT('Ctrl Pts',(2.81380019196286,1.,2.98351419779767));
#46817=CARTESIAN_POINT('Ctrl Pts',(2.82093279065457,1.,2.9865368066918));
#46818=CARTESIAN_POINT('Ctrl Pts',(2.82808728190157,1.,2.98952916401446));
#46819=CARTESIAN_POINT('Ctrl Pts',(2.83526351254248,1.,2.9924915517034));
#46820=CARTESIAN_POINT('Ctrl Pts',(2.84246132984415,1.,2.99542425341685));
#46821=CARTESIAN_POINT('Ctrl Pts',(2.84968053289451,1.,2.99832751144925));
#46822=CARTESIAN_POINT('Ctrl Pts',(2.85692085715685,1.,3.00120150796095));
#46823=CARTESIAN_POINT('Ctrl Pts',(2.86418200833667,1.,3.00404638316867));
#46824=CARTESIAN_POINT('Ctrl Pts',(2.87146368430501,1.,3.00686224485784));
#46825=CARTESIAN_POINT('Ctrl Pts',(2.87876560072727,1.,3.00964918108476));
#46826=CARTESIAN_POINT('Ctrl Pts',(2.8860875170608,1.,3.01240727308829));
#46827=CARTESIAN_POINT('Ctrl Pts',(2.89342925566321,1.,3.01513660431928));
#46828=CARTESIAN_POINT('Ctrl Pts',(2.9007906910105,1.,3.01783725121981));
#46829=CARTESIAN_POINT('Ctrl Pts',(2.90669553302526,1.,3.01997487193503));
#46830=CARTESIAN_POINT('Ctrl Pts',(2.91113297348212,1.,3.02156522742431));
#46831=CARTESIAN_POINT('Ctrl Pts',(2.91409518070399,1.,3.02261975104593));
#46832=CARTESIAN_POINT('Ctrl Pts',(2.91557726271063,1.,3.02314558451372));
#46833=CARTESIAN_POINT('Origin',(2.91557726271063,0.,3.02314558451372));
#46834=CARTESIAN_POINT('',(3.02314558451372,1.,2.91557726271063));
#46835=CARTESIAN_POINT('Origin',(0.,0.,0.));
#46836=CARTESIAN_POINT('',(2.36531447826213,1.,2.90994629141562));
#46837=CARTESIAN_POINT('Origin',(0.,1.,0.));
#46838=CARTESIAN_POINT('Ctrl Pts',(2.36531447826213,1.,2.90994629141563));
#46839=CARTESIAN_POINT('Ctrl Pts',(2.36531447826213,0.666666666666667,2.90994629141563));
#46840=CARTESIAN_POINT('Ctrl Pts',(2.36531447826213,0.333333333333333,2.90994629141563));
#46841=CARTESIAN_POINT('Ctrl Pts',(2.36531447826213,-0.333333333333333,
2.90994629141563));
#46842=CARTESIAN_POINT('Ctrl Pts',(2.36531447826213,-0.666666666666667,
2.90994629141563));
#46843=CARTESIAN_POINT('Ctrl Pts',(2.36531447826213,-1.,2.90994629141563));
#46844=CARTESIAN_POINT('Ctrl Pts',(2.52982887637028,-1.,3.35260583073571));
#46845=CARTESIAN_POINT('Ctrl Pts',(2.52982887637028,1.,3.35260583073571));
#46846=CARTESIAN_POINT('Ctrl Pts',(2.52954136549357,-1.,3.35105973714426));
#46847=CARTESIAN_POINT('Ctrl Pts',(2.52954136549357,1.,3.35105973714426));
#46848=CARTESIAN_POINT('Ctrl Pts',(2.5289632161143,-1.,3.34796903577628));
#46849=CARTESIAN_POINT('Ctrl Pts',(2.5289632161143,1.,3.34796903577628));
#46850=CARTESIAN_POINT('Ctrl Pts',(2.52808660916879,-1.,3.34333744117093));
#46851=CARTESIAN_POINT('Ctrl Pts',(2.52808660916879,1.,3.34333744117093));
#46852=CARTESIAN_POINT('Ctrl Pts',(2.52689902691551,-1.,3.33717090000955));
#46853=CARTESIAN_POINT('Ctrl Pts',(2.52689902691551,1.,3.33717090000955));
#46854=CARTESIAN_POINT('Ctrl Pts',(2.52538321165774,-1.,3.32947762189049));
#46855=CARTESIAN_POINT('Ctrl Pts',(2.52538321165774,1.,3.32947762189049));
#46856=CARTESIAN_POINT('Ctrl Pts',(2.52383598396878,-1.,3.32179931079521));
#46857=CARTESIAN_POINT('Ctrl Pts',(2.52383598396878,1.,3.32179931079521));
#46858=CARTESIAN_POINT('Ctrl Pts',(2.52225724871375,-1.,3.31413607874727));
#46859=CARTESIAN_POINT('Ctrl Pts',(2.52225724871375,1.,3.31413607874727));
#46860=CARTESIAN_POINT('Ctrl Pts',(2.52064689568167,-1.,3.30648808814986));
#46861=CARTESIAN_POINT('Ctrl Pts',(2.52064689568167,1.,3.30648808814986));
#46862=CARTESIAN_POINT('Ctrl Pts',(2.51900480700548,-1.,3.29885556387661));
#46863=CARTESIAN_POINT('Ctrl Pts',(2.51900480700548,1.,3.29885556387661));
#46864=CARTESIAN_POINT('Ctrl Pts',(2.51733085123316,-1.,3.2912387729863));
#46865=CARTESIAN_POINT('Ctrl Pts',(2.51733085123316,1.,3.2912387729863));
#46866=CARTESIAN_POINT('Ctrl Pts',(2.51562487464214,-1.,3.28363799702583));
#46867=CARTESIAN_POINT('Ctrl Pts',(2.51562487464214,1.,3.28363799702583));
#46868=CARTESIAN_POINT('Ctrl Pts',(2.51388669270329,-1.,3.27605350473048));
#46869=CARTESIAN_POINT('Ctrl Pts',(2.51388669270329,1.,3.27605350473048));
#46870=CARTESIAN_POINT('Ctrl Pts',(2.51211608411539,-1.,3.26848552888271));
#46871=CARTESIAN_POINT('Ctrl Pts',(2.51211608411539,1.,3.26848552888271));
#46872=CARTESIAN_POINT('Ctrl Pts',(2.51031277813697,-1.,3.26093423001716));
#46873=CARTESIAN_POINT('Ctrl Pts',(2.51031277813697,1.,3.26093423001716));
#46874=CARTESIAN_POINT('Ctrl Pts',(2.50847647070936,-1.,3.25339971461265));
#46875=CARTESIAN_POINT('Ctrl Pts',(2.50847647070936,1.,3.25339971461265));
#46876=CARTESIAN_POINT('Ctrl Pts',(2.50660685940645,-1.,3.24588208984042));
#46877=CARTESIAN_POINT('Ctrl Pts',(2.50660685940645,1.,3.24588208984042));
#46878=CARTESIAN_POINT('Ctrl Pts',(2.50470367580078,-1.,3.23838151080383));
#46879=CARTESIAN_POINT('Ctrl Pts',(2.50470367580078,1.,3.23838151080383));
#46880=CARTESIAN_POINT('Ctrl Pts',(2.50276671338074,-1.,3.23089822320596));
#46881=CARTESIAN_POINT('Ctrl Pts',(2.50276671338074,1.,3.23089822320596));
#46882=CARTESIAN_POINT('Ctrl Pts',(2.5007958720187,-1.,3.22343262620387));
#46883=CARTESIAN_POINT('Ctrl Pts',(2.5007958720187,1.,3.22343262620387));
#46884=CARTESIAN_POINT('Ctrl Pts',(2.49879114599293,-1.,3.21598526261157));
#46885=CARTESIAN_POINT('Ctrl Pts',(2.49879114599293,1.,3.21598526261157));
#46886=CARTESIAN_POINT('Ctrl Pts',(2.49675252647298,-1.,3.2085566984974));
#46887=CARTESIAN_POINT('Ctrl Pts',(2.49675252647298,1.,3.2085566984974));
#46888=CARTESIAN_POINT('Ctrl Pts',(2.49467992057726,-1.,3.20114742397549));
#46889=CARTESIAN_POINT('Ctrl Pts',(2.49467992057726,1.,3.20114742397549));
#46890=CARTESIAN_POINT('Ctrl Pts',(2.4925730723986,-1.,3.19375775555814));
#46891=CARTESIAN_POINT('Ctrl Pts',(2.4925730723986,1.,3.19375775555814));
#46892=CARTESIAN_POINT('Ctrl Pts',(2.49043146334095,-1.,3.18638771282315));
#46893=CARTESIAN_POINT('Ctrl Pts',(2.49043146334095,1.,3.18638771282315));
#46894=CARTESIAN_POINT('Ctrl Pts',(2.48825428288242,-1.,3.17903698136679));
#46895=CARTESIAN_POINT('Ctrl Pts',(2.48825428288242,1.,3.17903698136679));
#46896=CARTESIAN_POINT('Ctrl Pts',(2.48604065348619,-1.,3.17170518863357));
#46897=CARTESIAN_POINT('Ctrl Pts',(2.48604065348619,1.,3.17170518863357));
#46898=CARTESIAN_POINT('Ctrl Pts',(2.48378981792739,-1.,3.16439213290181));
#46899=CARTESIAN_POINT('Ctrl Pts',(2.48378981792739,1.,3.16439213290181));
#46900=CARTESIAN_POINT('Ctrl Pts',(2.48150133566568,-1.,3.15709802322735));
#46901=CARTESIAN_POINT('Ctrl Pts',(2.48150133566568,1.,3.15709802322735));
#46902=CARTESIAN_POINT('Ctrl Pts',(2.47917529057016,-1.,3.14982373241335));
#46903=CARTESIAN_POINT('Ctrl Pts',(2.47917529057016,1.,3.14982373241335));
#46904=CARTESIAN_POINT('Ctrl Pts',(2.47681245356095,-1.,3.14257099546531));
#46905=CARTESIAN_POINT('Ctrl Pts',(2.47681245356095,1.,3.14257099546531));
#46906=CARTESIAN_POINT('Ctrl Pts',(2.47441378371923,-1.,3.13534181229282));
#46907=CARTESIAN_POINT('Ctrl Pts',(2.47441378371923,1.,3.13534181229282));
#46908=CARTESIAN_POINT('Ctrl Pts',(2.47197997765868,-1.,3.12813790805948));
#46909=CARTESIAN_POINT('Ctrl Pts',(2.47197997765868,1.,3.12813790805948));
#46910=CARTESIAN_POINT('Ctrl Pts',(2.4695109894747,-1.,3.12096015766984));
#46911=CARTESIAN_POINT('Ctrl Pts',(2.4695109894747,1.,3.12096015766984));
#46912=CARTESIAN_POINT('Ctrl Pts',(2.46700558843507,-1.,3.11380805536124));
#46913=CARTESIAN_POINT('Ctrl Pts',(2.46700558843507,1.,3.11380805536124));
#46914=CARTESIAN_POINT('Ctrl Pts',(2.46446082979645,-1.,3.10667907901981));
#46915=CARTESIAN_POINT('Ctrl Pts',(2.46446082979645,1.,3.10667907901981));
#46916=CARTESIAN_POINT('Ctrl Pts',(2.4618730850188,-1.,3.09956993697048));
#46917=CARTESIAN_POINT('Ctrl Pts',(2.4618730850188,1.,3.09956993697048));
#46918=CARTESIAN_POINT('Ctrl Pts',(2.45923912563875,-1.,3.09247787931881));
#46919=CARTESIAN_POINT('Ctrl Pts',(2.45923912563875,1.,3.09247787931881));
#46920=CARTESIAN_POINT('Ctrl Pts',(2.45655725437037,-1.,3.08540206545313));
#46921=CARTESIAN_POINT('Ctrl Pts',(2.45655725437037,1.,3.08540206545313));
#46922=CARTESIAN_POINT('Ctrl Pts',(2.45382826787795,-1.,3.07834472886145));
#46923=CARTESIAN_POINT('Ctrl Pts',(2.45382826787795,1.,3.07834472886145));
#46924=CARTESIAN_POINT('Ctrl Pts',(2.45105688854432,-1.,3.0713129052131));
#46925=CARTESIAN_POINT('Ctrl Pts',(2.45105688854432,1.,3.0713129052131));
#46926=CARTESIAN_POINT('Ctrl Pts',(2.44824970516557,-1.,3.06431596421422));
#46927=CARTESIAN_POINT('Ctrl Pts',(2.44824970516557,1.,3.06431596421422));
#46928=CARTESIAN_POINT('Ctrl Pts',(2.44541251892568,-1.,3.05736242671521));
#46929=CARTESIAN_POINT('Ctrl Pts',(2.44541251892568,1.,3.05736242671521));
#46930=CARTESIAN_POINT('Ctrl Pts',(2.44254768923109,-1.,3.05045678021509));
#46931=CARTESIAN_POINT('Ctrl Pts',(2.44254768923109,1.,3.05045678021509));
#46932=CARTESIAN_POINT('Ctrl Pts',(2.43965194061849,-1.,3.04359685040545));
#46933=CARTESIAN_POINT('Ctrl Pts',(2.43965194061849,1.,3.04359685040545));
#46934=CARTESIAN_POINT('Ctrl Pts',(2.43671278042394,-1.,3.03676949672797));
#46935=CARTESIAN_POINT('Ctrl Pts',(2.43671278042394,1.,3.03676949672797));
#46936=CARTESIAN_POINT('Ctrl Pts',(2.43371241361462,-1.,3.02995534946946));
#46937=CARTESIAN_POINT('Ctrl Pts',(2.43371241361462,1.,3.02995534946946));
#46938=CARTESIAN_POINT('Ctrl Pts',(2.43063415586615,-1.,3.02313656035977));
#46939=CARTESIAN_POINT('Ctrl Pts',(2.43063415586615,1.,3.02313656035977));
#46940=CARTESIAN_POINT('Ctrl Pts',(2.4274685626416,-1.,3.01630420830494));
#46941=CARTESIAN_POINT('Ctrl Pts',(2.4274685626416,1.,3.01630420830494));
#46942=CARTESIAN_POINT('Ctrl Pts',(2.42421849439625,-1.,3.00946442616674));
#46943=CARTESIAN_POINT('Ctrl Pts',(2.42421849439625,1.,3.00946442616674));
#46944=CARTESIAN_POINT('Ctrl Pts',(2.42090763946812,-1.,3.00264868586038));
#46945=CARTESIAN_POINT('Ctrl Pts',(2.42090763946812,1.,3.00264868586038));
#46946=CARTESIAN_POINT('Ctrl Pts',(2.4175732450056,-1.,2.99590509293561));
#46947=CARTESIAN_POINT('Ctrl Pts',(2.4175732450056,1.,2.99590509293561));
#46948=CARTESIAN_POINT('Ctrl Pts',(2.4142506419963,-1.,2.98927983005851));
#46949=CARTESIAN_POINT('Ctrl Pts',(2.4142506419963,1.,2.98927983005851));
#46950=CARTESIAN_POINT('Ctrl Pts',(2.41095909342591,-1.,2.98280015815132));
#46951=CARTESIAN_POINT('Ctrl Pts',(2.41095909342591,1.,2.98280015815132));
#46952=CARTESIAN_POINT('Ctrl Pts',(2.40768975073691,-1.,2.97646002822395));
#46953=CARTESIAN_POINT('Ctrl Pts',(2.40768975073691,1.,2.97646002822395));
#46954=CARTESIAN_POINT('Ctrl Pts',(2.40438604734848,-1.,2.97019641312272));
#46955=CARTESIAN_POINT('Ctrl Pts',(2.40438604734848,1.,2.97019641312272));
#46956=CARTESIAN_POINT('Ctrl Pts',(2.40095565711535,-1.,2.96390432240181));
#46957=CARTESIAN_POINT('Ctrl Pts',(2.40095565711535,1.,2.96390432240181));
#46958=CARTESIAN_POINT('Ctrl Pts',(2.39730553974412,-1.,2.95748006482811));
#46959=CARTESIAN_POINT('Ctrl Pts',(2.39730553974412,1.,2.95748006482811));
#46960=CARTESIAN_POINT('Ctrl Pts',(2.39337207631613,-1.,2.95085857128372));
#46961=CARTESIAN_POINT('Ctrl Pts',(2.39337207631613,1.,2.95085857128372));
#46962=CARTESIAN_POINT('Ctrl Pts',(2.38914929090806,-1.,2.94404820669135));
#46963=CARTESIAN_POINT('Ctrl Pts',(2.38914929090806,1.,2.94404820669135));
#46964=CARTESIAN_POINT('Ctrl Pts',(2.38472771516476,-1.,2.93717903280599));
#46965=CARTESIAN_POINT('Ctrl Pts',(2.38472771516476,1.,2.93717903280599));
#46966=CARTESIAN_POINT('Ctrl Pts',(2.3802898958232,-1.,2.93049643640517));
#46967=CARTESIAN_POINT('Ctrl Pts',(2.3802898958232,1.,2.93049643640517));
#46968=CARTESIAN_POINT('Ctrl Pts',(2.37606510524271,-1.,2.92430340582912));
#46969=CARTESIAN_POINT('Ctrl Pts',(2.37606510524271,1.,2.92430340582912));
#46970=CARTESIAN_POINT('Ctrl Pts',(2.37229381109939,-1.,2.9189150379156));
#46971=CARTESIAN_POINT('Ctrl Pts',(2.37229381109939,1.,2.9189150379156));
#46972=CARTESIAN_POINT('Ctrl Pts',(2.36919161373074,-1.,2.91461249883016));
#46973=CARTESIAN_POINT('Ctrl Pts',(2.36919161373074,1.,2.91461249883016));
#46974=CARTESIAN_POINT('Ctrl Pts',(2.36690501170317,-1.,2.9115863784165));
#46975=CARTESIAN_POINT('Ctrl Pts',(2.36690501170317,1.,2.9115863784165));
#46976=CARTESIAN_POINT('Ctrl Pts',(2.36578327194396,-1.,2.91025813829606));
#46977=CARTESIAN_POINT('Ctrl Pts',(2.36578327194396,1.,2.91025813829606));
#46978=CARTESIAN_POINT('Ctrl Pts',(2.36535052956704,-1.,2.90989022547738));
#46979=CARTESIAN_POINT('Ctrl Pts',(2.36535052956704,1.,2.90989022547738));
#46980=CARTESIAN_POINT('Ctrl Pts',(2.36524348105023,-1.,2.90992398626098));
#46981=CARTESIAN_POINT('Ctrl Pts',(2.36524348105023,1.,2.90992398626098));
#46982=CARTESIAN_POINT('Ctrl Pts',(2.36523532225181,-1.,2.91001063062876));
#46983=CARTESIAN_POINT('Ctrl Pts',(2.36523532225181,1.,2.91001063062876));
#46984=CARTESIAN_POINT('',(2.52982887637028,1.,3.35260583073571));
#46985=CARTESIAN_POINT('Ctrl Pts',(2.52982887637028,1.,3.35260583073571));
#46986=CARTESIAN_POINT('Ctrl Pts',(2.52954136549357,1.,3.35105973714426));
#46987=CARTESIAN_POINT('Ctrl Pts',(2.5289632161143,1.,3.34796903577628));
#46988=CARTESIAN_POINT('Ctrl Pts',(2.52808660916879,1.,3.34333744117093));
#46989=CARTESIAN_POINT('Ctrl Pts',(2.52689902691551,1.,3.33717090000955));
#46990=CARTESIAN_POINT('Ctrl Pts',(2.52538321165774,1.,3.32947762189049));
#46991=CARTESIAN_POINT('Ctrl Pts',(2.52383598396878,1.,3.32179931079521));
#46992=CARTESIAN_POINT('Ctrl Pts',(2.52225724871375,1.,3.31413607874727));
#46993=CARTESIAN_POINT('Ctrl Pts',(2.52064689568167,1.,3.30648808814986));
#46994=CARTESIAN_POINT('Ctrl Pts',(2.51900480700548,1.,3.29885556387661));
#46995=CARTESIAN_POINT('Ctrl Pts',(2.51733085123316,1.,3.2912387729863));
#46996=CARTESIAN_POINT('Ctrl Pts',(2.51562487464214,1.,3.28363799702583));
#46997=CARTESIAN_POINT('Ctrl Pts',(2.51388669270329,1.,3.27605350473048));
#46998=CARTESIAN_POINT('Ctrl Pts',(2.51211608411539,1.,3.26848552888271));
#46999=CARTESIAN_POINT('Ctrl Pts',(2.51031277813697,1.,3.26093423001716));
#47000=CARTESIAN_POINT('Ctrl Pts',(2.50847647070936,1.,3.25339971461265));
#47001=CARTESIAN_POINT('Ctrl Pts',(2.50660685940645,1.,3.24588208984042));
#47002=CARTESIAN_POINT('Ctrl Pts',(2.50470367580078,1.,3.23838151080383));
#47003=CARTESIAN_POINT('Ctrl Pts',(2.50276671338074,1.,3.23089822320596));
#47004=CARTESIAN_POINT('Ctrl Pts',(2.5007958720187,1.,3.22343262620387));
#47005=CARTESIAN_POINT('Ctrl Pts',(2.49879114599293,1.,3.21598526261157));
#47006=CARTESIAN_POINT('Ctrl Pts',(2.49675252647298,1.,3.2085566984974));
#47007=CARTESIAN_POINT('Ctrl Pts',(2.49467992057726,1.,3.20114742397549));
#47008=CARTESIAN_POINT('Ctrl Pts',(2.4925730723986,1.,3.19375775555814));
#47009=CARTESIAN_POINT('Ctrl Pts',(2.49043146334095,1.,3.18638771282315));
#47010=CARTESIAN_POINT('Ctrl Pts',(2.48825428288242,1.,3.17903698136679));
#47011=CARTESIAN_POINT('Ctrl Pts',(2.48604065348619,1.,3.17170518863357));
#47012=CARTESIAN_POINT('Ctrl Pts',(2.48378981792739,1.,3.16439213290181));
#47013=CARTESIAN_POINT('Ctrl Pts',(2.48150133566568,1.,3.15709802322735));
#47014=CARTESIAN_POINT('Ctrl Pts',(2.47917529057016,1.,3.14982373241335));
#47015=CARTESIAN_POINT('Ctrl Pts',(2.47681245356095,1.,3.14257099546531));
#47016=CARTESIAN_POINT('Ctrl Pts',(2.47441378371923,1.,3.13534181229282));
#47017=CARTESIAN_POINT('Ctrl Pts',(2.47197997765868,1.,3.12813790805948));
#47018=CARTESIAN_POINT('Ctrl Pts',(2.4695109894747,1.,3.12096015766984));
#47019=CARTESIAN_POINT('Ctrl Pts',(2.46700558843507,1.,3.11380805536124));
#47020=CARTESIAN_POINT('Ctrl Pts',(2.46446082979645,1.,3.10667907901981));
#47021=CARTESIAN_POINT('Ctrl Pts',(2.4618730850188,1.,3.09956993697048));
#47022=CARTESIAN_POINT('Ctrl Pts',(2.45923912563875,1.,3.09247787931881));
#47023=CARTESIAN_POINT('Ctrl Pts',(2.45655725437037,1.,3.08540206545313));
#47024=CARTESIAN_POINT('Ctrl Pts',(2.45382826787795,1.,3.07834472886145));
#47025=CARTESIAN_POINT('Ctrl Pts',(2.45105688854432,1.,3.0713129052131));
#47026=CARTESIAN_POINT('Ctrl Pts',(2.44824970516557,1.,3.06431596421422));
#47027=CARTESIAN_POINT('Ctrl Pts',(2.44541251892568,1.,3.05736242671521));
#47028=CARTESIAN_POINT('Ctrl Pts',(2.44254768923109,1.,3.05045678021509));
#47029=CARTESIAN_POINT('Ctrl Pts',(2.43965194061849,1.,3.04359685040545));
#47030=CARTESIAN_POINT('Ctrl Pts',(2.43671278042394,1.,3.03676949672797));
#47031=CARTESIAN_POINT('Ctrl Pts',(2.43371241361462,1.,3.02995534946946));
#47032=CARTESIAN_POINT('Ctrl Pts',(2.43063415586615,1.,3.02313656035977));
#47033=CARTESIAN_POINT('Ctrl Pts',(2.4274685626416,1.,3.01630420830494));
#47034=CARTESIAN_POINT('Ctrl Pts',(2.42421849439625,1.,3.00946442616674));
#47035=CARTESIAN_POINT('Ctrl Pts',(2.42090763946812,1.,3.00264868586038));
#47036=CARTESIAN_POINT('Ctrl Pts',(2.4175732450056,1.,2.99590509293561));
#47037=CARTESIAN_POINT('Ctrl Pts',(2.4142506419963,1.,2.98927983005851));
#47038=CARTESIAN_POINT('Ctrl Pts',(2.41095909342591,1.,2.98280015815132));
#47039=CARTESIAN_POINT('Ctrl Pts',(2.40768975073691,1.,2.97646002822395));
#47040=CARTESIAN_POINT('Ctrl Pts',(2.40438604734848,1.,2.97019641312272));
#47041=CARTESIAN_POINT('Ctrl Pts',(2.40095565711535,1.,2.96390432240181));
#47042=CARTESIAN_POINT('Ctrl Pts',(2.39730553974412,1.,2.95748006482811));
#47043=CARTESIAN_POINT('Ctrl Pts',(2.39337207631613,1.,2.95085857128372));
#47044=CARTESIAN_POINT('Ctrl Pts',(2.38914929090806,1.,2.94404820669135));
#47045=CARTESIAN_POINT('Ctrl Pts',(2.38472771516476,1.,2.93717903280599));
#47046=CARTESIAN_POINT('Ctrl Pts',(2.3802898958232,1.,2.93049643640517));
#47047=CARTESIAN_POINT('Ctrl Pts',(2.37606510524271,1.,2.92430340582912));
#47048=CARTESIAN_POINT('Ctrl Pts',(2.37229381109939,1.,2.9189150379156));
#47049=CARTESIAN_POINT('Ctrl Pts',(2.36919161373074,1.,2.91461249883016));
#47050=CARTESIAN_POINT('Ctrl Pts',(2.36707658451709,1.,2.91181344022628));
#47051=CARTESIAN_POINT('Ctrl Pts',(2.36599991765853,1.,2.91051690822262));
#47052=CARTESIAN_POINT('Ctrl Pts',(2.36553202948741,1.,2.91005770527771));
#47053=CARTESIAN_POINT('Ctrl Pts',(2.3653621118858,1.,2.90995756655559));
#47054=CARTESIAN_POINT('Ctrl Pts',(2.36531447826213,1.,2.90994629141563));
#47055=CARTESIAN_POINT('',(2.52982887637028,0.,3.35260583073571));
#47056=CARTESIAN_POINT('Ctrl Pts',(2.03668666247593,-1.,3.1487152044751));
#47057=CARTESIAN_POINT('Ctrl Pts',(2.03668666247593,1.,3.1487152044751));
#47058=CARTESIAN_POINT('Ctrl Pts',(2.03660173757879,-1.,3.14869618937258));
#47059=CARTESIAN_POINT('Ctrl Pts',(2.03660173757879,1.,3.14869618937258));
#47060=CARTESIAN_POINT('Ctrl Pts',(2.03653654935591,-1.,3.14878756590812));
#47061=CARTESIAN_POINT('Ctrl Pts',(2.03653654935591,1.,3.14878756590812));
#47062=CARTESIAN_POINT('Ctrl Pts',(2.03675273049189,-1.,3.14931281968048));
#47063=CARTESIAN_POINT('Ctrl Pts',(2.03675273049189,1.,3.14931281968048));
#47064=CARTESIAN_POINT('Ctrl Pts',(2.03766932526445,-1.,3.15079010635742));
#47065=CARTESIAN_POINT('Ctrl Pts',(2.03766932526445,1.,3.15079010635742));
#47066=CARTESIAN_POINT('Ctrl Pts',(2.03984073791519,-1.,3.15389991674792));
#47067=CARTESIAN_POINT('Ctrl Pts',(2.03984073791519,1.,3.15389991674792));
#47068=CARTESIAN_POINT('Ctrl Pts',(2.04297406404027,-1.,3.15817983946367));
#47069=CARTESIAN_POINT('Ctrl Pts',(2.04297406404027,1.,3.15817983946367));
#47070=CARTESIAN_POINT('Ctrl Pts',(2.04693331247446,-1.,3.16343165058912));
#47071=CARTESIAN_POINT('Ctrl Pts',(2.04693331247446,1.,3.16343165058912));
#47072=CARTESIAN_POINT('Ctrl Pts',(2.05151770247233,-1.,3.16936341689527));
#47073=CARTESIAN_POINT('Ctrl Pts',(2.05151770247233,1.,3.16936341689527));
#47074=CARTESIAN_POINT('Ctrl Pts',(2.05650186773132,-1.,3.17564906975371));
#47075=CARTESIAN_POINT('Ctrl Pts',(2.05650186773132,1.,3.17564906975371));
#47076=CARTESIAN_POINT('Ctrl Pts',(2.06166849827101,-1.,3.18197692964614));
#47077=CARTESIAN_POINT('Ctrl Pts',(2.06166849827101,1.,3.18197692964614));
#47078=CARTESIAN_POINT('Ctrl Pts',(2.06684062744112,-1.,3.18809755562368));
#47079=CARTESIAN_POINT('Ctrl Pts',(2.06684062744112,1.,3.18809755562368));
#47080=CARTESIAN_POINT('Ctrl Pts',(2.07192253497857,-1.,3.19388465568252));
#47081=CARTESIAN_POINT('Ctrl Pts',(2.07192253497857,1.,3.19388465568252));
#47082=CARTESIAN_POINT('Ctrl Pts',(2.07690441870722,-1.,3.19934132836019));
#47083=CARTESIAN_POINT('Ctrl Pts',(2.07690441870722,1.,3.19934132836019));
#47084=CARTESIAN_POINT('Ctrl Pts',(2.08182850370878,-1.,3.2045481863073));
#47085=CARTESIAN_POINT('Ctrl Pts',(2.08182850370878,1.,3.2045481863073));
#47086=CARTESIAN_POINT('Ctrl Pts',(2.08676465517455,-1.,3.20962575845463));
#47087=CARTESIAN_POINT('Ctrl Pts',(2.08676465517455,1.,3.20962575845463));
#47088=CARTESIAN_POINT('Ctrl Pts',(2.09178419460443,-1.,3.21469429601654));
#47089=CARTESIAN_POINT('Ctrl Pts',(2.09178419460443,1.,3.21469429601654));
#47090=CARTESIAN_POINT('Ctrl Pts',(2.09692958434895,-1.,3.21982707347009));
#47091=CARTESIAN_POINT('Ctrl Pts',(2.09692958434895,1.,3.21982707347009));
#47092=CARTESIAN_POINT('Ctrl Pts',(2.10220384298492,-1.,3.22503437553434));
#47093=CARTESIAN_POINT('Ctrl Pts',(2.10220384298492,1.,3.22503437553434));
#47094=CARTESIAN_POINT('Ctrl Pts',(2.10758699642451,-1.,3.23028945793289));
#47095=CARTESIAN_POINT('Ctrl Pts',(2.10758699642451,1.,3.23028945793289));
#47096=CARTESIAN_POINT('Ctrl Pts',(2.11304604021773,-1.,3.23554444767099));
#47097=CARTESIAN_POINT('Ctrl Pts',(2.11304604021773,1.,3.23554444767099));
#47098=CARTESIAN_POINT('Ctrl Pts',(2.11854673326979,-1.,3.24074905517293));
#47099=CARTESIAN_POINT('Ctrl Pts',(2.11854673326979,1.,3.24074905517293));
#47100=CARTESIAN_POINT('Ctrl Pts',(2.12406646410962,-1.,3.24587102613376));
#47101=CARTESIAN_POINT('Ctrl Pts',(2.12406646410962,1.,3.24587102613376));
#47102=CARTESIAN_POINT('Ctrl Pts',(2.12960028396832,-1.,3.25090574494028));
#47103=CARTESIAN_POINT('Ctrl Pts',(2.12960028396832,1.,3.25090574494028));
#47104=CARTESIAN_POINT('Ctrl Pts',(2.13515375878803,-1.,3.25586495065054));
#47105=CARTESIAN_POINT('Ctrl Pts',(2.13515375878803,1.,3.25586495065054));
#47106=CARTESIAN_POINT('Ctrl Pts',(2.14073870754264,-1.,3.26077002641879));
#47107=CARTESIAN_POINT('Ctrl Pts',(2.14073870754264,1.,3.26077002641879));
#47108=CARTESIAN_POINT('Ctrl Pts',(2.1463680529566,-1.,3.26564388189759));
#47109=CARTESIAN_POINT('Ctrl Pts',(2.1463680529566,1.,3.26564388189759));
#47110=CARTESIAN_POINT('Ctrl Pts',(2.15205043199808,-1.,3.27050245897228));
#47111=CARTESIAN_POINT('Ctrl Pts',(2.15205043199808,1.,3.27050245897228));
#47112=CARTESIAN_POINT('Ctrl Pts',(2.15778690038347,-1.,3.27534954469187));
#47113=CARTESIAN_POINT('Ctrl Pts',(2.15778690038347,1.,3.27534954469187));
#47114=CARTESIAN_POINT('Ctrl Pts',(2.16357391934425,-1.,3.280181508414));
#47115=CARTESIAN_POINT('Ctrl Pts',(2.16357391934425,1.,3.280181508414));
#47116=CARTESIAN_POINT('Ctrl Pts',(2.16940517773455,-1.,3.28499019979724));
#47117=CARTESIAN_POINT('Ctrl Pts',(2.16940517773455,1.,3.28499019979724));
#47118=CARTESIAN_POINT('Ctrl Pts',(2.17527380048423,-1.,3.28976645712568));
#47119=CARTESIAN_POINT('Ctrl Pts',(2.17527380048423,1.,3.28976645712568));
#47120=CARTESIAN_POINT('Ctrl Pts',(2.18117455557065,-1.,3.2945036150049));
#47121=CARTESIAN_POINT('Ctrl Pts',(2.18117455557065,1.,3.2945036150049));
#47122=CARTESIAN_POINT('Ctrl Pts',(2.18710556500327,-1.,3.29920022557639));
#47123=CARTESIAN_POINT('Ctrl Pts',(2.18710556500327,1.,3.29920022557639));
#47124=CARTESIAN_POINT('Ctrl Pts',(2.19306710376111,-1.,3.30385816281831));
#47125=CARTESIAN_POINT('Ctrl Pts',(2.19306710376111,1.,3.30385816281831));
#47126=CARTESIAN_POINT('Ctrl Pts',(2.19906078949922,-1.,3.30848134694595));
#47127=CARTESIAN_POINT('Ctrl Pts',(2.19906078949922,1.,3.30848134694595));
#47128=CARTESIAN_POINT('Ctrl Pts',(2.20508863150607,-1.,3.31307424608949));
#47129=CARTESIAN_POINT('Ctrl Pts',(2.20508863150607,1.,3.31307424608949));
#47130=CARTESIAN_POINT('Ctrl Pts',(2.21115211847875,-1.,3.31764044024235));
#47131=CARTESIAN_POINT('Ctrl Pts',(2.21115211847875,1.,3.31764044024235));
#47132=CARTESIAN_POINT('Ctrl Pts',(2.21725135110898,-1.,3.32218125618968));
#47133=CARTESIAN_POINT('Ctrl Pts',(2.21725135110898,1.,3.32218125618968));
#47134=CARTESIAN_POINT('Ctrl Pts',(2.22338548312772,-1.,3.3266964672289));
#47135=CARTESIAN_POINT('Ctrl Pts',(2.22338548312772,1.,3.3266964672289));
#47136=CARTESIAN_POINT('Ctrl Pts',(2.22955308907233,-1.,3.33118487773611));
#47137=CARTESIAN_POINT('Ctrl Pts',(2.22955308907233,1.,3.33118487773611));
#47138=CARTESIAN_POINT('Ctrl Pts',(2.23575256328812,-1.,3.33564495756482));
#47139=CARTESIAN_POINT('Ctrl Pts',(2.23575256328812,1.,3.33564495756482));
#47140=CARTESIAN_POINT('Ctrl Pts',(2.24198249391422,-1.,3.34007543738025));
#47141=CARTESIAN_POINT('Ctrl Pts',(2.24198249391422,1.,3.34007543738025));
#47142=CARTESIAN_POINT('Ctrl Pts',(2.24824207678256,-1.,3.34447596770723));
#47143=CARTESIAN_POINT('Ctrl Pts',(2.24824207678256,1.,3.34447596770723));
#47144=CARTESIAN_POINT('Ctrl Pts',(2.25453097693483,-1.,3.34884690292285));
#47145=CARTESIAN_POINT('Ctrl Pts',(2.25453097693483,1.,3.34884690292285));
#47146=CARTESIAN_POINT('Ctrl Pts',(2.26084915222449,-1.,3.35318902552626));
#47147=CARTESIAN_POINT('Ctrl Pts',(2.26084915222449,1.,3.35318902552626));
#47148=CARTESIAN_POINT('Ctrl Pts',(2.26719668579909,-1.,3.35750328523061));
#47149=CARTESIAN_POINT('Ctrl Pts',(2.26719668579909,1.,3.35750328523061));
#47150=CARTESIAN_POINT('Ctrl Pts',(2.2735736262093,-1.,3.36179055004409));
#47151=CARTESIAN_POINT('Ctrl Pts',(2.2735736262093,1.,3.36179055004409));
#47152=CARTESIAN_POINT('Ctrl Pts',(2.27997979458037,-1.,3.36605130713076));
#47153=CARTESIAN_POINT('Ctrl Pts',(2.27997979458037,1.,3.36605130713076));
#47154=CARTESIAN_POINT('Ctrl Pts',(2.28641481081137,-1.,3.37028570206488));
#47155=CARTESIAN_POINT('Ctrl Pts',(2.28641481081137,1.,3.37028570206488));
#47156=CARTESIAN_POINT('Ctrl Pts',(2.29287818007393,-1.,3.37449367172826));
#47157=CARTESIAN_POINT('Ctrl Pts',(2.29287818007393,1.,3.37449367172826));
#47158=CARTESIAN_POINT('Ctrl Pts',(2.29936936127624,-1.,3.37867504959433));
#47159=CARTESIAN_POINT('Ctrl Pts',(2.29936936127624,1.,3.37867504959433));
#47160=CARTESIAN_POINT('Ctrl Pts',(2.30588783640343,-1.,3.3828296733661));
#47161=CARTESIAN_POINT('Ctrl Pts',(2.30588783640343,1.,3.3828296733661));
#47162=CARTESIAN_POINT('Ctrl Pts',(2.31243319489367,-1.,3.38695751492462));
#47163=CARTESIAN_POINT('Ctrl Pts',(2.31243319489367,1.,3.38695751492462));
#47164=CARTESIAN_POINT('Ctrl Pts',(2.31900513925424,-1.,3.39105869474822));
#47165=CARTESIAN_POINT('Ctrl Pts',(2.31900513925424,1.,3.39105869474822));
#47166=CARTESIAN_POINT('Ctrl Pts',(2.3256034390248,-1.,3.39513342019756));
#47167=CARTESIAN_POINT('Ctrl Pts',(2.3256034390248,1.,3.39513342019756));
#47168=CARTESIAN_POINT('Ctrl Pts',(2.33222789882489,-1.,3.39918194577956));
#47169=CARTESIAN_POINT('Ctrl Pts',(2.33222789882489,1.,3.39918194577956));
#47170=CARTESIAN_POINT('Ctrl Pts',(2.33887832342782,-1.,3.40320452776743));
#47171=CARTESIAN_POINT('Ctrl Pts',(2.33887832342782,1.,3.40320452776743));
#47172=CARTESIAN_POINT('Ctrl Pts',(2.34555447649188,-1.,3.40720137404297));
#47173=CARTESIAN_POINT('Ctrl Pts',(2.34555447649188,1.,3.40720137404297));
#47174=CARTESIAN_POINT('Ctrl Pts',(2.35225606824109,-1.,3.41117262314119));
#47175=CARTESIAN_POINT('Ctrl Pts',(2.35225606824109,1.,3.41117262314119));
#47176=CARTESIAN_POINT('Ctrl Pts',(2.35898278606946,-1.,3.41511836751469));
#47177=CARTESIAN_POINT('Ctrl Pts',(2.35898278606946,1.,3.41511836751469));
#47178=CARTESIAN_POINT('Ctrl Pts',(2.36573431470642,-1.,3.41903866635852));
#47179=CARTESIAN_POINT('Ctrl Pts',(2.36573431470642,1.,3.41903866635852));
#47180=CARTESIAN_POINT('Ctrl Pts',(2.37251035954292,-1.,3.42293356216511));
#47181=CARTESIAN_POINT('Ctrl Pts',(2.37251035954292,1.,3.42293356216511));
#47182=CARTESIAN_POINT('Ctrl Pts',(2.37931067028926,-1.,3.42680309754399));
#47183=CARTESIAN_POINT('Ctrl Pts',(2.37931067028926,1.,3.42680309754399));
#47184=CARTESIAN_POINT('Ctrl Pts',(2.38613505843552,-1.,3.4306473271292));
#47185=CARTESIAN_POINT('Ctrl Pts',(2.38613505843552,1.,3.4306473271292));
#47186=CARTESIAN_POINT('Ctrl Pts',(2.39298338804493,-1.,3.4344663067854));
#47187=CARTESIAN_POINT('Ctrl Pts',(2.39298338804493,1.,3.4344663067854));
#47188=CARTESIAN_POINT('Ctrl Pts',(2.39848113410292,-1.,3.43750133064416));
#47189=CARTESIAN_POINT('Ctrl Pts',(2.39848113410292,1.,3.43750133064416));
#47190=CARTESIAN_POINT('Ctrl Pts',(2.40261515589405,-1.,3.43976627484234));
#47191=CARTESIAN_POINT('Ctrl Pts',(2.40261515589405,1.,3.43976627484234));
#47192=CARTESIAN_POINT('Ctrl Pts',(2.4053759295909,-1.,3.44127120683039));
#47193=CARTESIAN_POINT('Ctrl Pts',(2.4053759295909,1.,3.44127120683039));
#47194=CARTESIAN_POINT('Ctrl Pts',(2.40675750623143,-1.,3.44202241512147));
#47195=CARTESIAN_POINT('Ctrl Pts',(2.40675750623143,1.,3.44202241512147));
#47196=CARTESIAN_POINT('',(2.03660101169714,1.,3.14877060440328));
#47197=CARTESIAN_POINT('Ctrl Pts',(2.03660101169714,-1.,3.14877060440327));
#47198=CARTESIAN_POINT('Ctrl Pts',(2.03660101169714,-0.666666666666667,
3.14877060440327));
#47199=CARTESIAN_POINT('Ctrl Pts',(2.03660101169714,-0.333333333333333,
3.14877060440327));
#47200=CARTESIAN_POINT('Ctrl Pts',(2.03660101169714,0.333333333333333,3.14877060440327));
#47201=CARTESIAN_POINT('Ctrl Pts',(2.03660101169714,0.666666666666667,3.14877060440327));
#47202=CARTESIAN_POINT('Ctrl Pts',(2.03660101169714,1.,3.14877060440327));
#47203=CARTESIAN_POINT('',(2.40675750623143,1.,3.44202241512147));
#47204=CARTESIAN_POINT('',(2.40675750623143,0.,3.44202241512147));
#47205=CARTESIAN_POINT('Ctrl Pts',(2.03660101169714,1.,3.14877060440328));
#47206=CARTESIAN_POINT('Ctrl Pts',(2.03659701539259,1.,3.14881939088124));
#47207=CARTESIAN_POINT('Ctrl Pts',(2.03663974554932,1.,3.1490119366901));
#47208=CARTESIAN_POINT('Ctrl Pts',(2.03693188810545,1.,3.14959882629805));
#47209=CARTESIAN_POINT('Ctrl Pts',(2.03783225495961,1.,3.15102344775328));
#47210=CARTESIAN_POINT('Ctrl Pts',(2.03984073791519,1.,3.15389991674792));
#47211=CARTESIAN_POINT('Ctrl Pts',(2.04297406404027,1.,3.15817983946367));
#47212=CARTESIAN_POINT('Ctrl Pts',(2.04693331247446,1.,3.16343165058912));
#47213=CARTESIAN_POINT('Ctrl Pts',(2.05151770247233,1.,3.16936341689527));
#47214=CARTESIAN_POINT('Ctrl Pts',(2.05650186773132,1.,3.17564906975371));
#47215=CARTESIAN_POINT('Ctrl Pts',(2.06166849827101,1.,3.18197692964614));
#47216=CARTESIAN_POINT('Ctrl Pts',(2.06684062744112,1.,3.18809755562368));
#47217=CARTESIAN_POINT('Ctrl Pts',(2.07192253497857,1.,3.19388465568252));
#47218=CARTESIAN_POINT('Ctrl Pts',(2.07690441870722,1.,3.19934132836019));
#47219=CARTESIAN_POINT('Ctrl Pts',(2.08182850370878,1.,3.2045481863073));
#47220=CARTESIAN_POINT('Ctrl Pts',(2.08676465517455,1.,3.20962575845463));
#47221=CARTESIAN_POINT('Ctrl Pts',(2.09178419460443,1.,3.21469429601654));
#47222=CARTESIAN_POINT('Ctrl Pts',(2.09692958434895,1.,3.21982707347009));
#47223=CARTESIAN_POINT('Ctrl Pts',(2.10220384298492,1.,3.22503437553434));
#47224=CARTESIAN_POINT('Ctrl Pts',(2.10758699642451,1.,3.23028945793289));
#47225=CARTESIAN_POINT('Ctrl Pts',(2.11304604021773,1.,3.23554444767099));
#47226=CARTESIAN_POINT('Ctrl Pts',(2.11854673326979,1.,3.24074905517293));
#47227=CARTESIAN_POINT('Ctrl Pts',(2.12406646410962,1.,3.24587102613376));
#47228=CARTESIAN_POINT('Ctrl Pts',(2.12960028396832,1.,3.25090574494028));
#47229=CARTESIAN_POINT('Ctrl Pts',(2.13515375878803,1.,3.25586495065054));
#47230=CARTESIAN_POINT('Ctrl Pts',(2.14073870754264,1.,3.26077002641879));
#47231=CARTESIAN_POINT('Ctrl Pts',(2.1463680529566,1.,3.26564388189759));
#47232=CARTESIAN_POINT('Ctrl Pts',(2.15205043199808,1.,3.27050245897228));
#47233=CARTESIAN_POINT('Ctrl Pts',(2.15778690038347,1.,3.27534954469187));
#47234=CARTESIAN_POINT('Ctrl Pts',(2.16357391934425,1.,3.280181508414));
#47235=CARTESIAN_POINT('Ctrl Pts',(2.16940517773455,1.,3.28499019979724));
#47236=CARTESIAN_POINT('Ctrl Pts',(2.17527380048423,1.,3.28976645712568));
#47237=CARTESIAN_POINT('Ctrl Pts',(2.18117455557065,1.,3.2945036150049));
#47238=CARTESIAN_POINT('Ctrl Pts',(2.18710556500327,1.,3.29920022557639));
#47239=CARTESIAN_POINT('Ctrl Pts',(2.19306710376111,1.,3.30385816281831));
#47240=CARTESIAN_POINT('Ctrl Pts',(2.19906078949922,1.,3.30848134694595));
#47241=CARTESIAN_POINT('Ctrl Pts',(2.20508863150607,1.,3.31307424608949));
#47242=CARTESIAN_POINT('Ctrl Pts',(2.21115211847875,1.,3.31764044024235));
#47243=CARTESIAN_POINT('Ctrl Pts',(2.21725135110898,1.,3.32218125618968));
#47244=CARTESIAN_POINT('Ctrl Pts',(2.22338548312772,1.,3.3266964672289));
#47245=CARTESIAN_POINT('Ctrl Pts',(2.22955308907233,1.,3.33118487773611));
#47246=CARTESIAN_POINT('Ctrl Pts',(2.23575256328812,1.,3.33564495756482));
#47247=CARTESIAN_POINT('Ctrl Pts',(2.24198249391422,1.,3.34007543738025));
#47248=CARTESIAN_POINT('Ctrl Pts',(2.24824207678256,1.,3.34447596770723));
#47249=CARTESIAN_POINT('Ctrl Pts',(2.25453097693483,1.,3.34884690292285));
#47250=CARTESIAN_POINT('Ctrl Pts',(2.26084915222449,1.,3.35318902552626));
#47251=CARTESIAN_POINT('Ctrl Pts',(2.26719668579909,1.,3.35750328523061));
#47252=CARTESIAN_POINT('Ctrl Pts',(2.2735736262093,1.,3.36179055004409));
#47253=CARTESIAN_POINT('Ctrl Pts',(2.27997979458037,1.,3.36605130713076));
#47254=CARTESIAN_POINT('Ctrl Pts',(2.28641481081137,1.,3.37028570206488));
#47255=CARTESIAN_POINT('Ctrl Pts',(2.29287818007393,1.,3.37449367172826));
#47256=CARTESIAN_POINT('Ctrl Pts',(2.29936936127624,1.,3.37867504959433));
#47257=CARTESIAN_POINT('Ctrl Pts',(2.30588783640343,1.,3.3828296733661));
#47258=CARTESIAN_POINT('Ctrl Pts',(2.31243319489367,1.,3.38695751492462));
#47259=CARTESIAN_POINT('Ctrl Pts',(2.31900513925424,1.,3.39105869474822));
#47260=CARTESIAN_POINT('Ctrl Pts',(2.3256034390248,1.,3.39513342019756));
#47261=CARTESIAN_POINT('Ctrl Pts',(2.33222789882489,1.,3.39918194577956));
#47262=CARTESIAN_POINT('Ctrl Pts',(2.33887832342782,1.,3.40320452776743));
#47263=CARTESIAN_POINT('Ctrl Pts',(2.34555447649188,1.,3.40720137404297));
#47264=CARTESIAN_POINT('Ctrl Pts',(2.35225606824109,1.,3.41117262314119));
#47265=CARTESIAN_POINT('Ctrl Pts',(2.35898278606946,1.,3.41511836751469));
#47266=CARTESIAN_POINT('Ctrl Pts',(2.36573431470642,1.,3.41903866635852));
#47267=CARTESIAN_POINT('Ctrl Pts',(2.37251035954292,1.,3.42293356216511));
#47268=CARTESIAN_POINT('Ctrl Pts',(2.37931067028926,1.,3.42680309754399));
#47269=CARTESIAN_POINT('Ctrl Pts',(2.38613505843552,1.,3.4306473271292));
#47270=CARTESIAN_POINT('Ctrl Pts',(2.39298338804493,1.,3.4344663067854));
#47271=CARTESIAN_POINT('Ctrl Pts',(2.39848113410292,1.,3.43750133064416));
#47272=CARTESIAN_POINT('Ctrl Pts',(2.40261515589405,1.,3.43976627484234));
#47273=CARTESIAN_POINT('Ctrl Pts',(2.4053759295909,1.,3.44127120683039));
#47274=CARTESIAN_POINT('Ctrl Pts',(2.40675750623143,1.,3.44202241512147));
#47275=CARTESIAN_POINT('Origin',(2.40675750623143,0.,3.44202241512147));
#47276=CARTESIAN_POINT('',(2.52982887637028,1.,3.35260583073571));
#47277=CARTESIAN_POINT('Origin',(0.,0.,0.));
#47278=CARTESIAN_POINT('',(1.88097764062697,1.,3.24413672884812));
#47279=CARTESIAN_POINT('Origin',(0.,1.,0.));
#47280=CARTESIAN_POINT('Ctrl Pts',(1.88097764062697,1.,3.24413672884812));
#47281=CARTESIAN_POINT('Ctrl Pts',(1.88097764062697,0.666666666666667,3.24413672884812));
#47282=CARTESIAN_POINT('Ctrl Pts',(1.88097764062697,0.333333333333333,3.24413672884812));
#47283=CARTESIAN_POINT('Ctrl Pts',(1.88097764062697,-0.333333333333333,
3.24413672884812));
#47284=CARTESIAN_POINT('Ctrl Pts',(1.88097764062697,-0.666666666666667,
3.24413672884812));
#47285=CARTESIAN_POINT('Ctrl Pts',(1.88097764062697,-1.,3.24413672884812));
#47286=CARTESIAN_POINT('Ctrl Pts',(1.97421938526992,-1.,3.70708211654725));
#47287=CARTESIAN_POINT('Ctrl Pts',(1.97421938526992,1.,3.70708211654725));
#47288=CARTESIAN_POINT('Ctrl Pts',(1.97417727645308,-1.,3.70551008132332));
#47289=CARTESIAN_POINT('Ctrl Pts',(1.97417727645308,1.,3.70551008132332));
#47290=CARTESIAN_POINT('Ctrl Pts',(1.97408973726715,-1.,3.70236698912904));
#47291=CARTESIAN_POINT('Ctrl Pts',(1.97408973726715,1.,3.70236698912904));
#47292=CARTESIAN_POINT('Ctrl Pts',(1.97394846383216,-1.,3.6976552856004));
#47293=CARTESIAN_POINT('Ctrl Pts',(1.97394846383216,1.,3.6976552856004));
#47294=CARTESIAN_POINT('Ctrl Pts',(1.97374016225483,-1.,3.69137888599902));
#47295=CARTESIAN_POINT('Ctrl Pts',(1.97374016225483,1.,3.69137888599902));
#47296=CARTESIAN_POINT('Ctrl Pts',(1.97344650304519,-1.,3.68354319915092));
#47297=CARTESIAN_POINT('Ctrl Pts',(1.97344650304519,1.,3.68354319915092));
#47298=CARTESIAN_POINT('Ctrl Pts',(1.97311947678516,-1.,3.67571738107084));
#47299=CARTESIAN_POINT('Ctrl Pts',(1.97311947678516,1.,3.67571738107084));
#47300=CARTESIAN_POINT('Ctrl Pts',(1.97275897198678,-1.,3.66790152752075));
#47301=CARTESIAN_POINT('Ctrl Pts',(1.97275897198678,1.,3.66790152752075));
#47302=CARTESIAN_POINT('Ctrl Pts',(1.9723648543905,-1.,3.6600957816636));
#47303=CARTESIAN_POINT('Ctrl Pts',(1.9723648543905,1.,3.6600957816636));
#47304=CARTESIAN_POINT('Ctrl Pts',(1.97193697240239,-1.,3.652300347166));
#47305=CARTESIAN_POINT('Ctrl Pts',(1.97193697240239,1.,3.652300347166));
#47306=CARTESIAN_POINT('Ctrl Pts',(1.97147515441164,-1.,3.64451546723514));
#47307=CARTESIAN_POINT('Ctrl Pts',(1.97147515441164,1.,3.64451546723514));
#47308=CARTESIAN_POINT('Ctrl Pts',(1.97097920454464,-1.,3.63674139590412));
#47309=CARTESIAN_POINT('Ctrl Pts',(1.97097920454464,1.,3.63674139590412));
#47310=CARTESIAN_POINT('Ctrl Pts',(1.97044889850463,-1.,3.62897836973293));
#47311=CARTESIAN_POINT('Ctrl Pts',(1.97044889850463,1.,3.62897836973293));
#47312=CARTESIAN_POINT('Ctrl Pts',(1.96988398129978,-1.,3.62122658401893));
#47313=CARTESIAN_POINT('Ctrl Pts',(1.96988398129978,1.,3.62122658401893));
#47314=CARTESIAN_POINT('Ctrl Pts',(1.96928416040877,-1.,3.61348615496704));
#47315=CARTESIAN_POINT('Ctrl Pts',(1.96928416040877,1.,3.61348615496704));
#47316=CARTESIAN_POINT('Ctrl Pts',(1.9686491188594,-1.,3.60575714017989));
#47317=CARTESIAN_POINT('Ctrl Pts',(1.9686491188594,1.,3.60575714017989));
#47318=CARTESIAN_POINT('Ctrl Pts',(1.96797854118369,-1.,3.59803959819938));
#47319=CARTESIAN_POINT('Ctrl Pts',(1.96797854118369,1.,3.59803959819938));
#47320=CARTESIAN_POINT('Ctrl Pts',(1.96727213799544,-1.,3.59033364022801));
#47321=CARTESIAN_POINT('Ctrl Pts',(1.96727213799544,1.,3.59033364022801));
#47322=CARTESIAN_POINT('Ctrl Pts',(1.96652966688911,-1.,3.58263947663829));
#47323=CARTESIAN_POINT('Ctrl Pts',(1.96652966688911,1.,3.58263947663829));
#47324=CARTESIAN_POINT('Ctrl Pts',(1.96575096652789,-1.,3.57495748600959));
#47325=CARTESIAN_POINT('Ctrl Pts',(1.96575096652789,1.,3.57495748600959));
#47326=CARTESIAN_POINT('Ctrl Pts',(1.96493594634567,-1.,3.56728820357791));
#47327=CARTESIAN_POINT('Ctrl Pts',(1.96493594634567,1.,3.56728820357791));
#47328=CARTESIAN_POINT('Ctrl Pts',(1.96408450906812,-1.,3.55963218706096));
#47329=CARTESIAN_POINT('Ctrl Pts',(1.96408450906812,1.,3.55963218706096));
#47330=CARTESIAN_POINT('Ctrl Pts',(1.96319648628644,-1.,3.55198990600886));
#47331=CARTESIAN_POINT('Ctrl Pts',(1.96319648628644,1.,3.55198990600886));
#47332=CARTESIAN_POINT('Ctrl Pts',(1.96227157573067,-1.,3.54436163300443));
#47333=CARTESIAN_POINT('Ctrl Pts',(1.96227157573067,1.,3.54436163300443));
#47334=CARTESIAN_POINT('Ctrl Pts',(1.96130926212689,-1.,3.53674730625813));
#47335=CARTESIAN_POINT('Ctrl Pts',(1.96130926212689,1.,3.53674730625813));
#47336=CARTESIAN_POINT('Ctrl Pts',(1.96030879411566,-1.,3.52914648844351));
#47337=CARTESIAN_POINT('Ctrl Pts',(1.96030879411566,1.,3.52914648844351));
#47338=CARTESIAN_POINT('Ctrl Pts',(1.95926936324461,-1.,3.52155867431486));
#47339=CARTESIAN_POINT('Ctrl Pts',(1.95926936324461,1.,3.52155867431486));
#47340=CARTESIAN_POINT('Ctrl Pts',(1.95819025316779,-1.,3.51398354617794));
#47341=CARTESIAN_POINT('Ctrl Pts',(1.95819025316779,1.,3.51398354617794));
#47342=CARTESIAN_POINT('Ctrl Pts',(1.95707099606511,-1.,3.50642124159909));
#47343=CARTESIAN_POINT('Ctrl Pts',(1.95707099606511,1.,3.50642124159909));
#47344=CARTESIAN_POINT('Ctrl Pts',(1.95591153823661,-1.,3.49887263575583));
#47345=CARTESIAN_POINT('Ctrl Pts',(1.95591153823661,1.,3.49887263575583));
#47346=CARTESIAN_POINT('Ctrl Pts',(1.95471236969643,-1.,3.49133956289133));
#47347=CARTESIAN_POINT('Ctrl Pts',(1.95471236969643,1.,3.49133956289133));
#47348=CARTESIAN_POINT('Ctrl Pts',(1.95347412486308,-1.,3.48382414832634));
#47349=CARTESIAN_POINT('Ctrl Pts',(1.95347412486308,1.,3.48382414832634));
#47350=CARTESIAN_POINT('Ctrl Pts',(1.95219722189876,-1.,3.47632820495921));
#47351=CARTESIAN_POINT('Ctrl Pts',(1.95219722189876,1.,3.47632820495921));
#47352=CARTESIAN_POINT('Ctrl Pts',(1.95088147859876,-1.,3.46885258974191));
#47353=CARTESIAN_POINT('Ctrl Pts',(1.95088147859876,1.,3.46885258974191));
#47354=CARTESIAN_POINT('Ctrl Pts',(1.94952575850197,-1.,3.46139661060962));
#47355=CARTESIAN_POINT('Ctrl Pts',(1.94952575850197,1.,3.46139661060962));
#47356=CARTESIAN_POINT('Ctrl Pts',(1.94812754766524,-1.,3.45395731584051));
#47357=CARTESIAN_POINT('Ctrl Pts',(1.94812754766524,1.,3.45395731584051));
#47358=CARTESIAN_POINT('Ctrl Pts',(1.94668377715329,-1.,3.44653088665681));
#47359=CARTESIAN_POINT('Ctrl Pts',(1.94668377715329,1.,3.44653088665681));
#47360=CARTESIAN_POINT('Ctrl Pts',(1.94519168842879,-1.,3.43911410197687));
#47361=CARTESIAN_POINT('Ctrl Pts',(1.94519168842879,1.,3.43911410197687));
#47362=CARTESIAN_POINT('Ctrl Pts',(1.94364973660284,-1.,3.43170586602434));
#47363=CARTESIAN_POINT('Ctrl Pts',(1.94364973660284,1.,3.43170586602434));
#47364=CARTESIAN_POINT('Ctrl Pts',(1.94205835913696,-1.,3.42430850941503));
#47365=CARTESIAN_POINT('Ctrl Pts',(1.94205835913696,1.,3.42430850941503));
#47366=CARTESIAN_POINT('Ctrl Pts',(1.94042111965246,-1.,3.41692971994096));
#47367=CARTESIAN_POINT('Ctrl Pts',(1.94042111965246,1.,3.41692971994096));
#47368=CARTESIAN_POINT('Ctrl Pts',(1.93874306008143,-1.,3.40957978266642));
#47369=CARTESIAN_POINT('Ctrl Pts',(1.93874306008143,1.,3.40957978266642));
#47370=CARTESIAN_POINT('Ctrl Pts',(1.93702857723098,-1.,3.40226802104109));
#47371=CARTESIAN_POINT('Ctrl Pts',(1.93702857723098,1.,3.40226802104109));
#47372=CARTESIAN_POINT('Ctrl Pts',(1.93527929945985,-1.,3.39499923640795));
#47373=CARTESIAN_POINT('Ctrl Pts',(1.93527929945985,1.,3.39499923640795));
#47374=CARTESIAN_POINT('Ctrl Pts',(1.93349233176788,-1.,3.38777076883256));
#47375=CARTESIAN_POINT('Ctrl Pts',(1.93349233176788,1.,3.38777076883256));
#47376=CARTESIAN_POINT('Ctrl Pts',(1.93165739093276,-1.,3.3805676852555));
#47377=CARTESIAN_POINT('Ctrl Pts',(1.93165739093276,1.,3.3805676852555));
#47378=CARTESIAN_POINT('Ctrl Pts',(1.92975993109877,-1.,3.37336807068043));
#47379=CARTESIAN_POINT('Ctrl Pts',(1.92975993109877,1.,3.37336807068043));
#47380=CARTESIAN_POINT('Ctrl Pts',(1.92778626543786,-1.,3.36615168657567));
#47381=CARTESIAN_POINT('Ctrl Pts',(1.92778626543786,1.,3.36615168657567));
#47382=CARTESIAN_POINT('Ctrl Pts',(1.92572846125756,-1.,3.35890824422965));
#47383=CARTESIAN_POINT('Ctrl Pts',(1.92572846125756,1.,3.35890824422965));
#47384=CARTESIAN_POINT('Ctrl Pts',(1.92358838440528,-1.,3.35164424847223));
#47385=CARTESIAN_POINT('Ctrl Pts',(1.92358838440528,1.,3.35164424847223));
#47386=CARTESIAN_POINT('Ctrl Pts',(1.92138450828404,-1.,3.34439448941961));
#47387=CARTESIAN_POINT('Ctrl Pts',(1.92138450828404,1.,3.34439448941961));
#47388=CARTESIAN_POINT('Ctrl Pts',(1.9191460961021,-1.,3.33721230710012));
#47389=CARTESIAN_POINT('Ctrl Pts',(1.9191460961021,1.,3.33721230710012));
#47390=CARTESIAN_POINT('Ctrl Pts',(1.91690081930331,-1.,3.33014884257873));
#47391=CARTESIAN_POINT('Ctrl Pts',(1.91690081930331,1.,3.33014884257873));
#47392=CARTESIAN_POINT('Ctrl Pts',(1.91466343916627,-1.,3.32323403454535));
#47393=CARTESIAN_POINT('Ctrl Pts',(1.91466343916627,1.,3.32323403454535));
#47394=CARTESIAN_POINT('Ctrl Pts',(1.91242616234442,-1.,3.31646052426364));
#47395=CARTESIAN_POINT('Ctrl Pts',(1.91242616234442,1.,3.31646052426364));
#47396=CARTESIAN_POINT('Ctrl Pts',(1.91014297830446,-1.,3.30975721158596));
#47397=CARTESIAN_POINT('Ctrl Pts',(1.91014297830446,1.,3.30975721158596));
#47398=CARTESIAN_POINT('Ctrl Pts',(1.90773912171341,-1.,3.30300595568195));
#47399=CARTESIAN_POINT('Ctrl Pts',(1.90773912171341,1.,3.30300595568195));
#47400=CARTESIAN_POINT('Ctrl Pts',(1.90513891864087,-1.,3.29608978722113));
#47401=CARTESIAN_POINT('Ctrl Pts',(1.90513891864087,1.,3.29608978722113));
#47402=CARTESIAN_POINT('Ctrl Pts',(1.90228971247527,-1.,3.2889344860029));
#47403=CARTESIAN_POINT('Ctrl Pts',(1.90228971247527,1.,3.2889344860029));
#47404=CARTESIAN_POINT('Ctrl Pts',(1.89918429230462,-1.,3.28154737912352));
#47405=CARTESIAN_POINT('Ctrl Pts',(1.89918429230462,1.,3.28154737912352));
#47406=CARTESIAN_POINT('Ctrl Pts',(1.89589172903793,-1.,3.27407108933139));
#47407=CARTESIAN_POINT('Ctrl Pts',(1.89589172903793,1.,3.27407108933139));
#47408=CARTESIAN_POINT('Ctrl Pts',(1.89255393500965,-1.,3.26677653888676));
#47409=CARTESIAN_POINT('Ctrl Pts',(1.89255393500965,1.,3.26677653888676));
#47410=CARTESIAN_POINT('Ctrl Pts',(1.88934996203698,-1.,3.25999885193947));
#47411=CARTESIAN_POINT('Ctrl Pts',(1.88934996203698,1.,3.25999885193947));
#47412=CARTESIAN_POINT('Ctrl Pts',(1.88646802523466,-1.,3.25408686339463));
#47413=CARTESIAN_POINT('Ctrl Pts',(1.88646802523466,1.,3.25408686339463));
#47414=CARTESIAN_POINT('Ctrl Pts',(1.88407708646357,-1.,3.24935200511918));
#47415=CARTESIAN_POINT('Ctrl Pts',(1.88407708646357,1.,3.24935200511918));
#47416=CARTESIAN_POINT('Ctrl Pts',(1.88229202582941,-1.,3.24600543790443));
#47417=CARTESIAN_POINT('Ctrl Pts',(1.88229202582941,1.,3.24600543790443));
#47418=CARTESIAN_POINT('Ctrl Pts',(1.88139187908074,-1.,3.24451807186481));
#47419=CARTESIAN_POINT('Ctrl Pts',(1.88139187908074,1.,3.24451807186481));
#47420=CARTESIAN_POINT('Ctrl Pts',(1.88102201872555,-1.,3.24408699284121));
#47421=CARTESIAN_POINT('Ctrl Pts',(1.88102201872555,1.,3.24408699284121));
#47422=CARTESIAN_POINT('Ctrl Pts',(1.88091100680349,-1.,3.24410359189609));
#47423=CARTESIAN_POINT('Ctrl Pts',(1.88091100680349,1.,3.24410359189609));
#47424=CARTESIAN_POINT('Ctrl Pts',(1.8808893942881,-1.,3.24418789321065));
#47425=CARTESIAN_POINT('Ctrl Pts',(1.8808893942881,1.,3.24418789321065));
#47426=CARTESIAN_POINT('',(1.97421938526992,1.,3.70708211654725));
#47427=CARTESIAN_POINT('Ctrl Pts',(1.97421938526992,1.,3.70708211654725));
#47428=CARTESIAN_POINT('Ctrl Pts',(1.97417727645308,1.,3.70551008132332));
#47429=CARTESIAN_POINT('Ctrl Pts',(1.97408973726715,1.,3.70236698912904));
#47430=CARTESIAN_POINT('Ctrl Pts',(1.97394846383216,1.,3.6976552856004));
#47431=CARTESIAN_POINT('Ctrl Pts',(1.97374016225483,1.,3.69137888599902));
#47432=CARTESIAN_POINT('Ctrl Pts',(1.97344650304519,1.,3.68354319915092));
#47433=CARTESIAN_POINT('Ctrl Pts',(1.97311947678516,1.,3.67571738107084));
#47434=CARTESIAN_POINT('Ctrl Pts',(1.97275897198678,1.,3.66790152752075));
#47435=CARTESIAN_POINT('Ctrl Pts',(1.9723648543905,1.,3.6600957816636));
#47436=CARTESIAN_POINT('Ctrl Pts',(1.97193697240239,1.,3.652300347166));
#47437=CARTESIAN_POINT('Ctrl Pts',(1.97147515441164,1.,3.64451546723514));
#47438=CARTESIAN_POINT('Ctrl Pts',(1.97097920454464,1.,3.63674139590412));
#47439=CARTESIAN_POINT('Ctrl Pts',(1.97044889850463,1.,3.62897836973293));
#47440=CARTESIAN_POINT('Ctrl Pts',(1.96988398129978,1.,3.62122658401893));
#47441=CARTESIAN_POINT('Ctrl Pts',(1.96928416040877,1.,3.61348615496704));
#47442=CARTESIAN_POINT('Ctrl Pts',(1.9686491188594,1.,3.60575714017989));
#47443=CARTESIAN_POINT('Ctrl Pts',(1.96797854118369,1.,3.59803959819938));
#47444=CARTESIAN_POINT('Ctrl Pts',(1.96727213799544,1.,3.59033364022801));
#47445=CARTESIAN_POINT('Ctrl Pts',(1.96652966688911,1.,3.58263947663829));
#47446=CARTESIAN_POINT('Ctrl Pts',(1.96575096652789,1.,3.57495748600959));
#47447=CARTESIAN_POINT('Ctrl Pts',(1.96493594634567,1.,3.56728820357791));
#47448=CARTESIAN_POINT('Ctrl Pts',(1.96408450906812,1.,3.55963218706096));
#47449=CARTESIAN_POINT('Ctrl Pts',(1.96319648628644,1.,3.55198990600886));
#47450=CARTESIAN_POINT('Ctrl Pts',(1.96227157573067,1.,3.54436163300443));
#47451=CARTESIAN_POINT('Ctrl Pts',(1.96130926212689,1.,3.53674730625813));
#47452=CARTESIAN_POINT('Ctrl Pts',(1.96030879411566,1.,3.52914648844351));
#47453=CARTESIAN_POINT('Ctrl Pts',(1.95926936324461,1.,3.52155867431486));
#47454=CARTESIAN_POINT('Ctrl Pts',(1.95819025316779,1.,3.51398354617794));
#47455=CARTESIAN_POINT('Ctrl Pts',(1.95707099606511,1.,3.50642124159909));
#47456=CARTESIAN_POINT('Ctrl Pts',(1.95591153823661,1.,3.49887263575583));
#47457=CARTESIAN_POINT('Ctrl Pts',(1.95471236969643,1.,3.49133956289133));
#47458=CARTESIAN_POINT('Ctrl Pts',(1.95347412486308,1.,3.48382414832634));
#47459=CARTESIAN_POINT('Ctrl Pts',(1.95219722189876,1.,3.47632820495921));
#47460=CARTESIAN_POINT('Ctrl Pts',(1.95088147859876,1.,3.46885258974191));
#47461=CARTESIAN_POINT('Ctrl Pts',(1.94952575850197,1.,3.46139661060962));
#47462=CARTESIAN_POINT('Ctrl Pts',(1.94812754766524,1.,3.45395731584051));
#47463=CARTESIAN_POINT('Ctrl Pts',(1.94668377715329,1.,3.44653088665681));
#47464=CARTESIAN_POINT('Ctrl Pts',(1.94519168842879,1.,3.43911410197687));
#47465=CARTESIAN_POINT('Ctrl Pts',(1.94364973660284,1.,3.43170586602434));
#47466=CARTESIAN_POINT('Ctrl Pts',(1.94205835913696,1.,3.42430850941503));
#47467=CARTESIAN_POINT('Ctrl Pts',(1.94042111965246,1.,3.41692971994096));
#47468=CARTESIAN_POINT('Ctrl Pts',(1.93874306008143,1.,3.40957978266642));
#47469=CARTESIAN_POINT('Ctrl Pts',(1.93702857723098,1.,3.40226802104109));
#47470=CARTESIAN_POINT('Ctrl Pts',(1.93527929945985,1.,3.39499923640795));
#47471=CARTESIAN_POINT('Ctrl Pts',(1.93349233176788,1.,3.38777076883256));
#47472=CARTESIAN_POINT('Ctrl Pts',(1.93165739093276,1.,3.3805676852555));
#47473=CARTESIAN_POINT('Ctrl Pts',(1.92975993109877,1.,3.37336807068043));
#47474=CARTESIAN_POINT('Ctrl Pts',(1.92778626543786,1.,3.36615168657567));
#47475=CARTESIAN_POINT('Ctrl Pts',(1.92572846125756,1.,3.35890824422965));
#47476=CARTESIAN_POINT('Ctrl Pts',(1.92358838440528,1.,3.35164424847223));
#47477=CARTESIAN_POINT('Ctrl Pts',(1.92138450828404,1.,3.34439448941961));
#47478=CARTESIAN_POINT('Ctrl Pts',(1.9191460961021,1.,3.33721230710012));
#47479=CARTESIAN_POINT('Ctrl Pts',(1.91690081930331,1.,3.33014884257873));
#47480=CARTESIAN_POINT('Ctrl Pts',(1.91466343916627,1.,3.32323403454535));
#47481=CARTESIAN_POINT('Ctrl Pts',(1.91242616234442,1.,3.31646052426364));
#47482=CARTESIAN_POINT('Ctrl Pts',(1.91014297830446,1.,3.30975721158596));
#47483=CARTESIAN_POINT('Ctrl Pts',(1.90773912171341,1.,3.30300595568195));
#47484=CARTESIAN_POINT('Ctrl Pts',(1.90513891864087,1.,3.29608978722113));
#47485=CARTESIAN_POINT('Ctrl Pts',(1.90228971247527,1.,3.2889344860029));
#47486=CARTESIAN_POINT('Ctrl Pts',(1.89918429230462,1.,3.28154737912352));
#47487=CARTESIAN_POINT('Ctrl Pts',(1.89589172903793,1.,3.27407108933139));
#47488=CARTESIAN_POINT('Ctrl Pts',(1.89255393500965,1.,3.26677653888676));
#47489=CARTESIAN_POINT('Ctrl Pts',(1.88934996203698,1.,3.25999885193947));
#47490=CARTESIAN_POINT('Ctrl Pts',(1.88646802523466,1.,3.25408686339463));
#47491=CARTESIAN_POINT('Ctrl Pts',(1.88407708646357,1.,3.24935200511918));
#47492=CARTESIAN_POINT('Ctrl Pts',(1.88242596600454,1.,3.2462565441079));
#47493=CARTESIAN_POINT('Ctrl Pts',(1.88156537699203,1.,3.24480754676064));
#47494=CARTESIAN_POINT('Ctrl Pts',(1.88117508446775,1.,3.24428080353022));
#47495=CARTESIAN_POINT('Ctrl Pts',(1.8810229239812,1.,3.24415531671284));
#47496=CARTESIAN_POINT('Ctrl Pts',(1.88097764062697,1.,3.24413672884812));
#47497=CARTESIAN_POINT('',(1.97421938526992,0.,3.70708211654725));
#47498=CARTESIAN_POINT('Ctrl Pts',(1.519044091397,-1.,3.42855728381368));
#47499=CARTESIAN_POINT('Ctrl Pts',(1.519044091397,1.,3.42855728381368));
#47500=CARTESIAN_POINT('Ctrl Pts',(1.51896318668366,-1.,3.42852521763778));
#47501=CARTESIAN_POINT('Ctrl Pts',(1.51896318668366,1.,3.42852521763778));
#47502=CARTESIAN_POINT('Ctrl Pts',(1.51888450659652,-1.,3.42860527149177));
#47503=CARTESIAN_POINT('Ctrl Pts',(1.51888450659652,1.,3.42860527149177));
#47504=CARTESIAN_POINT('Ctrl Pts',(1.51901585839109,-1.,3.42915787669893));
#47505=CARTESIAN_POINT('Ctrl Pts',(1.51901585839109,1.,3.42915787669893));
#47506=CARTESIAN_POINT('Ctrl Pts',(1.51969006980999,-1.,3.43076036253837));
#47507=CARTESIAN_POINT('Ctrl Pts',(1.51969006980999,1.,3.43076036253837));
#47508=CARTESIAN_POINT('Ctrl Pts',(1.52134826724292,-1.,3.43417156977893));
#47509=CARTESIAN_POINT('Ctrl Pts',(1.52134826724292,1.,3.43417156977893));
#47510=CARTESIAN_POINT('Ctrl Pts',(1.5237734895035,-1.,3.4388889597401));
#47511=CARTESIAN_POINT('Ctrl Pts',(1.5237734895035,1.,3.4388889597401));
#47512=CARTESIAN_POINT('Ctrl Pts',(1.52686242875556,-1.,3.44469547526647));
#47513=CARTESIAN_POINT('Ctrl Pts',(1.52686242875556,1.,3.44469547526647));
#47514=CARTESIAN_POINT('Ctrl Pts',(1.53046244461635,-1.,3.45127136828305));
#47515=CARTESIAN_POINT('Ctrl Pts',(1.53046244461635,1.,3.45127136828305));
#47516=CARTESIAN_POINT('Ctrl Pts',(1.53440195378792,-1.,3.45825932955032));
#47517=CARTESIAN_POINT('Ctrl Pts',(1.53440195378792,1.,3.45825932955032));
#47518=CARTESIAN_POINT('Ctrl Pts',(1.53851507915502,-1.,3.46531752207153));
#47519=CARTESIAN_POINT('Ctrl Pts',(1.53851507915502,1.,3.46531752207153));
#47520=CARTESIAN_POINT('Ctrl Pts',(1.54266605398187,-1.,3.47217189224653));
#47521=CARTESIAN_POINT('Ctrl Pts',(1.54266605398187,1.,3.47217189224653));
#47522=CARTESIAN_POINT('Ctrl Pts',(1.54678009290276,-1.,3.47868272898751));
#47523=CARTESIAN_POINT('Ctrl Pts',(1.54678009290276,1.,3.47868272898751));
#47524=CARTESIAN_POINT('Ctrl Pts',(1.55084702970452,-1.,3.48485155928567));
#47525=CARTESIAN_POINT('Ctrl Pts',(1.55084702970452,1.,3.48485155928567));
#47526=CARTESIAN_POINT('Ctrl Pts',(1.55489595901116,-1.,3.4907646087742));
#47527=CARTESIAN_POINT('Ctrl Pts',(1.55489595901116,1.,3.4907646087742));
#47528=CARTESIAN_POINT('Ctrl Pts',(1.55897703097874,-1.,3.49655185179655));
#47529=CARTESIAN_POINT('Ctrl Pts',(1.55897703097874,1.,3.49655185179655));
#47530=CARTESIAN_POINT('Ctrl Pts',(1.56314187758675,-1.,3.50234321621578));
#47531=CARTESIAN_POINT('Ctrl Pts',(1.56314187758675,1.,3.50234321621578));
#47532=CARTESIAN_POINT('Ctrl Pts',(1.56742097575012,-1.,3.50821771695363));
#47533=CARTESIAN_POINT('Ctrl Pts',(1.56742097575012,1.,3.50821771695363));
#47534=CARTESIAN_POINT('Ctrl Pts',(1.57181569799743,-1.,3.51418598431665));
#47535=CARTESIAN_POINT('Ctrl Pts',(1.57181569799743,1.,3.51418598431665));
#47536=CARTESIAN_POINT('Ctrl Pts',(1.57631049988158,-1.,3.52021847865912));
#47537=CARTESIAN_POINT('Ctrl Pts',(1.57631049988158,1.,3.52021847865912));
#47538=CARTESIAN_POINT('Ctrl Pts',(1.58088027227848,-1.,3.52626275334881));
#47539=CARTESIAN_POINT('Ctrl Pts',(1.58088027227848,1.,3.52626275334881));
#47540=CARTESIAN_POINT('Ctrl Pts',(1.58549906268088,-1.,3.5322637814708));
#47541=CARTESIAN_POINT('Ctrl Pts',(1.58549906268088,1.,3.5322637814708));
#47542=CARTESIAN_POINT('Ctrl Pts',(1.59014958368739,-1.,3.53818616861077));
#47543=CARTESIAN_POINT('Ctrl Pts',(1.59014958368739,1.,3.53818616861077));
#47544=CARTESIAN_POINT('Ctrl Pts',(1.59482766949766,-1.,3.54402458182337));
#47545=CARTESIAN_POINT('Ctrl Pts',(1.59482766949766,1.,3.54402458182337));
#47546=CARTESIAN_POINT('Ctrl Pts',(1.59953698113457,-1.,3.54979148634454));
#47547=CARTESIAN_POINT('Ctrl Pts',(1.59953698113457,1.,3.54979148634454));
#47548=CARTESIAN_POINT('Ctrl Pts',(1.60428584699853,-1.,3.55550985096129));
#47549=CARTESIAN_POINT('Ctrl Pts',(1.60428584699853,1.,3.55550985096129));
#47550=CARTESIAN_POINT('Ctrl Pts',(1.60908344685457,-1.,3.5612043248298));
#47551=CARTESIAN_POINT('Ctrl Pts',(1.60908344685457,1.,3.5612043248298));
#47552=CARTESIAN_POINT('Ctrl Pts',(1.61393581747514,-1.,3.56689200468387));
#47553=CARTESIAN_POINT('Ctrl Pts',(1.61393581747514,1.,3.56689200468387));
#47554=CARTESIAN_POINT('Ctrl Pts',(1.61884340915404,-1.,3.57257679609806));
#47555=CARTESIAN_POINT('Ctrl Pts',(1.61884340915404,1.,3.57257679609806));
#47556=CARTESIAN_POINT('Ctrl Pts',(1.62380329464844,-1.,3.5782545595439));
#47557=CARTESIAN_POINT('Ctrl Pts',(1.62380329464844,1.,3.5782545595439));
#47558=CARTESIAN_POINT('Ctrl Pts',(1.62881051550745,-1.,3.58391625774343));
#47559=CARTESIAN_POINT('Ctrl Pts',(1.62881051550745,1.,3.58391625774343));
#47560=CARTESIAN_POINT('Ctrl Pts',(1.6338597145126,-1.,3.58955176627879));
#47561=CARTESIAN_POINT('Ctrl Pts',(1.6338597145126,1.,3.58955176627879));
#47562=CARTESIAN_POINT('Ctrl Pts',(1.63894676675352,-1.,3.59515368334893));
#47563=CARTESIAN_POINT('Ctrl Pts',(1.63894676675352,1.,3.59515368334893));
#47564=CARTESIAN_POINT('Ctrl Pts',(1.64407004385582,-1.,3.60072028513845));
#47565=CARTESIAN_POINT('Ctrl Pts',(1.64407004385582,1.,3.60072028513845));
#47566=CARTESIAN_POINT('Ctrl Pts',(1.64922952425832,-1.,3.60625346556992));
#47567=CARTESIAN_POINT('Ctrl Pts',(1.64922952425832,1.,3.60625346556992));
#47568=CARTESIAN_POINT('Ctrl Pts',(1.65442619244325,-1.,3.61175734965127));
#47569=CARTESIAN_POINT('Ctrl Pts',(1.65442619244325,1.,3.61175734965127));
#47570=CARTESIAN_POINT('Ctrl Pts',(1.65966133399186,-1.,3.61723666482456));
#47571=CARTESIAN_POINT('Ctrl Pts',(1.65966133399186,1.,3.61723666482456));
#47572=CARTESIAN_POINT('Ctrl Pts',(1.66493585923855,-1.,3.62269517989109));
#47573=CARTESIAN_POINT('Ctrl Pts',(1.66493585923855,1.,3.62269517989109));
#47574=CARTESIAN_POINT('Ctrl Pts',(1.67024966008044,-1.,3.62813422105271));
#47575=CARTESIAN_POINT('Ctrl Pts',(1.67024966008044,1.,3.62813422105271));
#47576=CARTESIAN_POINT('Ctrl Pts',(1.67560193613156,-1.,3.63355343201232));
#47577=CARTESIAN_POINT('Ctrl Pts',(1.67560193613156,1.,3.63355343201232));
#47578=CARTESIAN_POINT('Ctrl Pts',(1.68099146651586,-1.,3.63895140887462));
#47579=CARTESIAN_POINT('Ctrl Pts',(1.68099146651586,1.,3.63895140887462));
#47580=CARTESIAN_POINT('Ctrl Pts',(1.68641690471457,-1.,3.64432638915203));
#47581=CARTESIAN_POINT('Ctrl Pts',(1.68641690471457,1.,3.64432638915203));
#47582=CARTESIAN_POINT('Ctrl Pts',(1.69187705481689,-1.,3.64967689827371));
#47583=CARTESIAN_POINT('Ctrl Pts',(1.69187705481689,1.,3.64967689827371));
#47584=CARTESIAN_POINT('Ctrl Pts',(1.69737117722534,-1.,3.65500246526749));
#47585=CARTESIAN_POINT('Ctrl Pts',(1.69737117722534,1.,3.65500246526749));
#47586=CARTESIAN_POINT('Ctrl Pts',(1.70289888566873,-1.,3.66030338774847));
#47587=CARTESIAN_POINT('Ctrl Pts',(1.70289888566873,1.,3.66030338774847));
#47588=CARTESIAN_POINT('Ctrl Pts',(1.70846001610956,-1.,3.66558043198876));
#47589=CARTESIAN_POINT('Ctrl Pts',(1.70846001610956,1.,3.66558043198876));
#47590=CARTESIAN_POINT('Ctrl Pts',(1.71405450210383,-1.,3.67083454901611));
#47591=CARTESIAN_POINT('Ctrl Pts',(1.71405450210383,1.,3.67083454901611));
#47592=CARTESIAN_POINT('Ctrl Pts',(1.71968225581808,-1.,3.67606660374709));
#47593=CARTESIAN_POINT('Ctrl Pts',(1.71968225581808,1.,3.67606660374709));
#47594=CARTESIAN_POINT('Ctrl Pts',(1.72534302437056,-1.,3.68127704936579));
#47595=CARTESIAN_POINT('Ctrl Pts',(1.72534302437056,1.,3.68127704936579));
#47596=CARTESIAN_POINT('Ctrl Pts',(1.73103640956717,-1.,3.68646597019332));
#47597=CARTESIAN_POINT('Ctrl Pts',(1.73103640956717,1.,3.68646597019332));
#47598=CARTESIAN_POINT('Ctrl Pts',(1.73676193254557,-1.,3.69163322648036));
#47599=CARTESIAN_POINT('Ctrl Pts',(1.73676193254557,1.,3.69163322648036));
#47600=CARTESIAN_POINT('Ctrl Pts',(1.74251908492617,-1.,3.69677856910517));
#47601=CARTESIAN_POINT('Ctrl Pts',(1.74251908492617,1.,3.69677856910517));
#47602=CARTESIAN_POINT('Ctrl Pts',(1.74830738046057,-1.,3.7019017567335));
#47603=CARTESIAN_POINT('Ctrl Pts',(1.74830738046057,1.,3.7019017567335));
#47604=CARTESIAN_POINT('Ctrl Pts',(1.75412641804042,-1.,3.70700269736659));
#47605=CARTESIAN_POINT('Ctrl Pts',(1.75412641804042,1.,3.70700269736659));
#47606=CARTESIAN_POINT('Ctrl Pts',(1.75997588498865,-1.,3.71208146346136));
#47607=CARTESIAN_POINT('Ctrl Pts',(1.75997588498865,1.,3.71208146346136));
#47608=CARTESIAN_POINT('Ctrl Pts',(1.76585552124394,-1.,3.71713822377359));
#47609=CARTESIAN_POINT('Ctrl Pts',(1.76585552124394,1.,3.71713822377359));
#47610=CARTESIAN_POINT('Ctrl Pts',(1.77176509401761,-1.,3.72217319911254));
#47611=CARTESIAN_POINT('Ctrl Pts',(1.77176509401761,1.,3.72217319911254));
#47612=CARTESIAN_POINT('Ctrl Pts',(1.77770437039658,-1.,3.72718661205609));
#47613=CARTESIAN_POINT('Ctrl Pts',(1.77770437039658,1.,3.72718661205609));
#47614=CARTESIAN_POINT('Ctrl Pts',(1.78367308442901,-1.,3.7321786309547));
#47615=CARTESIAN_POINT('Ctrl Pts',(1.78367308442901,1.,3.7321786309547));
#47616=CARTESIAN_POINT('Ctrl Pts',(1.78967092823491,-1.,3.73714934730681));
#47617=CARTESIAN_POINT('Ctrl Pts',(1.78967092823491,1.,3.73714934730681));
#47618=CARTESIAN_POINT('Ctrl Pts',(1.79569757859422,-1.,3.74209880352445));
#47619=CARTESIAN_POINT('Ctrl Pts',(1.79569757859422,1.,3.74209880352445));
#47620=CARTESIAN_POINT('Ctrl Pts',(1.8017527148577,-1.,3.74702700875467));
#47621=CARTESIAN_POINT('Ctrl Pts',(1.8017527148577,1.,3.74702700875467));
#47622=CARTESIAN_POINT('Ctrl Pts',(1.80783603939617,-1.,3.75193395887977));
#47623=CARTESIAN_POINT('Ctrl Pts',(1.80783603939617,1.,3.75193395887977));
#47624=CARTESIAN_POINT('Ctrl Pts',(1.8139472983358,-1.,3.75681965683071));
#47625=CARTESIAN_POINT('Ctrl Pts',(1.8139472983358,1.,3.75681965683071));
#47626=CARTESIAN_POINT('Ctrl Pts',(1.82008629694091,-1.,3.76168412707948));
#47627=CARTESIAN_POINT('Ctrl Pts',(1.82008629694091,1.,3.76168412707948));
#47628=CARTESIAN_POINT('Ctrl Pts',(1.82625289220915,-1.,3.76652740353775));
#47629=CARTESIAN_POINT('Ctrl Pts',(1.82625289220915,1.,3.76652740353775));
#47630=CARTESIAN_POINT('Ctrl Pts',(1.83120816955645,-1.,3.77038509817999));
#47631=CARTESIAN_POINT('Ctrl Pts',(1.83120816955645,1.,3.77038509817999));
#47632=CARTESIAN_POINT('Ctrl Pts',(1.83493697934534,-1.,3.77326886064398));
#47633=CARTESIAN_POINT('Ctrl Pts',(1.83493697934534,1.,3.77326886064398));
#47634=CARTESIAN_POINT('Ctrl Pts',(1.83742834010626,-1.,3.77518714457833));
#47635=CARTESIAN_POINT('Ctrl Pts',(1.83742834010626,1.,3.77518714457833));
#47636=CARTESIAN_POINT('Ctrl Pts',(1.8386753923786,-1.,3.77614523045147));
#47637=CARTESIAN_POINT('Ctrl Pts',(1.8386753923786,1.,3.77614523045147));
#47638=CARTESIAN_POINT('',(1.5189508286633,1.,3.42859860294306));
#47639=CARTESIAN_POINT('Ctrl Pts',(1.5189508286633,-1.,3.42859860294306));
#47640=CARTESIAN_POINT('Ctrl Pts',(1.5189508286633,-0.666666666666667,3.42859860294306));
#47641=CARTESIAN_POINT('Ctrl Pts',(1.5189508286633,-0.333333333333333,3.42859860294306));
#47642=CARTESIAN_POINT('Ctrl Pts',(1.5189508286633,0.333333333333333,3.42859860294306));
#47643=CARTESIAN_POINT('Ctrl Pts',(1.5189508286633,0.666666666666667,3.42859860294306));
#47644=CARTESIAN_POINT('Ctrl Pts',(1.5189508286633,1.,3.42859860294306));
#47645=CARTESIAN_POINT('',(1.8386753923786,1.,3.77614523045147));
#47646=CARTESIAN_POINT('',(1.8386753923786,0.,3.77614523045147));
#47647=CARTESIAN_POINT('Ctrl Pts',(1.5189508286633,1.,3.42859860294306));
#47648=CARTESIAN_POINT('Ctrl Pts',(1.51893924967331,1.,3.42864616361875));
#47649=CARTESIAN_POINT('Ctrl Pts',(1.5189513329503,1.,3.42884302333841));
#47650=CARTESIAN_POINT('Ctrl Pts',(1.51914806898491,1.,3.42946838852587));
#47651=CARTESIAN_POINT('Ctrl Pts',(1.5198144909338,1.,3.43101631893414));
#47652=CARTESIAN_POINT('Ctrl Pts',(1.52134826724292,1.,3.43417156977893));
#47653=CARTESIAN_POINT('Ctrl Pts',(1.5237734895035,1.,3.4388889597401));
#47654=CARTESIAN_POINT('Ctrl Pts',(1.52686242875556,1.,3.44469547526647));
#47655=CARTESIAN_POINT('Ctrl Pts',(1.53046244461635,1.,3.45127136828305));
#47656=CARTESIAN_POINT('Ctrl Pts',(1.53440195378792,1.,3.45825932955032));
#47657=CARTESIAN_POINT('Ctrl Pts',(1.53851507915502,1.,3.46531752207153));
#47658=CARTESIAN_POINT('Ctrl Pts',(1.54266605398187,1.,3.47217189224653));
#47659=CARTESIAN_POINT('Ctrl Pts',(1.54678009290276,1.,3.47868272898751));
#47660=CARTESIAN_POINT('Ctrl Pts',(1.55084702970452,1.,3.48485155928567));
#47661=CARTESIAN_POINT('Ctrl Pts',(1.55489595901116,1.,3.4907646087742));
#47662=CARTESIAN_POINT('Ctrl Pts',(1.55897703097874,1.,3.49655185179655));
#47663=CARTESIAN_POINT('Ctrl Pts',(1.56314187758675,1.,3.50234321621578));
#47664=CARTESIAN_POINT('Ctrl Pts',(1.56742097575012,1.,3.50821771695363));
#47665=CARTESIAN_POINT('Ctrl Pts',(1.57181569799743,1.,3.51418598431665));
#47666=CARTESIAN_POINT('Ctrl Pts',(1.57631049988158,1.,3.52021847865912));
#47667=CARTESIAN_POINT('Ctrl Pts',(1.58088027227848,1.,3.52626275334881));
#47668=CARTESIAN_POINT('Ctrl Pts',(1.58549906268088,1.,3.5322637814708));
#47669=CARTESIAN_POINT('Ctrl Pts',(1.59014958368739,1.,3.53818616861077));
#47670=CARTESIAN_POINT('Ctrl Pts',(1.59482766949766,1.,3.54402458182337));
#47671=CARTESIAN_POINT('Ctrl Pts',(1.59953698113457,1.,3.54979148634454));
#47672=CARTESIAN_POINT('Ctrl Pts',(1.60428584699853,1.,3.55550985096129));
#47673=CARTESIAN_POINT('Ctrl Pts',(1.60908344685457,1.,3.5612043248298));
#47674=CARTESIAN_POINT('Ctrl Pts',(1.61393581747514,1.,3.56689200468387));
#47675=CARTESIAN_POINT('Ctrl Pts',(1.61884340915404,1.,3.57257679609806));
#47676=CARTESIAN_POINT('Ctrl Pts',(1.62380329464844,1.,3.5782545595439));
#47677=CARTESIAN_POINT('Ctrl Pts',(1.62881051550745,1.,3.58391625774343));
#47678=CARTESIAN_POINT('Ctrl Pts',(1.6338597145126,1.,3.58955176627879));
#47679=CARTESIAN_POINT('Ctrl Pts',(1.63894676675352,1.,3.59515368334893));
#47680=CARTESIAN_POINT('Ctrl Pts',(1.64407004385582,1.,3.60072028513845));
#47681=CARTESIAN_POINT('Ctrl Pts',(1.64922952425832,1.,3.60625346556992));
#47682=CARTESIAN_POINT('Ctrl Pts',(1.65442619244325,1.,3.61175734965127));
#47683=CARTESIAN_POINT('Ctrl Pts',(1.65966133399186,1.,3.61723666482456));
#47684=CARTESIAN_POINT('Ctrl Pts',(1.66493585923855,1.,3.62269517989109));
#47685=CARTESIAN_POINT('Ctrl Pts',(1.67024966008044,1.,3.62813422105271));
#47686=CARTESIAN_POINT('Ctrl Pts',(1.67560193613156,1.,3.63355343201232));
#47687=CARTESIAN_POINT('Ctrl Pts',(1.68099146651586,1.,3.63895140887462));
#47688=CARTESIAN_POINT('Ctrl Pts',(1.68641690471457,1.,3.64432638915203));
#47689=CARTESIAN_POINT('Ctrl Pts',(1.69187705481689,1.,3.64967689827371));
#47690=CARTESIAN_POINT('Ctrl Pts',(1.69737117722534,1.,3.65500246526749));
#47691=CARTESIAN_POINT('Ctrl Pts',(1.70289888566873,1.,3.66030338774847));
#47692=CARTESIAN_POINT('Ctrl Pts',(1.70846001610956,1.,3.66558043198876));
#47693=CARTESIAN_POINT('Ctrl Pts',(1.71405450210383,1.,3.67083454901611));
#47694=CARTESIAN_POINT('Ctrl Pts',(1.71968225581808,1.,3.67606660374709));
#47695=CARTESIAN_POINT('Ctrl Pts',(1.72534302437056,1.,3.68127704936579));
#47696=CARTESIAN_POINT('Ctrl Pts',(1.73103640956717,1.,3.68646597019332));
#47697=CARTESIAN_POINT('Ctrl Pts',(1.73676193254557,1.,3.69163322648036));
#47698=CARTESIAN_POINT('Ctrl Pts',(1.74251908492617,1.,3.69677856910517));
#47699=CARTESIAN_POINT('Ctrl Pts',(1.74830738046057,1.,3.7019017567335));
#47700=CARTESIAN_POINT('Ctrl Pts',(1.75412641804042,1.,3.70700269736659));
#47701=CARTESIAN_POINT('Ctrl Pts',(1.75997588498865,1.,3.71208146346136));
#47702=CARTESIAN_POINT('Ctrl Pts',(1.76585552124394,1.,3.71713822377359));
#47703=CARTESIAN_POINT('Ctrl Pts',(1.77176509401761,1.,3.72217319911254));
#47704=CARTESIAN_POINT('Ctrl Pts',(1.77770437039658,1.,3.72718661205609));
#47705=CARTESIAN_POINT('Ctrl Pts',(1.78367308442901,1.,3.7321786309547));
#47706=CARTESIAN_POINT('Ctrl Pts',(1.78967092823491,1.,3.73714934730681));
#47707=CARTESIAN_POINT('Ctrl Pts',(1.79569757859422,1.,3.74209880352445));
#47708=CARTESIAN_POINT('Ctrl Pts',(1.8017527148577,1.,3.74702700875467));
#47709=CARTESIAN_POINT('Ctrl Pts',(1.80783603939617,1.,3.75193395887977));
#47710=CARTESIAN_POINT('Ctrl Pts',(1.8139472983358,1.,3.75681965683071));
#47711=CARTESIAN_POINT('Ctrl Pts',(1.82008629694091,1.,3.76168412707948));
#47712=CARTESIAN_POINT('Ctrl Pts',(1.82625289220915,1.,3.76652740353775));
#47713=CARTESIAN_POINT('Ctrl Pts',(1.83120816955645,1.,3.77038509817999));
#47714=CARTESIAN_POINT('Ctrl Pts',(1.83493697934534,1.,3.77326886064398));
#47715=CARTESIAN_POINT('Ctrl Pts',(1.83742834010626,1.,3.77518714457833));
#47716=CARTESIAN_POINT('Ctrl Pts',(1.8386753923786,1.,3.77614523045147));
#47717=CARTESIAN_POINT('Origin',(1.8386753923786,0.,3.77614523045147));
#47718=CARTESIAN_POINT('',(1.97421938526992,1.,3.70708211654725));
#47719=CARTESIAN_POINT('Origin',(0.,0.,0.));
#47720=CARTESIAN_POINT('',(1.35032489087269,1.,3.49844575334386));
#47721=CARTESIAN_POINT('Origin',(0.,1.,0.));
#47722=CARTESIAN_POINT('Ctrl Pts',(1.35032489087269,1.,3.49844575334386));
#47723=CARTESIAN_POINT('Ctrl Pts',(1.35032489087269,0.666666666666667,3.49844575334386));
#47724=CARTESIAN_POINT('Ctrl Pts',(1.35032489087269,0.333333333333333,3.49844575334386));
#47725=CARTESIAN_POINT('Ctrl Pts',(1.35032489087269,-0.333333333333333,
3.49844575334386));
#47726=CARTESIAN_POINT('Ctrl Pts',(1.35032489087269,-0.666666666666667,
3.49844575334386));
#47727=CARTESIAN_POINT('Ctrl Pts',(1.35032489087269,-1.,3.49844575334386));
#47728=CARTESIAN_POINT('Ctrl Pts',(1.36999806084572,-1.,3.97027773754922));
#47729=CARTESIAN_POINT('Ctrl Pts',(1.36999806084572,1.,3.97027773754922));
#47730=CARTESIAN_POINT('Ctrl Pts',(1.37020239094758,-1.,3.9687184694173));
#47731=CARTESIAN_POINT('Ctrl Pts',(1.37020239094758,1.,3.9687184694173));
#47732=CARTESIAN_POINT('Ctrl Pts',(1.37060761746027,-1.,3.96560037975788));
#47733=CARTESIAN_POINT('Ctrl Pts',(1.37060761746027,1.,3.96560037975788));
#47734=CARTESIAN_POINT('Ctrl Pts',(1.37120515615663,-1.,3.96092458508407));
#47735=CARTESIAN_POINT('Ctrl Pts',(1.37120515615663,1.,3.96092458508407));
#47736=CARTESIAN_POINT('Ctrl Pts',(1.37198126433139,-1.,3.95469287283105));
#47737=CARTESIAN_POINT('Ctrl Pts',(1.37198126433139,1.,3.95469287283105));
#47738=CARTESIAN_POINT('Ctrl Pts',(1.37291699203423,-1.,3.94690771786926));
#47739=CARTESIAN_POINT('Ctrl Pts',(1.37291699203423,1.,3.94690771786926));
#47740=CARTESIAN_POINT('Ctrl Pts',(1.37381821967499,-1.,3.93912709041791));
#47741=CARTESIAN_POINT('Ctrl Pts',(1.37381821967499,1.,3.93912709041791));
#47742=CARTESIAN_POINT('Ctrl Pts',(1.37468482215784,-1.,3.93135106761941));
#47743=CARTESIAN_POINT('Ctrl Pts',(1.37468482215784,1.,3.93135106761941));
#47744=CARTESIAN_POINT('Ctrl Pts',(1.37551664448057,-1.,3.92357976987132));
#47745=CARTESIAN_POINT('Ctrl Pts',(1.37551664448057,1.,3.92357976987132));
#47746=CARTESIAN_POINT('Ctrl Pts',(1.37631350505516,-1.,3.91581337461825));
#47747=CARTESIAN_POINT('Ctrl Pts',(1.37631350505516,1.,3.91581337461825));
#47748=CARTESIAN_POINT('Ctrl Pts',(1.3770751963376,-1.,3.90805209522729));
#47749=CARTESIAN_POINT('Ctrl Pts',(1.3770751963376,1.,3.90805209522729));
#47750=CARTESIAN_POINT('Ctrl Pts',(1.3778014851263,-1.,3.90029615196255));
#47751=CARTESIAN_POINT('Ctrl Pts',(1.3778014851263,1.,3.90029615196255));
#47752=CARTESIAN_POINT('Ctrl Pts',(1.37849211287981,-1.,3.89254574338385));
#47753=CARTESIAN_POINT('Ctrl Pts',(1.37849211287981,1.,3.89254574338385));
#47754=CARTESIAN_POINT('Ctrl Pts',(1.37914679719446,-1.,3.88480102249461));
#47755=CARTESIAN_POINT('Ctrl Pts',(1.37914679719446,1.,3.88480102249461));
#47756=CARTESIAN_POINT('Ctrl Pts',(1.37976523097187,-1.,3.87706205830865));
#47757=CARTESIAN_POINT('Ctrl Pts',(1.37976523097187,1.,3.87706205830865));
#47758=CARTESIAN_POINT('Ctrl Pts',(1.38034709213129,-1.,3.86932885813403));
#47759=CARTESIAN_POINT('Ctrl Pts',(1.38034709213129,1.,3.86932885813403));
#47760=CARTESIAN_POINT('Ctrl Pts',(1.38089205993067,-1.,3.86160143044187));
#47761=CARTESIAN_POINT('Ctrl Pts',(1.38089205993067,1.,3.86160143044187));
#47762=CARTESIAN_POINT('Ctrl Pts',(1.38139983115075,-1.,3.85387983979557));
#47763=CARTESIAN_POINT('Ctrl Pts',(1.38139983115075,1.,3.85387983979557));
#47764=CARTESIAN_POINT('Ctrl Pts',(1.38187013346089,-1.,3.84616425605705));
#47765=CARTESIAN_POINT('Ctrl Pts',(1.38187013346089,1.,3.84616425605705));
#47766=CARTESIAN_POINT('Ctrl Pts',(1.38230274828774,-1.,3.83845502790609));
#47767=CARTESIAN_POINT('Ctrl Pts',(1.38230274828774,1.,3.83845502790609));
#47768=CARTESIAN_POINT('Ctrl Pts',(1.38269750245086,-1.,3.83075266982138));
#47769=CARTESIAN_POINT('Ctrl Pts',(1.38269750245086,1.,3.83075266982138));
#47770=CARTESIAN_POINT('Ctrl Pts',(1.38305421262724,-1.,3.82305771743715));
#47771=CARTESIAN_POINT('Ctrl Pts',(1.38305421262724,1.,3.82305771743715));
#47772=CARTESIAN_POINT('Ctrl Pts',(1.38337263902766,-1.,3.81537060817765));
#47773=CARTESIAN_POINT('Ctrl Pts',(1.38337263902766,1.,3.81537060817765));
#47774=CARTESIAN_POINT('Ctrl Pts',(1.38365244046226,-1.,3.80769156398429));
#47775=CARTESIAN_POINT('Ctrl Pts',(1.38365244046226,1.,3.80769156398429));
#47776=CARTESIAN_POINT('Ctrl Pts',(1.38389311766701,-1.,3.80002044322169));
#47777=CARTESIAN_POINT('Ctrl Pts',(1.38389311766701,1.,3.80002044322169));
#47778=CARTESIAN_POINT('Ctrl Pts',(1.38409399694588,-1.,3.79235669640907));
#47779=CARTESIAN_POINT('Ctrl Pts',(1.38409399694588,1.,3.79235669640907));
#47780=CARTESIAN_POINT('Ctrl Pts',(1.38425435883773,-1.,3.78469969805134));
#47781=CARTESIAN_POINT('Ctrl Pts',(1.38425435883773,1.,3.78469969805134));
#47782=CARTESIAN_POINT('Ctrl Pts',(1.38437354551435,-1.,3.77704902230441));
#47783=CARTESIAN_POINT('Ctrl Pts',(1.38437354551435,1.,3.77704902230441));
#47784=CARTESIAN_POINT('Ctrl Pts',(1.38445107339517,-1.,3.76940473185775));
#47785=CARTESIAN_POINT('Ctrl Pts',(1.38445107339517,1.,3.76940473185775));
#47786=CARTESIAN_POINT('Ctrl Pts',(1.38448675253343,-1.,3.76176768271347));
#47787=CARTESIAN_POINT('Ctrl Pts',(1.38448675253343,1.,3.76176768271347));
#47788=CARTESIAN_POINT('Ctrl Pts',(1.38448077997155,-1.,3.75413976318727));
#47789=CARTESIAN_POINT('Ctrl Pts',(1.38448077997155,1.,3.75413976318727));
#47790=CARTESIAN_POINT('Ctrl Pts',(1.38443344984389,-1.,3.7465231716786));
#47791=CARTESIAN_POINT('Ctrl Pts',(1.38443344984389,1.,3.7465231716786));
#47792=CARTESIAN_POINT('Ctrl Pts',(1.38434489156456,-1.,3.73891976418099));
#47793=CARTESIAN_POINT('Ctrl Pts',(1.38434489156456,1.,3.73891976418099));
#47794=CARTESIAN_POINT('Ctrl Pts',(1.38421479111531,-1.,3.73133035859283));
#47795=CARTESIAN_POINT('Ctrl Pts',(1.38421479111531,1.,3.73133035859283));
#47796=CARTESIAN_POINT('Ctrl Pts',(1.3840421342895,-1.,3.72375409358805));
#47797=CARTESIAN_POINT('Ctrl Pts',(1.3840421342895,1.,3.72375409358805));
#47798=CARTESIAN_POINT('Ctrl Pts',(1.38382489984585,-1.,3.7161876605181));
#47799=CARTESIAN_POINT('Ctrl Pts',(1.38382489984585,1.,3.7161876605181));
#47800=CARTESIAN_POINT('Ctrl Pts',(1.38356065402122,-1.,3.70862680753343));
#47801=CARTESIAN_POINT('Ctrl Pts',(1.38356065402122,1.,3.70862680753343));
#47802=CARTESIAN_POINT('Ctrl Pts',(1.38324717612862,-1.,3.70106792167894));
#47803=CARTESIAN_POINT('Ctrl Pts',(1.38324717612862,1.,3.70106792167894));
#47804=CARTESIAN_POINT('Ctrl Pts',(1.38288311171649,-1.,3.69350967899523));
#47805=CARTESIAN_POINT('Ctrl Pts',(1.38288311171649,1.,3.69350967899523));
#47806=CARTESIAN_POINT('Ctrl Pts',(1.38246852827185,-1.,3.68595444983844));
#47807=CARTESIAN_POINT('Ctrl Pts',(1.38246852827185,1.,3.68595444983844));
#47808=CARTESIAN_POINT('Ctrl Pts',(1.38200574290626,-1.,3.6784103848243));
#47809=CARTESIAN_POINT('Ctrl Pts',(1.38200574290626,1.,3.6784103848243));
#47810=CARTESIAN_POINT('Ctrl Pts',(1.38149812653876,-1.,3.67088843112282));
#47811=CARTESIAN_POINT('Ctrl Pts',(1.38149812653876,1.,3.67088843112282));
#47812=CARTESIAN_POINT('Ctrl Pts',(1.38094856333558,-1.,3.66339848520874));
#47813=CARTESIAN_POINT('Ctrl Pts',(1.38094856333558,1.,3.66339848520874));
#47814=CARTESIAN_POINT('Ctrl Pts',(1.38035791051215,-1.,3.65594554404396));
#47815=CARTESIAN_POINT('Ctrl Pts',(1.38035791051215,1.,3.65594554404396));
#47816=CARTESIAN_POINT('Ctrl Pts',(1.37972372481598,-1.,3.64852652756444));
#47817=CARTESIAN_POINT('Ctrl Pts',(1.37972372481598,1.,3.64852652756444));
#47818=CARTESIAN_POINT('Ctrl Pts',(1.37903818567347,-1.,3.64112507791112));
#47819=CARTESIAN_POINT('Ctrl Pts',(1.37903818567347,1.,3.64112507791112));
#47820=CARTESIAN_POINT('Ctrl Pts',(1.37829035457324,-1.,3.63371727442448));
#47821=CARTESIAN_POINT('Ctrl Pts',(1.37829035457324,1.,3.63371727442448));
#47822=CARTESIAN_POINT('Ctrl Pts',(1.37746987919868,-1.,3.62628098665112));
#47823=CARTESIAN_POINT('Ctrl Pts',(1.37746987919868,1.,3.62628098665112));
#47824=CARTESIAN_POINT('Ctrl Pts',(1.37657053403102,-1.,3.61880481160408));
#47825=CARTESIAN_POINT('Ctrl Pts',(1.37657053403102,1.,3.61880481160408));
#47826=CARTESIAN_POINT('Ctrl Pts',(1.37559314436641,-1.,3.61129546591082));
#47827=CARTESIAN_POINT('Ctrl Pts',(1.37559314436641,1.,3.61129546591082));
#47828=CARTESIAN_POINT('Ctrl Pts',(1.37455051379642,-1.,3.60379020124038));
#47829=CARTESIAN_POINT('Ctrl Pts',(1.37455051379642,1.,3.60379020124038));
#47830=CARTESIAN_POINT('Ctrl Pts',(1.37346320103184,-1.,3.59634627869117));
#47831=CARTESIAN_POINT('Ctrl Pts',(1.37346320103184,1.,3.59634627869117));
#47832=CARTESIAN_POINT('Ctrl Pts',(1.37235053661,-1.,3.5890185384643));
#47833=CARTESIAN_POINT('Ctrl Pts',(1.37235053661,1.,3.5890185384643));
#47834=CARTESIAN_POINT('Ctrl Pts',(1.37122241663073,-1.,3.58183885982745));
#47835=CARTESIAN_POINT('Ctrl Pts',(1.37122241663073,1.,3.58183885982745));
#47836=CARTESIAN_POINT('Ctrl Pts',(1.37007229485646,-1.,3.57479875549453));
#47837=CARTESIAN_POINT('Ctrl Pts',(1.37007229485646,1.,3.57479875549453));
#47838=CARTESIAN_POINT('Ctrl Pts',(1.36886584973349,-1.,3.56782080304554));
#47839=CARTESIAN_POINT('Ctrl Pts',(1.36886584973349,1.,3.56782080304554));
#47840=CARTESIAN_POINT('Ctrl Pts',(1.36754771771174,-1.,3.56077662028492));
#47841=CARTESIAN_POINT('Ctrl Pts',(1.36754771771174,1.,3.56077662028492));
#47842=CARTESIAN_POINT('Ctrl Pts',(1.36606145456711,-1.,3.55353883995793));
#47843=CARTESIAN_POINT('Ctrl Pts',(1.36606145456711,1.,3.55353883995793));
#47844=CARTESIAN_POINT('Ctrl Pts',(1.36436666257567,-1.,3.54602591832893));
#47845=CARTESIAN_POINT('Ctrl Pts',(1.36436666257567,1.,3.54602591832893));
#47846=CARTESIAN_POINT('Ctrl Pts',(1.36245507339334,-1.,3.53824396425032));
#47847=CARTESIAN_POINT('Ctrl Pts',(1.36245507339334,1.,3.53824396425032));
#47848=CARTESIAN_POINT('Ctrl Pts',(1.36037259643827,-1.,3.53034464961849));
#47849=CARTESIAN_POINT('Ctrl Pts',(1.36037259643827,1.,3.53034464961849));
#47850=CARTESIAN_POINT('Ctrl Pts',(1.35821701528975,-1.,3.52261776117121));
#47851=CARTESIAN_POINT('Ctrl Pts',(1.35821701528975,1.,3.52261776117121));
#47852=CARTESIAN_POINT('Ctrl Pts',(1.35611275237288,-1.,3.51542230699919));
#47853=CARTESIAN_POINT('Ctrl Pts',(1.35611275237288,1.,3.51542230699919));
#47854=CARTESIAN_POINT('Ctrl Pts',(1.35419113576022,-1.,3.50913227060177));
#47855=CARTESIAN_POINT('Ctrl Pts',(1.35419113576022,1.,3.50913227060177));
#47856=CARTESIAN_POINT('Ctrl Pts',(1.3525703284343,-1.,3.50408168106113));
#47857=CARTESIAN_POINT('Ctrl Pts',(1.3525703284343,1.,3.50408168106113));
#47858=CARTESIAN_POINT('Ctrl Pts',(1.35133076331065,-1.,3.50049707063673));
#47859=CARTESIAN_POINT('Ctrl Pts',(1.35133076331065,1.,3.50049707063673));
#47860=CARTESIAN_POINT('Ctrl Pts',(1.35067437417289,-1.,3.49888720256612));
#47861=CARTESIAN_POINT('Ctrl Pts',(1.35067437417289,1.,3.49888720256612));
#47862=CARTESIAN_POINT('Ctrl Pts',(1.35037650302887,-1.,3.49840357193384));
#47863=CARTESIAN_POINT('Ctrl Pts',(1.35037650302887,1.,3.49840357193384));
#47864=CARTESIAN_POINT('Ctrl Pts',(1.35026426118351,-1.,3.49840260053616));
#47865=CARTESIAN_POINT('Ctrl Pts',(1.35026426118351,1.,3.49840260053616));
#47866=CARTESIAN_POINT('Ctrl Pts',(1.35022972712301,-1.,3.49848248301936));
#47867=CARTESIAN_POINT('Ctrl Pts',(1.35022972712301,1.,3.49848248301936));
#47868=CARTESIAN_POINT('',(1.36999806084572,1.,3.97027773754922));
#47869=CARTESIAN_POINT('Ctrl Pts',(1.36999806084572,1.,3.97027773754922));
#47870=CARTESIAN_POINT('Ctrl Pts',(1.37020239094758,1.,3.9687184694173));
#47871=CARTESIAN_POINT('Ctrl Pts',(1.37060761746027,1.,3.96560037975788));
#47872=CARTESIAN_POINT('Ctrl Pts',(1.37120515615663,1.,3.96092458508407));
#47873=CARTESIAN_POINT('Ctrl Pts',(1.37198126433139,1.,3.95469287283105));
#47874=CARTESIAN_POINT('Ctrl Pts',(1.37291699203423,1.,3.94690771786926));
#47875=CARTESIAN_POINT('Ctrl Pts',(1.37381821967499,1.,3.93912709041791));
#47876=CARTESIAN_POINT('Ctrl Pts',(1.37468482215784,1.,3.93135106761941));
#47877=CARTESIAN_POINT('Ctrl Pts',(1.37551664448057,1.,3.92357976987132));
#47878=CARTESIAN_POINT('Ctrl Pts',(1.37631350505516,1.,3.91581337461825));
#47879=CARTESIAN_POINT('Ctrl Pts',(1.3770751963376,1.,3.90805209522729));
#47880=CARTESIAN_POINT('Ctrl Pts',(1.3778014851263,1.,3.90029615196255));
#47881=CARTESIAN_POINT('Ctrl Pts',(1.37849211287981,1.,3.89254574338385));
#47882=CARTESIAN_POINT('Ctrl Pts',(1.37914679719446,1.,3.88480102249461));
#47883=CARTESIAN_POINT('Ctrl Pts',(1.37976523097187,1.,3.87706205830865));
#47884=CARTESIAN_POINT('Ctrl Pts',(1.38034709213129,1.,3.86932885813403));
#47885=CARTESIAN_POINT('Ctrl Pts',(1.38089205993067,1.,3.86160143044187));
#47886=CARTESIAN_POINT('Ctrl Pts',(1.38139983115075,1.,3.85387983979557));
#47887=CARTESIAN_POINT('Ctrl Pts',(1.38187013346089,1.,3.84616425605705));
#47888=CARTESIAN_POINT('Ctrl Pts',(1.38230274828774,1.,3.83845502790609));
#47889=CARTESIAN_POINT('Ctrl Pts',(1.38269750245086,1.,3.83075266982138));
#47890=CARTESIAN_POINT('Ctrl Pts',(1.38305421262724,1.,3.82305771743715));
#47891=CARTESIAN_POINT('Ctrl Pts',(1.38337263902766,1.,3.81537060817765));
#47892=CARTESIAN_POINT('Ctrl Pts',(1.38365244046226,1.,3.80769156398429));
#47893=CARTESIAN_POINT('Ctrl Pts',(1.38389311766701,1.,3.80002044322169));
#47894=CARTESIAN_POINT('Ctrl Pts',(1.38409399694588,1.,3.79235669640907));
#47895=CARTESIAN_POINT('Ctrl Pts',(1.38425435883773,1.,3.78469969805134));
#47896=CARTESIAN_POINT('Ctrl Pts',(1.38437354551435,1.,3.77704902230441));
#47897=CARTESIAN_POINT('Ctrl Pts',(1.38445107339517,1.,3.76940473185775));
#47898=CARTESIAN_POINT('Ctrl Pts',(1.38448675253343,1.,3.76176768271347));
#47899=CARTESIAN_POINT('Ctrl Pts',(1.38448077997155,1.,3.75413976318727));
#47900=CARTESIAN_POINT('Ctrl Pts',(1.38443344984389,1.,3.7465231716786));
#47901=CARTESIAN_POINT('Ctrl Pts',(1.38434489156456,1.,3.73891976418099));
#47902=CARTESIAN_POINT('Ctrl Pts',(1.38421479111531,1.,3.73133035859283));
#47903=CARTESIAN_POINT('Ctrl Pts',(1.3840421342895,1.,3.72375409358805));
#47904=CARTESIAN_POINT('Ctrl Pts',(1.38382489984585,1.,3.7161876605181));
#47905=CARTESIAN_POINT('Ctrl Pts',(1.38356065402122,1.,3.70862680753343));
#47906=CARTESIAN_POINT('Ctrl Pts',(1.38324717612862,1.,3.70106792167894));
#47907=CARTESIAN_POINT('Ctrl Pts',(1.38288311171649,1.,3.69350967899523));
#47908=CARTESIAN_POINT('Ctrl Pts',(1.38246852827185,1.,3.68595444983844));
#47909=CARTESIAN_POINT('Ctrl Pts',(1.38200574290626,1.,3.6784103848243));
#47910=CARTESIAN_POINT('Ctrl Pts',(1.38149812653876,1.,3.67088843112282));
#47911=CARTESIAN_POINT('Ctrl Pts',(1.38094856333558,1.,3.66339848520874));
#47912=CARTESIAN_POINT('Ctrl Pts',(1.38035791051215,1.,3.65594554404396));
#47913=CARTESIAN_POINT('Ctrl Pts',(1.37972372481598,1.,3.64852652756444));
#47914=CARTESIAN_POINT('Ctrl Pts',(1.37903818567347,1.,3.64112507791112));
#47915=CARTESIAN_POINT('Ctrl Pts',(1.37829035457324,1.,3.63371727442448));
#47916=CARTESIAN_POINT('Ctrl Pts',(1.37746987919868,1.,3.62628098665112));
#47917=CARTESIAN_POINT('Ctrl Pts',(1.37657053403102,1.,3.61880481160408));
#47918=CARTESIAN_POINT('Ctrl Pts',(1.37559314436641,1.,3.61129546591082));
#47919=CARTESIAN_POINT('Ctrl Pts',(1.37455051379642,1.,3.60379020124038));
#47920=CARTESIAN_POINT('Ctrl Pts',(1.37346320103184,1.,3.59634627869117));
#47921=CARTESIAN_POINT('Ctrl Pts',(1.37235053661,1.,3.5890185384643));
#47922=CARTESIAN_POINT('Ctrl Pts',(1.37122241663073,1.,3.58183885982745));
#47923=CARTESIAN_POINT('Ctrl Pts',(1.37007229485646,1.,3.57479875549453));
#47924=CARTESIAN_POINT('Ctrl Pts',(1.36886584973349,1.,3.56782080304554));
#47925=CARTESIAN_POINT('Ctrl Pts',(1.36754771771174,1.,3.56077662028492));
#47926=CARTESIAN_POINT('Ctrl Pts',(1.36606145456711,1.,3.55353883995793));
#47927=CARTESIAN_POINT('Ctrl Pts',(1.36436666257567,1.,3.54602591832893));
#47928=CARTESIAN_POINT('Ctrl Pts',(1.36245507339334,1.,3.53824396425032));
#47929=CARTESIAN_POINT('Ctrl Pts',(1.36037259643827,1.,3.53034464961849));
#47930=CARTESIAN_POINT('Ctrl Pts',(1.35821701528975,1.,3.52261776117121));
#47931=CARTESIAN_POINT('Ctrl Pts',(1.35611275237288,1.,3.51542230699919));
#47932=CARTESIAN_POINT('Ctrl Pts',(1.35419113576022,1.,3.50913227060177));
#47933=CARTESIAN_POINT('Ctrl Pts',(1.3525703284343,1.,3.50408168106113));
#47934=CARTESIAN_POINT('Ctrl Pts',(1.35142377279535,1.,3.5007660381658));
#47935=CARTESIAN_POINT('Ctrl Pts',(1.35080045218652,1.,3.49920025459856));
#47936=CARTESIAN_POINT('Ctrl Pts',(1.35049736560633,1.,3.49861894124915));
#47937=CARTESIAN_POINT('Ctrl Pts',(1.35036670893102,1.,3.49847119623841));
#47938=CARTESIAN_POINT('Ctrl Pts',(1.35032489087269,1.,3.49844575334386));
#47939=CARTESIAN_POINT('',(1.36999806084572,0.,3.97027773754922));
#47940=CARTESIAN_POINT('Ctrl Pts',(0.96399761336957,-1.,3.62397690409552));
#47941=CARTESIAN_POINT('Ctrl Pts',(0.96399761336957,1.,3.62397690409552));
#47942=CARTESIAN_POINT('Ctrl Pts',(0.963922720982576,-1.,3.62393257642191));
#47943=CARTESIAN_POINT('Ctrl Pts',(0.963922720982576,1.,3.62393257642191));
#47944=CARTESIAN_POINT('Ctrl Pts',(0.963832486396055,-1.,3.62399933640277));
#47945=CARTESIAN_POINT('Ctrl Pts',(0.963832486396055,1.,3.62399933640277));
#47946=CARTESIAN_POINT('Ctrl Pts',(0.963875774532102,-1.,3.62456568607055));
#47947=CARTESIAN_POINT('Ctrl Pts',(0.963875774532102,1.,3.62456568607055));
#47948=CARTESIAN_POINT('Ctrl Pts',(0.964291001274618,-1.,3.62625391255277));
#47949=CARTESIAN_POINT('Ctrl Pts',(0.964291001274618,1.,3.62625391255277));
#47950=CARTESIAN_POINT('Ctrl Pts',(0.965395153165715,-1.,3.62988252139998));
#47951=CARTESIAN_POINT('Ctrl Pts',(0.965395153165715,1.,3.62988252139998));
#47952=CARTESIAN_POINT('Ctrl Pts',(0.967052554540877,-1.,3.6349212208096));
#47953=CARTESIAN_POINT('Ctrl Pts',(0.967052554540877,1.,3.6349212208096));
#47954=CARTESIAN_POINT('Ctrl Pts',(0.969195124674828,-1.,3.64113946505393));
#47955=CARTESIAN_POINT('Ctrl Pts',(0.969195124674828,1.,3.64113946505393));
#47956=CARTESIAN_POINT('Ctrl Pts',(0.971722122060277,-1.,3.64819756447072));
#47957=CARTESIAN_POINT('Ctrl Pts',(0.971722122060277,1.,3.64819756447072));
#47958=CARTESIAN_POINT('Ctrl Pts',(0.974519971354138,-1.,3.6557157673487));
#47959=CARTESIAN_POINT('Ctrl Pts',(0.974519971354138,1.,3.6557157673487));
#47960=CARTESIAN_POINT('Ctrl Pts',(0.977478312751416,-1.,3.66333049637403));
#47961=CARTESIAN_POINT('Ctrl Pts',(0.977478312751416,1.,3.66333049637403));
#47962=CARTESIAN_POINT('Ctrl Pts',(0.980505922458494,-1.,3.67074983340444));
#47963=CARTESIAN_POINT('Ctrl Pts',(0.980505922458494,1.,3.67074983340444));
#47964=CARTESIAN_POINT('Ctrl Pts',(0.983550791470864,-1.,3.67782408841876));
#47965=CARTESIAN_POINT('Ctrl Pts',(0.983550791470864,1.,3.67782408841876));
#47966=CARTESIAN_POINT('Ctrl Pts',(0.986602639864285,-1.,3.6845531792623));
#47967=CARTESIAN_POINT('Ctrl Pts',(0.986602639864285,1.,3.6845531792623));
#47968=CARTESIAN_POINT('Ctrl Pts',(0.989676715398858,-1.,3.69102682138955));
#47969=CARTESIAN_POINT('Ctrl Pts',(0.989676715398858,1.,3.69102682138955));
#47970=CARTESIAN_POINT('Ctrl Pts',(0.992802218332103,-1.,3.69738123415696));
#47971=CARTESIAN_POINT('Ctrl Pts',(0.992802218332103,1.,3.69738123415696));
#47972=CARTESIAN_POINT('Ctrl Pts',(0.996009819772431,-1.,3.70375282282107));
#47973=CARTESIAN_POINT('Ctrl Pts',(0.996009819772431,1.,3.70375282282107));
#47974=CARTESIAN_POINT('Ctrl Pts',(0.999317260756344,-1.,3.7102243971387));
#47975=CARTESIAN_POINT('Ctrl Pts',(0.999317260756344,1.,3.7102243971387));
#47976=CARTESIAN_POINT('Ctrl Pts',(1.00272423396802,-1.,3.71680667125047));
#47977=CARTESIAN_POINT('Ctrl Pts',(1.00272423396802,1.,3.71680667125047));
#47978=CARTESIAN_POINT('Ctrl Pts',(1.00622000735696,-1.,3.72346803750544));
#47979=CARTESIAN_POINT('Ctrl Pts',(1.00622000735696,1.,3.72346803750544));
#47980=CARTESIAN_POINT('Ctrl Pts',(1.00978798539491,-1.,3.73015276704407));
#47981=CARTESIAN_POINT('Ctrl Pts',(1.00978798539491,1.,3.73015276704407));
#47982=CARTESIAN_POINT('Ctrl Pts',(1.01341114319906,-1.,3.73680245055747));
#47983=CARTESIAN_POINT('Ctrl Pts',(1.01341114319906,1.,3.73680245055747));
#47984=CARTESIAN_POINT('Ctrl Pts',(1.01707794311088,-1.,3.74337942504993));
#47985=CARTESIAN_POINT('Ctrl Pts',(1.01707794311088,1.,3.74337942504993));
#47986=CARTESIAN_POINT('Ctrl Pts',(1.02078510487439,-1.,3.74987777155873));
#47987=CARTESIAN_POINT('Ctrl Pts',(1.02078510487439,1.,3.74987777155873));
#47988=CARTESIAN_POINT('Ctrl Pts',(1.02453429444668,-1.,3.75631037456224));
#47989=CARTESIAN_POINT('Ctrl Pts',(1.02453429444668,1.,3.75631037456224));
#47990=CARTESIAN_POINT('Ctrl Pts',(1.02833014458184,-1.,3.76270122291245));
#47991=CARTESIAN_POINT('Ctrl Pts',(1.02833014458184,1.,3.76270122291245));
#47992=CARTESIAN_POINT('Ctrl Pts',(1.03217786604919,-1.,3.76907609832516));
#47993=CARTESIAN_POINT('Ctrl Pts',(1.03217786604919,1.,3.76907609832516));
#47994=CARTESIAN_POINT('Ctrl Pts',(1.03608074678008,-1.,3.77545283140427));
#47995=CARTESIAN_POINT('Ctrl Pts',(1.03608074678008,1.,3.77545283140427));
#47996=CARTESIAN_POINT('Ctrl Pts',(1.04003862055798,-1.,3.7818353500817));
#47997=CARTESIAN_POINT('Ctrl Pts',(1.04003862055798,1.,3.7818353500817));
#47998=CARTESIAN_POINT('Ctrl Pts',(1.04404924374422,-1.,3.78821910787179));
#47999=CARTESIAN_POINT('Ctrl Pts',(1.04404924374422,1.,3.78821910787179));
#48000=CARTESIAN_POINT('Ctrl Pts',(1.04810913267639,-1.,3.79459440308786));
#48001=CARTESIAN_POINT('Ctrl Pts',(1.04810913267639,1.,3.79459440308786));
#48002=CARTESIAN_POINT('Ctrl Pts',(1.05221457990016,-1.,3.80095039790681));
#48003=CARTESIAN_POINT('Ctrl Pts',(1.05221457990016,1.,3.80095039790681));
#48004=CARTESIAN_POINT('Ctrl Pts',(1.05636266918644,-1.,3.80727913637791));
#48005=CARTESIAN_POINT('Ctrl Pts',(1.05636266918644,1.,3.80727913637791));
#48006=CARTESIAN_POINT('Ctrl Pts',(1.06055206187299,-1.,3.8135786611749));
#48007=CARTESIAN_POINT('Ctrl Pts',(1.06055206187299,1.,3.8135786611749));
#48008=CARTESIAN_POINT('Ctrl Pts',(1.0647824403893,-1.,3.81985083953012));
#48009=CARTESIAN_POINT('Ctrl Pts',(1.0647824403893,1.,3.81985083953012));
#48010=CARTESIAN_POINT('Ctrl Pts',(1.06905413180359,-1.,3.82609989967276));
#48011=CARTESIAN_POINT('Ctrl Pts',(1.06905413180359,1.,3.82609989967276));
#48012=CARTESIAN_POINT('Ctrl Pts',(1.07336766633459,-1.,3.83233071195144));
#48013=CARTESIAN_POINT('Ctrl Pts',(1.07336766633459,1.,3.83233071195144));
#48014=CARTESIAN_POINT('Ctrl Pts',(1.07772335353858,-1.,3.83854714117491));
#48015=CARTESIAN_POINT('Ctrl Pts',(1.07772335353858,1.,3.83854714117491));
#48016=CARTESIAN_POINT('Ctrl Pts',(1.08212087917991,-1.,3.8447504803063));
#48017=CARTESIAN_POINT('Ctrl Pts',(1.08212087917991,1.,3.8447504803063));
#48018=CARTESIAN_POINT('Ctrl Pts',(1.08655950846384,-1.,3.85094025222713));
#48019=CARTESIAN_POINT('Ctrl Pts',(1.08655950846384,1.,3.85094025222713));
#48020=CARTESIAN_POINT('Ctrl Pts',(1.09103825516294,-1.,3.85711487933931));
#48021=CARTESIAN_POINT('Ctrl Pts',(1.09103825516294,1.,3.85711487933931));
#48022=CARTESIAN_POINT('Ctrl Pts',(1.09555606505013,-1.,3.86327241021247));
#48023=CARTESIAN_POINT('Ctrl Pts',(1.09555606505013,1.,3.86327241021247));
#48024=CARTESIAN_POINT('Ctrl Pts',(1.10011198761195,-1.,3.86941120134849));
#48025=CARTESIAN_POINT('Ctrl Pts',(1.10011198761195,1.,3.86941120134849));
#48026=CARTESIAN_POINT('Ctrl Pts',(1.10470536603287,-1.,3.87553067187514));
#48027=CARTESIAN_POINT('Ctrl Pts',(1.10470536603287,1.,3.87553067187514));
#48028=CARTESIAN_POINT('Ctrl Pts',(1.10933577224008,-1.,3.88163105531724));
#48029=CARTESIAN_POINT('Ctrl Pts',(1.10933577224008,1.,3.88163105531724));
#48030=CARTESIAN_POINT('Ctrl Pts',(1.11400292434429,-1.,3.88771308285171));
#48031=CARTESIAN_POINT('Ctrl Pts',(1.11400292434429,1.,3.88771308285171));
#48032=CARTESIAN_POINT('Ctrl Pts',(1.11870660794603,-1.,3.89377768340344));
#48033=CARTESIAN_POINT('Ctrl Pts',(1.11870660794603,1.,3.89377768340344));
#48034=CARTESIAN_POINT('Ctrl Pts',(1.12344660099043,-1.,3.89982569750025));
#48035=CARTESIAN_POINT('Ctrl Pts',(1.12344660099043,1.,3.89982569750025));
#48036=CARTESIAN_POINT('Ctrl Pts',(1.12822258281553,-1.,3.90585753318737));
#48037=CARTESIAN_POINT('Ctrl Pts',(1.12822258281553,1.,3.90585753318737));
#48038=CARTESIAN_POINT('Ctrl Pts',(1.13303414693896,-1.,3.91187321145649));
#48039=CARTESIAN_POINT('Ctrl Pts',(1.13303414693896,1.,3.91187321145649));
#48040=CARTESIAN_POINT('Ctrl Pts',(1.13788084225554,-1.,3.91787251936827));
#48041=CARTESIAN_POINT('Ctrl Pts',(1.13788084225554,1.,3.91787251936827));
#48042=CARTESIAN_POINT('Ctrl Pts',(1.14276220561593,-1.,3.92385513133997));
#48043=CARTESIAN_POINT('Ctrl Pts',(1.14276220561593,1.,3.92385513133997));
#48044=CARTESIAN_POINT('Ctrl Pts',(1.14767779451123,-1.,3.92982073294257));
#48045=CARTESIAN_POINT('Ctrl Pts',(1.14767779451123,1.,3.92982073294257));
#48046=CARTESIAN_POINT('Ctrl Pts',(1.1526272271632,-1.,3.9357691705628));
#48047=CARTESIAN_POINT('Ctrl Pts',(1.1526272271632,1.,3.9357691705628));
#48048=CARTESIAN_POINT('Ctrl Pts',(1.15761018340956,-1.,3.94170046685203));
#48049=CARTESIAN_POINT('Ctrl Pts',(1.15761018340956,1.,3.94170046685203));
#48050=CARTESIAN_POINT('Ctrl Pts',(1.16262637999157,-1.,3.94761474780583));
#48051=CARTESIAN_POINT('Ctrl Pts',(1.16262637999157,1.,3.94761474780583));
#48052=CARTESIAN_POINT('Ctrl Pts',(1.16767555244438,-1.,3.95351219509876));
#48053=CARTESIAN_POINT('Ctrl Pts',(1.16767555244438,1.,3.95351219509876));
#48054=CARTESIAN_POINT('Ctrl Pts',(1.17275743590361,-1.,3.95939299213276));
#48055=CARTESIAN_POINT('Ctrl Pts',(1.17275743590361,1.,3.95939299213276));
#48056=CARTESIAN_POINT('Ctrl Pts',(1.17787174135592,-1.,3.96525726358159));
#48057=CARTESIAN_POINT('Ctrl Pts',(1.17787174135592,1.,3.96525726358159));
#48058=CARTESIAN_POINT('Ctrl Pts',(1.18301815039831,-1.,3.97110505165415));
#48059=CARTESIAN_POINT('Ctrl Pts',(1.18301815039831,1.,3.97110505165415));
#48060=CARTESIAN_POINT('Ctrl Pts',(1.18819633715539,-1.,3.97693634767754));
#48061=CARTESIAN_POINT('Ctrl Pts',(1.18819633715539,1.,3.97693634767754));
#48062=CARTESIAN_POINT('Ctrl Pts',(1.19340598349475,-1.,3.98275111052561));
#48063=CARTESIAN_POINT('Ctrl Pts',(1.19340598349475,1.,3.98275111052561));
#48064=CARTESIAN_POINT('Ctrl Pts',(1.19864679609566,-1.,3.98854928957189));
#48065=CARTESIAN_POINT('Ctrl Pts',(1.19864679609566,1.,3.98854928957189));
#48066=CARTESIAN_POINT('Ctrl Pts',(1.20391852375138,-1.,3.99433084799666));
#48067=CARTESIAN_POINT('Ctrl Pts',(1.20391852375138,1.,3.99433084799666));
#48068=CARTESIAN_POINT('Ctrl Pts',(1.20922097029551,-1.,4.00009577950721));
#48069=CARTESIAN_POINT('Ctrl Pts',(1.20922097029551,1.,4.00009577950721));
#48070=CARTESIAN_POINT('Ctrl Pts',(1.21455398918133,-1.,4.00584409522722));
#48071=CARTESIAN_POINT('Ctrl Pts',(1.21455398918133,1.,4.00584409522722));
#48072=CARTESIAN_POINT('Ctrl Pts',(1.21884478244403,-1.,4.01042947140789));
#48073=CARTESIAN_POINT('Ctrl Pts',(1.21884478244403,1.,4.01042947140789));
#48074=CARTESIAN_POINT('Ctrl Pts',(1.22207656455845,-1.,4.01386104433519));
#48075=CARTESIAN_POINT('Ctrl Pts',(1.22207656455845,1.,4.01386104433519));
#48076=CARTESIAN_POINT('Ctrl Pts',(1.22423716681317,-1.,4.01614544569895));
#48077=CARTESIAN_POINT('Ctrl Pts',(1.22423716681317,1.,4.01614544569895));
#48078=CARTESIAN_POINT('Ctrl Pts',(1.22531898815164,-1.,4.01728681790024));
#48079=CARTESIAN_POINT('Ctrl Pts',(1.22531898815164,1.,4.01728681790024));
#48080=CARTESIAN_POINT('',(0.963899035118985,1.,3.62400312501199));
#48081=CARTESIAN_POINT('Ctrl Pts',(0.963899035118985,-1.,3.62400312501199));
#48082=CARTESIAN_POINT('Ctrl Pts',(0.963899035118985,-0.666666666666667,
3.62400312501199));
#48083=CARTESIAN_POINT('Ctrl Pts',(0.963899035118985,-0.333333333333333,
3.62400312501199));
#48084=CARTESIAN_POINT('Ctrl Pts',(0.963899035118985,0.333333333333333,
3.62400312501199));
#48085=CARTESIAN_POINT('Ctrl Pts',(0.963899035118985,0.666666666666667,
3.62400312501199));
#48086=CARTESIAN_POINT('Ctrl Pts',(0.963899035118985,1.,3.62400312501199));
#48087=CARTESIAN_POINT('',(1.22531898815164,1.,4.01728681790024));
#48088=CARTESIAN_POINT('',(1.22531898815164,0.,4.01728681790024));
#48089=CARTESIAN_POINT('Ctrl Pts',(0.963899035118985,1.,3.62400312501199));
#48090=CARTESIAN_POINT('Ctrl Pts',(0.963880158556712,1.,3.62404828878375));
#48091=CARTESIAN_POINT('Ctrl Pts',(0.963861297423578,1.,3.62424461507455));
#48092=CARTESIAN_POINT('Ctrl Pts',(0.963957782642589,1.,3.62489305727516));
#48093=CARTESIAN_POINT('Ctrl Pts',(0.964373850166081,1.,3.62652618145252));
#48094=CARTESIAN_POINT('Ctrl Pts',(0.965395153165715,1.,3.62988252139998));
#48095=CARTESIAN_POINT('Ctrl Pts',(0.967052554540877,1.,3.6349212208096));
#48096=CARTESIAN_POINT('Ctrl Pts',(0.969195124674828,1.,3.64113946505393));
#48097=CARTESIAN_POINT('Ctrl Pts',(0.971722122060277,1.,3.64819756447072));
#48098=CARTESIAN_POINT('Ctrl Pts',(0.974519971354138,1.,3.6557157673487));
#48099=CARTESIAN_POINT('Ctrl Pts',(0.977478312751416,1.,3.66333049637403));
#48100=CARTESIAN_POINT('Ctrl Pts',(0.980505922458494,1.,3.67074983340444));
#48101=CARTESIAN_POINT('Ctrl Pts',(0.983550791470864,1.,3.67782408841876));
#48102=CARTESIAN_POINT('Ctrl Pts',(0.986602639864285,1.,3.6845531792623));
#48103=CARTESIAN_POINT('Ctrl Pts',(0.989676715398858,1.,3.69102682138955));
#48104=CARTESIAN_POINT('Ctrl Pts',(0.992802218332103,1.,3.69738123415696));
#48105=CARTESIAN_POINT('Ctrl Pts',(0.996009819772431,1.,3.70375282282107));
#48106=CARTESIAN_POINT('Ctrl Pts',(0.999317260756344,1.,3.7102243971387));
#48107=CARTESIAN_POINT('Ctrl Pts',(1.00272423396802,1.,3.71680667125047));
#48108=CARTESIAN_POINT('Ctrl Pts',(1.00622000735696,1.,3.72346803750544));
#48109=CARTESIAN_POINT('Ctrl Pts',(1.00978798539491,1.,3.73015276704407));
#48110=CARTESIAN_POINT('Ctrl Pts',(1.01341114319906,1.,3.73680245055747));
#48111=CARTESIAN_POINT('Ctrl Pts',(1.01707794311088,1.,3.74337942504993));
#48112=CARTESIAN_POINT('Ctrl Pts',(1.02078510487439,1.,3.74987777155873));
#48113=CARTESIAN_POINT('Ctrl Pts',(1.02453429444668,1.,3.75631037456224));
#48114=CARTESIAN_POINT('Ctrl Pts',(1.02833014458184,1.,3.76270122291245));
#48115=CARTESIAN_POINT('Ctrl Pts',(1.03217786604919,1.,3.76907609832516));
#48116=CARTESIAN_POINT('Ctrl Pts',(1.03608074678008,1.,3.77545283140427));
#48117=CARTESIAN_POINT('Ctrl Pts',(1.04003862055798,1.,3.7818353500817));
#48118=CARTESIAN_POINT('Ctrl Pts',(1.04404924374422,1.,3.78821910787179));
#48119=CARTESIAN_POINT('Ctrl Pts',(1.04810913267639,1.,3.79459440308786));
#48120=CARTESIAN_POINT('Ctrl Pts',(1.05221457990016,1.,3.80095039790681));
#48121=CARTESIAN_POINT('Ctrl Pts',(1.05636266918644,1.,3.80727913637791));
#48122=CARTESIAN_POINT('Ctrl Pts',(1.06055206187299,1.,3.8135786611749));
#48123=CARTESIAN_POINT('Ctrl Pts',(1.0647824403893,1.,3.81985083953012));
#48124=CARTESIAN_POINT('Ctrl Pts',(1.06905413180359,1.,3.82609989967276));
#48125=CARTESIAN_POINT('Ctrl Pts',(1.07336766633459,1.,3.83233071195144));
#48126=CARTESIAN_POINT('Ctrl Pts',(1.07772335353858,1.,3.83854714117491));
#48127=CARTESIAN_POINT('Ctrl Pts',(1.08212087917991,1.,3.8447504803063));
#48128=CARTESIAN_POINT('Ctrl Pts',(1.08655950846384,1.,3.85094025222713));
#48129=CARTESIAN_POINT('Ctrl Pts',(1.09103825516294,1.,3.85711487933931));
#48130=CARTESIAN_POINT('Ctrl Pts',(1.09555606505013,1.,3.86327241021247));
#48131=CARTESIAN_POINT('Ctrl Pts',(1.10011198761195,1.,3.86941120134849));
#48132=CARTESIAN_POINT('Ctrl Pts',(1.10470536603287,1.,3.87553067187514));
#48133=CARTESIAN_POINT('Ctrl Pts',(1.10933577224008,1.,3.88163105531724));
#48134=CARTESIAN_POINT('Ctrl Pts',(1.11400292434429,1.,3.88771308285171));
#48135=CARTESIAN_POINT('Ctrl Pts',(1.11870660794603,1.,3.89377768340344));
#48136=CARTESIAN_POINT('Ctrl Pts',(1.12344660099043,1.,3.89982569750025));
#48137=CARTESIAN_POINT('Ctrl Pts',(1.12822258281553,1.,3.90585753318737));
#48138=CARTESIAN_POINT('Ctrl Pts',(1.13303414693896,1.,3.91187321145649));
#48139=CARTESIAN_POINT('Ctrl Pts',(1.13788084225554,1.,3.91787251936827));
#48140=CARTESIAN_POINT('Ctrl Pts',(1.14276220561593,1.,3.92385513133997));
#48141=CARTESIAN_POINT('Ctrl Pts',(1.14767779451123,1.,3.92982073294257));
#48142=CARTESIAN_POINT('Ctrl Pts',(1.1526272271632,1.,3.9357691705628));
#48143=CARTESIAN_POINT('Ctrl Pts',(1.15761018340956,1.,3.94170046685203));
#48144=CARTESIAN_POINT('Ctrl Pts',(1.16262637999157,1.,3.94761474780583));
#48145=CARTESIAN_POINT('Ctrl Pts',(1.16767555244438,1.,3.95351219509876));
#48146=CARTESIAN_POINT('Ctrl Pts',(1.17275743590361,1.,3.95939299213276));
#48147=CARTESIAN_POINT('Ctrl Pts',(1.17787174135592,1.,3.96525726358159));
#48148=CARTESIAN_POINT('Ctrl Pts',(1.18301815039831,1.,3.97110505165415));
#48149=CARTESIAN_POINT('Ctrl Pts',(1.18819633715539,1.,3.97693634767754));
#48150=CARTESIAN_POINT('Ctrl Pts',(1.19340598349475,1.,3.98275111052561));
#48151=CARTESIAN_POINT('Ctrl Pts',(1.19864679609566,1.,3.98854928957189));
#48152=CARTESIAN_POINT('Ctrl Pts',(1.20391852375138,1.,3.99433084799666));
#48153=CARTESIAN_POINT('Ctrl Pts',(1.20922097029551,1.,4.00009577950721));
#48154=CARTESIAN_POINT('Ctrl Pts',(1.21455398918133,1.,4.00584409522722));
#48155=CARTESIAN_POINT('Ctrl Pts',(1.21884478244403,1.,4.01042947140789));
#48156=CARTESIAN_POINT('Ctrl Pts',(1.22207656455845,1.,4.01386104433519));
#48157=CARTESIAN_POINT('Ctrl Pts',(1.22423716681317,1.,4.01614544569895));
#48158=CARTESIAN_POINT('Ctrl Pts',(1.22531898815164,1.,4.01728681790024));
#48159=CARTESIAN_POINT('Origin',(1.22531898815164,0.,4.01728681790024));
#48160=CARTESIAN_POINT('',(1.36999806084572,1.,3.97027773754922));
#48161=CARTESIAN_POINT('Origin',(0.,0.,0.));
#48162=CARTESIAN_POINT('',(0.786422660833742,1.,3.66661143271648));
#48163=CARTESIAN_POINT('Origin',(0.,1.,0.));
#48164=CARTESIAN_POINT('Ctrl Pts',(0.786422660833742,1.,3.66661143271648));
#48165=CARTESIAN_POINT('Ctrl Pts',(0.786422660833742,0.666666666666667,
3.66661143271648));
#48166=CARTESIAN_POINT('Ctrl Pts',(0.786422660833742,0.333333333333333,
3.66661143271648));
#48167=CARTESIAN_POINT('Ctrl Pts',(0.786422660833742,-0.333333333333333,
3.66661143271648));
#48168=CARTESIAN_POINT('Ctrl Pts',(0.786422660833742,-0.666666666666667,
3.66661143271648));
#48169=CARTESIAN_POINT('Ctrl Pts',(0.786422660833742,-1.,3.66661143271648));
#48170=CARTESIAN_POINT('Ctrl Pts',(0.732042837400619,-1.,4.13571194405636));
#48171=CARTESIAN_POINT('Ctrl Pts',(0.732042837400619,1.,4.13571194405636));
#48172=CARTESIAN_POINT('Ctrl Pts',(0.732488575135925,-1.,4.13420383737278));
#48173=CARTESIAN_POINT('Ctrl Pts',(0.732488575135925,1.,4.13420383737278));
#48174=CARTESIAN_POINT('Ctrl Pts',(0.733376589325634,-1.,4.13118752796397));
#48175=CARTESIAN_POINT('Ctrl Pts',(0.733376589325634,1.,4.13118752796397));
#48176=CARTESIAN_POINT('Ctrl Pts',(0.734698226767512,-1.,4.12666277572794));
#48177=CARTESIAN_POINT('Ctrl Pts',(0.734698226767512,1.,4.12666277572794));
#48178=CARTESIAN_POINT('Ctrl Pts',(0.736439634335347,-1.,4.12062919626082));
#48179=CARTESIAN_POINT('Ctrl Pts',(0.736439634335347,1.,4.12062919626082));
#48180=CARTESIAN_POINT('Ctrl Pts',(0.738581708229118,-1.,4.11308626953795));
#48181=CARTESIAN_POINT('Ctrl Pts',(0.738581708229118,1.,4.11308626953795));
#48182=CARTESIAN_POINT('Ctrl Pts',(0.740688998555151,-1.,4.1055424175856));
#48183=CARTESIAN_POINT('Ctrl Pts',(0.740688998555151,1.,4.1055424175856));
#48184=CARTESIAN_POINT('Ctrl Pts',(0.742761369690017,-1.,4.09799769702712));
#48185=CARTESIAN_POINT('Ctrl Pts',(0.742761369690017,1.,4.09799769702712));
#48186=CARTESIAN_POINT('Ctrl Pts',(0.744798649705513,-1.,4.09045220253011));
#48187=CARTESIAN_POINT('Ctrl Pts',(0.744798649705513,1.,4.09045220253011));
#48188=CARTESIAN_POINT('Ctrl Pts',(0.746800631490821,-1.,4.08290608094789));
#48189=CARTESIAN_POINT('Ctrl Pts',(0.746800631490821,1.,4.08290608094789));
#48190=CARTESIAN_POINT('Ctrl Pts',(0.748767076679176,-1.,4.07535951055363));
#48191=CARTESIAN_POINT('Ctrl Pts',(0.748767076679176,1.,4.07535951055363));
#48192=CARTESIAN_POINT('Ctrl Pts',(0.750697720483175,-1.,4.06781267241886));
#48193=CARTESIAN_POINT('Ctrl Pts',(0.750697720483175,1.,4.06781267241886));
#48194=CARTESIAN_POINT('Ctrl Pts',(0.752592276482868,-1.,4.06026572221399));
#48195=CARTESIAN_POINT('Ctrl Pts',(0.752592276482868,1.,4.06026572221399));
#48196=CARTESIAN_POINT('Ctrl Pts',(0.754450441816411,-1.,4.05271876688106));
#48197=CARTESIAN_POINT('Ctrl Pts',(0.754450441816411,1.,4.05271876688106));
#48198=CARTESIAN_POINT('Ctrl Pts',(0.756271902370186,-1.,4.04517182654344));
#48199=CARTESIAN_POINT('Ctrl Pts',(0.756271902370186,1.,4.04517182654344));
#48200=CARTESIAN_POINT('Ctrl Pts',(0.758056338885553,-1.,4.03762485803468));
#48201=CARTESIAN_POINT('Ctrl Pts',(0.758056338885553,1.,4.03762485803468));
#48202=CARTESIAN_POINT('Ctrl Pts',(0.759803433244165,-1.,4.0300778195465));
#48203=CARTESIAN_POINT('Ctrl Pts',(0.759803433244165,1.,4.0300778195465));
#48204=CARTESIAN_POINT('Ctrl Pts',(0.761512875859941,-1.,4.02253072741347));
#48205=CARTESIAN_POINT('Ctrl Pts',(0.761512875859941,1.,4.02253072741347));
#48206=CARTESIAN_POINT('Ctrl Pts',(0.763184371182826,-1.,4.01498370680434));
#48207=CARTESIAN_POINT('Ctrl Pts',(0.763184371182826,1.,4.01498370680434));
#48208=CARTESIAN_POINT('Ctrl Pts',(0.764817648784946,-1.,4.00743706791366));
#48209=CARTESIAN_POINT('Ctrl Pts',(0.764817648784946,1.,4.00743706791366));
#48210=CARTESIAN_POINT('Ctrl Pts',(0.766412457135785,-1.,3.99989129179464));
#48211=CARTESIAN_POINT('Ctrl Pts',(0.766412457135785,1.,3.99989129179464));
#48212=CARTESIAN_POINT('Ctrl Pts',(0.767968531377707,-1.,3.99234687880892));
#48213=CARTESIAN_POINT('Ctrl Pts',(0.767968531377707,1.,3.99234687880892));
#48214=CARTESIAN_POINT('Ctrl Pts',(0.769485566245459,-1.,3.98480422348403));
#48215=CARTESIAN_POINT('Ctrl Pts',(0.769485566245459,1.,3.98480422348403));
#48216=CARTESIAN_POINT('Ctrl Pts',(0.770963190030503,-1.,3.97726349165507));
#48217=CARTESIAN_POINT('Ctrl Pts',(0.770963190030503,1.,3.97726349165507));
#48218=CARTESIAN_POINT('Ctrl Pts',(0.772400931772238,-1.,3.96972446532832));
#48219=CARTESIAN_POINT('Ctrl Pts',(0.772400931772238,1.,3.96972446532832));
#48220=CARTESIAN_POINT('Ctrl Pts',(0.773798212026682,-1.,3.96218649639876));
#48221=CARTESIAN_POINT('Ctrl Pts',(0.773798212026682,1.,3.96218649639876));
#48222=CARTESIAN_POINT('Ctrl Pts',(0.775154418039441,-1.,3.95464885452364));
#48223=CARTESIAN_POINT('Ctrl Pts',(0.775154418039441,1.,3.95464885452364));
#48224=CARTESIAN_POINT('Ctrl Pts',(0.776468966697959,-1.,3.94711101619471));
#48225=CARTESIAN_POINT('Ctrl Pts',(0.776468966697959,1.,3.94711101619471));
#48226=CARTESIAN_POINT('Ctrl Pts',(0.777741370568549,-1.,3.93957296768098));
#48227=CARTESIAN_POINT('Ctrl Pts',(0.777741370568549,1.,3.93957296768098));
#48228=CARTESIAN_POINT('Ctrl Pts',(0.778971308134786,-1.,3.93203552473153));
#48229=CARTESIAN_POINT('Ctrl Pts',(0.778971308134786,1.,3.93203552473153));
#48230=CARTESIAN_POINT('Ctrl Pts',(0.780158678615506,-1.,3.92450058323799));
#48231=CARTESIAN_POINT('Ctrl Pts',(0.780158678615506,1.,3.92450058323799));
#48232=CARTESIAN_POINT('Ctrl Pts',(0.781303428618343,-1.,3.9169703605466));
#48233=CARTESIAN_POINT('Ctrl Pts',(0.781303428618343,1.,3.9169703605466));
#48234=CARTESIAN_POINT('Ctrl Pts',(0.782405395622758,-1.,3.90944671004536));
#48235=CARTESIAN_POINT('Ctrl Pts',(0.782405395622758,1.,3.90944671004536));
#48236=CARTESIAN_POINT('Ctrl Pts',(0.783464141529082,-1.,3.90193039043971));
#48237=CARTESIAN_POINT('Ctrl Pts',(0.783464141529082,1.,3.90193039043971));
#48238=CARTESIAN_POINT('Ctrl Pts',(0.784478799358335,-1.,3.89442039235105));
#48239=CARTESIAN_POINT('Ctrl Pts',(0.784478799358335,1.,3.89442039235105));
#48240=CARTESIAN_POINT('Ctrl Pts',(0.785447890340723,-1.,3.88691313167399));
#48241=CARTESIAN_POINT('Ctrl Pts',(0.785447890340723,1.,3.88691313167399));
#48242=CARTESIAN_POINT('Ctrl Pts',(0.786369675812591,-1.,3.87940402818186));
#48243=CARTESIAN_POINT('Ctrl Pts',(0.786369675812591,1.,3.87940402818186));
#48244=CARTESIAN_POINT('Ctrl Pts',(0.78724252761798,-1.,3.87188916600905));
#48245=CARTESIAN_POINT('Ctrl Pts',(0.78724252761798,1.,3.87188916600905));
#48246=CARTESIAN_POINT('Ctrl Pts',(0.78806531509377,-1.,3.86436702561342));
#48247=CARTESIAN_POINT('Ctrl Pts',(0.78806531509377,1.,3.86436702561342));
#48248=CARTESIAN_POINT('Ctrl Pts',(0.788837734090688,-1.,3.85683995872536));
#48249=CARTESIAN_POINT('Ctrl Pts',(0.788837734090688,1.,3.85683995872536));
#48250=CARTESIAN_POINT('Ctrl Pts',(0.789560798155618,-1.,3.8493163780891));
#48251=CARTESIAN_POINT('Ctrl Pts',(0.789560798155618,1.,3.8493163780891));
#48252=CARTESIAN_POINT('Ctrl Pts',(0.790236124191289,-1.,3.84180762342476));
#48253=CARTESIAN_POINT('Ctrl Pts',(0.790236124191289,1.,3.84180762342476));
#48254=CARTESIAN_POINT('Ctrl Pts',(0.790865012705339,-1.,3.83432392054804));
#48255=CARTESIAN_POINT('Ctrl Pts',(0.790865012705339,1.,3.83432392054804));
#48256=CARTESIAN_POINT('Ctrl Pts',(0.791447528662381,-1.,3.82687033899799));
#48257=CARTESIAN_POINT('Ctrl Pts',(0.791447528662381,1.,3.82687033899799));
#48258=CARTESIAN_POINT('Ctrl Pts',(0.791981740718606,-1.,3.81944345442237));
#48259=CARTESIAN_POINT('Ctrl Pts',(0.791981740718606,1.,3.81944345442237));
#48260=CARTESIAN_POINT('Ctrl Pts',(0.792462483517568,-1.,3.81202588694726));
#48261=CARTESIAN_POINT('Ctrl Pts',(0.792462483517568,1.,3.81202588694726));
#48262=CARTESIAN_POINT('Ctrl Pts',(0.792882695234692,-1.,3.80459229925598));
#48263=CARTESIAN_POINT('Ctrl Pts',(0.792882695234692,1.,3.80459229925598));
#48264=CARTESIAN_POINT('Ctrl Pts',(0.7932356129732,-1.,3.79711921389862));
#48265=CARTESIAN_POINT('Ctrl Pts',(0.7932356129732,1.,3.79711921389862));
#48266=CARTESIAN_POINT('Ctrl Pts',(0.793516871680965,-1.,3.78959439439222));
#48267=CARTESIAN_POINT('Ctrl Pts',(0.793516871680965,1.,3.78959439439222));
#48268=CARTESIAN_POINT('Ctrl Pts',(0.793726235781339,-1.,3.78202460377617));
#48269=CARTESIAN_POINT('Ctrl Pts',(0.793726235781339,1.,3.78202460377617));
#48270=CARTESIAN_POINT('Ctrl Pts',(0.793870523787515,-1.,3.77444863801264));
#48271=CARTESIAN_POINT('Ctrl Pts',(0.793870523787515,1.,3.77444863801264));
#48272=CARTESIAN_POINT('Ctrl Pts',(0.793961083689141,-1.,3.76692626931184));
#48273=CARTESIAN_POINT('Ctrl Pts',(0.793961083689141,1.,3.76692626931184));
#48274=CARTESIAN_POINT('Ctrl Pts',(0.794008429135046,-1.,3.75951468666325));
#48275=CARTESIAN_POINT('Ctrl Pts',(0.794008429135046,1.,3.75951468666325));
#48276=CARTESIAN_POINT('Ctrl Pts',(0.79401734737144,-1.,3.75224692493895));
#48277=CARTESIAN_POINT('Ctrl Pts',(0.79401734737144,1.,3.75224692493895));
#48278=CARTESIAN_POINT('Ctrl Pts',(0.79398270045988,-1.,3.74511357728827));
#48279=CARTESIAN_POINT('Ctrl Pts',(0.79398270045988,1.,3.74511357728827));
#48280=CARTESIAN_POINT('Ctrl Pts',(0.79388270093679,-1.,3.73803280541576));
#48281=CARTESIAN_POINT('Ctrl Pts',(0.79388270093679,1.,3.73803280541576));
#48282=CARTESIAN_POINT('Ctrl Pts',(0.793682750269347,-1.,3.7308691469564));
#48283=CARTESIAN_POINT('Ctrl Pts',(0.793682750269347,1.,3.7308691469564));
#48284=CARTESIAN_POINT('Ctrl Pts',(0.79334702378387,-1.,3.7234879729357));
#48285=CARTESIAN_POINT('Ctrl Pts',(0.79334702378387,1.,3.7234879729357));
#48286=CARTESIAN_POINT('Ctrl Pts',(0.792848377370115,-1.,3.7158024239604));
#48287=CARTESIAN_POINT('Ctrl Pts',(0.792848377370115,1.,3.7158024239604));
#48288=CARTESIAN_POINT('Ctrl Pts',(0.792177688845967,-1.,3.70781724021879));
#48289=CARTESIAN_POINT('Ctrl Pts',(0.792177688845967,1.,3.70781724021879));
#48290=CARTESIAN_POINT('Ctrl Pts',(0.791356575696508,-1.,3.69968940808982));
#48291=CARTESIAN_POINT('Ctrl Pts',(0.791356575696508,1.,3.69968940808982));
#48292=CARTESIAN_POINT('Ctrl Pts',(0.790436284989579,-1.,3.69172044327754));
#48293=CARTESIAN_POINT('Ctrl Pts',(0.790436284989579,1.,3.69172044327754));
#48294=CARTESIAN_POINT('Ctrl Pts',(0.789483546065158,-1.,3.68428439784285));
#48295=CARTESIAN_POINT('Ctrl Pts',(0.789483546065158,1.,3.68428439784285));
#48296=CARTESIAN_POINT('Ctrl Pts',(0.788569566220662,-1.,3.67777119516438));
#48297=CARTESIAN_POINT('Ctrl Pts',(0.788569566220662,1.,3.67777119516438));
#48298=CARTESIAN_POINT('Ctrl Pts',(0.787758799995426,-1.,3.672529236635));
#48299=CARTESIAN_POINT('Ctrl Pts',(0.787758799995426,1.,3.672529236635));
#48300=CARTESIAN_POINT('Ctrl Pts',(0.787095252589507,-1.,3.66879484800625));
#48301=CARTESIAN_POINT('Ctrl Pts',(0.787095252589507,1.,3.66879484800625));
#48302=CARTESIAN_POINT('Ctrl Pts',(0.786698783541657,-1.,3.66710211819938));
#48303=CARTESIAN_POINT('Ctrl Pts',(0.786698783541657,1.,3.66710211819938));
#48304=CARTESIAN_POINT('Ctrl Pts',(0.786480236184947,-1.,3.66657784454965));
#48305=CARTESIAN_POINT('Ctrl Pts',(0.786480236184947,1.,3.66657784454965));
#48306=CARTESIAN_POINT('Ctrl Pts',(0.786369528183039,-1.,3.66655932661846));
#48307=CARTESIAN_POINT('Ctrl Pts',(0.786369528183039,1.,3.66655932661846));
#48308=CARTESIAN_POINT('Ctrl Pts',(0.786322922920599,-1.,3.66663282329846));
#48309=CARTESIAN_POINT('Ctrl Pts',(0.786322922920599,1.,3.66663282329846));
#48310=CARTESIAN_POINT('',(0.732042837400619,1.,4.13571194405636));
#48311=CARTESIAN_POINT('Ctrl Pts',(0.732042837400619,1.,4.13571194405636));
#48312=CARTESIAN_POINT('Ctrl Pts',(0.732488575135925,1.,4.13420383737278));
#48313=CARTESIAN_POINT('Ctrl Pts',(0.733376589325634,1.,4.13118752796397));
#48314=CARTESIAN_POINT('Ctrl Pts',(0.734698226767512,1.,4.12666277572794));
#48315=CARTESIAN_POINT('Ctrl Pts',(0.736439634335347,1.,4.12062919626082));
#48316=CARTESIAN_POINT('Ctrl Pts',(0.738581708229118,1.,4.11308626953795));
#48317=CARTESIAN_POINT('Ctrl Pts',(0.740688998555151,1.,4.1055424175856));
#48318=CARTESIAN_POINT('Ctrl Pts',(0.742761369690017,1.,4.09799769702712));
#48319=CARTESIAN_POINT('Ctrl Pts',(0.744798649705513,1.,4.09045220253011));
#48320=CARTESIAN_POINT('Ctrl Pts',(0.746800631490821,1.,4.08290608094789));
#48321=CARTESIAN_POINT('Ctrl Pts',(0.748767076679176,1.,4.07535951055363));
#48322=CARTESIAN_POINT('Ctrl Pts',(0.750697720483175,1.,4.06781267241886));
#48323=CARTESIAN_POINT('Ctrl Pts',(0.752592276482868,1.,4.06026572221399));
#48324=CARTESIAN_POINT('Ctrl Pts',(0.754450441816411,1.,4.05271876688106));
#48325=CARTESIAN_POINT('Ctrl Pts',(0.756271902370186,1.,4.04517182654344));
#48326=CARTESIAN_POINT('Ctrl Pts',(0.758056338885553,1.,4.03762485803468));
#48327=CARTESIAN_POINT('Ctrl Pts',(0.759803433244165,1.,4.0300778195465));
#48328=CARTESIAN_POINT('Ctrl Pts',(0.761512875859941,1.,4.02253072741347));
#48329=CARTESIAN_POINT('Ctrl Pts',(0.763184371182826,1.,4.01498370680434));
#48330=CARTESIAN_POINT('Ctrl Pts',(0.764817648784946,1.,4.00743706791366));
#48331=CARTESIAN_POINT('Ctrl Pts',(0.766412457135785,1.,3.99989129179464));
#48332=CARTESIAN_POINT('Ctrl Pts',(0.767968531377707,1.,3.99234687880892));
#48333=CARTESIAN_POINT('Ctrl Pts',(0.769485566245459,1.,3.98480422348403));
#48334=CARTESIAN_POINT('Ctrl Pts',(0.770963190030503,1.,3.97726349165507));
#48335=CARTESIAN_POINT('Ctrl Pts',(0.772400931772238,1.,3.96972446532832));
#48336=CARTESIAN_POINT('Ctrl Pts',(0.773798212026682,1.,3.96218649639876));
#48337=CARTESIAN_POINT('Ctrl Pts',(0.775154418039441,1.,3.95464885452364));
#48338=CARTESIAN_POINT('Ctrl Pts',(0.776468966697959,1.,3.94711101619471));
#48339=CARTESIAN_POINT('Ctrl Pts',(0.777741370568549,1.,3.93957296768098));
#48340=CARTESIAN_POINT('Ctrl Pts',(0.778971308134786,1.,3.93203552473153));
#48341=CARTESIAN_POINT('Ctrl Pts',(0.780158678615506,1.,3.92450058323799));
#48342=CARTESIAN_POINT('Ctrl Pts',(0.781303428618343,1.,3.9169703605466));
#48343=CARTESIAN_POINT('Ctrl Pts',(0.782405395622758,1.,3.90944671004536));
#48344=CARTESIAN_POINT('Ctrl Pts',(0.783464141529082,1.,3.90193039043971));
#48345=CARTESIAN_POINT('Ctrl Pts',(0.784478799358335,1.,3.89442039235105));
#48346=CARTESIAN_POINT('Ctrl Pts',(0.785447890340723,1.,3.88691313167399));
#48347=CARTESIAN_POINT('Ctrl Pts',(0.786369675812591,1.,3.87940402818186));
#48348=CARTESIAN_POINT('Ctrl Pts',(0.78724252761798,1.,3.87188916600905));
#48349=CARTESIAN_POINT('Ctrl Pts',(0.78806531509377,1.,3.86436702561342));
#48350=CARTESIAN_POINT('Ctrl Pts',(0.788837734090688,1.,3.85683995872536));
#48351=CARTESIAN_POINT('Ctrl Pts',(0.789560798155618,1.,3.8493163780891));
#48352=CARTESIAN_POINT('Ctrl Pts',(0.790236124191289,1.,3.84180762342476));
#48353=CARTESIAN_POINT('Ctrl Pts',(0.790865012705339,1.,3.83432392054804));
#48354=CARTESIAN_POINT('Ctrl Pts',(0.791447528662381,1.,3.82687033899799));
#48355=CARTESIAN_POINT('Ctrl Pts',(0.791981740718606,1.,3.81944345442237));
#48356=CARTESIAN_POINT('Ctrl Pts',(0.792462483517568,1.,3.81202588694726));
#48357=CARTESIAN_POINT('Ctrl Pts',(0.792882695234692,1.,3.80459229925598));
#48358=CARTESIAN_POINT('Ctrl Pts',(0.7932356129732,1.,3.79711921389862));
#48359=CARTESIAN_POINT('Ctrl Pts',(0.793516871680965,1.,3.78959439439222));
#48360=CARTESIAN_POINT('Ctrl Pts',(0.793726235781339,1.,3.78202460377617));
#48361=CARTESIAN_POINT('Ctrl Pts',(0.793870523787515,1.,3.77444863801264));
#48362=CARTESIAN_POINT('Ctrl Pts',(0.793961083689141,1.,3.76692626931184));
#48363=CARTESIAN_POINT('Ctrl Pts',(0.794008429135046,1.,3.75951468666325));
#48364=CARTESIAN_POINT('Ctrl Pts',(0.79401734737144,1.,3.75224692493895));
#48365=CARTESIAN_POINT('Ctrl Pts',(0.79398270045988,1.,3.74511357728827));
#48366=CARTESIAN_POINT('Ctrl Pts',(0.79388270093679,1.,3.73803280541576));
#48367=CARTESIAN_POINT('Ctrl Pts',(0.793682750269347,1.,3.7308691469564));
#48368=CARTESIAN_POINT('Ctrl Pts',(0.79334702378387,1.,3.7234879729357));
#48369=CARTESIAN_POINT('Ctrl Pts',(0.792848377370115,1.,3.7158024239604));
#48370=CARTESIAN_POINT('Ctrl Pts',(0.792177688845967,1.,3.70781724021879));
#48371=CARTESIAN_POINT('Ctrl Pts',(0.791356575696508,1.,3.69968940808982));
#48372=CARTESIAN_POINT('Ctrl Pts',(0.790436284989579,1.,3.69172044327754));
#48373=CARTESIAN_POINT('Ctrl Pts',(0.789483546065158,1.,3.68428439784285));
#48374=CARTESIAN_POINT('Ctrl Pts',(0.788569566220662,1.,3.67777119516438));
#48375=CARTESIAN_POINT('Ctrl Pts',(0.787758799995426,1.,3.672529236635));
#48376=CARTESIAN_POINT('Ctrl Pts',(0.787145041181588,1.,3.66907505398769));
#48377=CARTESIAN_POINT('Ctrl Pts',(0.786774337198499,1.,3.66743103898844));
#48378=CARTESIAN_POINT('Ctrl Pts',(0.786565919559889,1.,3.66680946938396));
#48379=CARTESIAN_POINT('Ctrl Pts',(0.786459983896781,1.,3.66664310415236));
#48380=CARTESIAN_POINT('Ctrl Pts',(0.786422660833743,1.,3.66661143271648));
#48381=CARTESIAN_POINT('',(0.732042837400619,0.,4.13571194405636));
#48382=CARTESIAN_POINT('Ctrl Pts',(0.385214314776328,-1.,3.73016218570874));
#48383=CARTESIAN_POINT('Ctrl Pts',(0.385214314776328,1.,3.73016218570874));
#48384=CARTESIAN_POINT('Ctrl Pts',(0.385147278814803,-1.,3.73010668803185));
#48385=CARTESIAN_POINT('Ctrl Pts',(0.385147278814803,1.,3.73010668803185));
#48386=CARTESIAN_POINT('Ctrl Pts',(0.385047711603887,-1.,3.73015851028729));
#48387=CARTESIAN_POINT('Ctrl Pts',(0.385047711603887,1.,3.73015851028729));
#48388=CARTESIAN_POINT('Ctrl Pts',(0.385001870183841,-1.,3.73072465900727));
#48389=CARTESIAN_POINT('Ctrl Pts',(0.385001870183841,1.,3.73072465900727));
#48390=CARTESIAN_POINT('Ctrl Pts',(0.385147887989514,-1.,3.73245705639337));
#48391=CARTESIAN_POINT('Ctrl Pts',(0.385147887989514,1.,3.73245705639337));
#48392=CARTESIAN_POINT('Ctrl Pts',(0.385670806454744,-1.,3.73621371845475));
#48393=CARTESIAN_POINT('Ctrl Pts',(0.385670806454744,1.,3.73621371845475));
#48394=CARTESIAN_POINT('Ctrl Pts',(0.386519576222035,-1.,3.74144965781088));
#48395=CARTESIAN_POINT('Ctrl Pts',(0.386519576222035,1.,3.74144965781088));
#48396=CARTESIAN_POINT('Ctrl Pts',(0.387663020050396,-1.,3.74792651696269));
#48397=CARTESIAN_POINT('Ctrl Pts',(0.387663020050396,1.,3.74792651696269));
#48398=CARTESIAN_POINT('Ctrl Pts',(0.38905477589825,-1.,3.75529302894757));
#48399=CARTESIAN_POINT('Ctrl Pts',(0.38905477589825,1.,3.75529302894757));
#48400=CARTESIAN_POINT('Ctrl Pts',(0.390642072979258,-1.,3.76315635032993));
#48401=CARTESIAN_POINT('Ctrl Pts',(0.390642072979258,1.,3.76315635032993));
#48402=CARTESIAN_POINT('Ctrl Pts',(0.392372786223346,-1.,3.77114011595892));
#48403=CARTESIAN_POINT('Ctrl Pts',(0.392372786223346,1.,3.77114011595892));
#48404=CARTESIAN_POINT('Ctrl Pts',(0.394202481011595,-1.,3.77894173114368));
#48405=CARTESIAN_POINT('Ctrl Pts',(0.394202481011595,1.,3.77894173114368));
#48406=CARTESIAN_POINT('Ctrl Pts',(0.396103205335028,-1.,3.78640521279479));
#48407=CARTESIAN_POINT('Ctrl Pts',(0.396103205335028,1.,3.78640521279479));
#48408=CARTESIAN_POINT('Ctrl Pts',(0.398064818684158,-1.,3.79352887163457));
#48409=CARTESIAN_POINT('Ctrl Pts',(0.398064818684158,1.,3.79352887163457));
#48410=CARTESIAN_POINT('Ctrl Pts',(0.400088346504726,-1.,3.80040370384659));
#48411=CARTESIAN_POINT('Ctrl Pts',(0.400088346504726,1.,3.80040370384659));
#48412=CARTESIAN_POINT('Ctrl Pts',(0.402181320148474,-1.,3.80716881962763));
#48413=CARTESIAN_POINT('Ctrl Pts',(0.402181320148474,1.,3.80716881962763));
#48414=CARTESIAN_POINT('Ctrl Pts',(0.404352694628236,-1.,3.81396374287762));
#48415=CARTESIAN_POINT('Ctrl Pts',(0.404352694628236,1.,3.81396374287762));
#48416=CARTESIAN_POINT('Ctrl Pts',(0.406607038258906,-1.,3.82087303913741));
#48417=CARTESIAN_POINT('Ctrl Pts',(0.406607038258906,1.,3.82087303913741));
#48418=CARTESIAN_POINT('Ctrl Pts',(0.408942371447376,-1.,3.82790724256397));
#48419=CARTESIAN_POINT('Ctrl Pts',(0.408942371447376,1.,3.82790724256397));
#48420=CARTESIAN_POINT('Ctrl Pts',(0.411353038798459,-1.,3.83503345578645));
#48421=CARTESIAN_POINT('Ctrl Pts',(0.411353038798459,1.,3.83503345578645));
#48422=CARTESIAN_POINT('Ctrl Pts',(0.413831367016726,-1.,3.84219403994742));
#48423=CARTESIAN_POINT('Ctrl Pts',(0.413831367016726,1.,3.84219403994742));
#48424=CARTESIAN_POINT('Ctrl Pts',(0.41636967805292,-1.,3.8493286415751));
#48425=CARTESIAN_POINT('Ctrl Pts',(0.41636967805292,1.,3.8493286415751));
#48426=CARTESIAN_POINT('Ctrl Pts',(0.418962468086809,-1.,3.85639825648031));
#48427=CARTESIAN_POINT('Ctrl Pts',(0.418962468086809,1.,3.85639825648031));
#48428=CARTESIAN_POINT('Ctrl Pts',(0.421607423177575,-1.,3.86339652542749));
#48429=CARTESIAN_POINT('Ctrl Pts',(0.421607423177575,1.,3.86339652542749));
#48430=CARTESIAN_POINT('Ctrl Pts',(0.424304173195142,-1.,3.87033643487882));
#48431=CARTESIAN_POINT('Ctrl Pts',(0.424304173195142,1.,3.87033643487882));
#48432=CARTESIAN_POINT('Ctrl Pts',(0.427053541173469,-1.,3.87724240306609));
#48433=CARTESIAN_POINT('Ctrl Pts',(0.427053541173469,1.,3.87724240306609));
#48434=CARTESIAN_POINT('Ctrl Pts',(0.429856640579733,-1.,3.88414070943334));
#48435=CARTESIAN_POINT('Ctrl Pts',(0.429856640579733,1.,3.88414070943334));
#48436=CARTESIAN_POINT('Ctrl Pts',(0.432713929544439,-1.,3.89104947940592));
#48437=CARTESIAN_POINT('Ctrl Pts',(0.432713929544439,1.,3.89104947940592));
#48438=CARTESIAN_POINT('Ctrl Pts',(0.435624629433505,-1.,3.8979725665544));
#48439=CARTESIAN_POINT('Ctrl Pts',(0.435624629433505,1.,3.8979725665544));
#48440=CARTESIAN_POINT('Ctrl Pts',(0.438587235458233,-1.,3.90490512938546));
#48441=CARTESIAN_POINT('Ctrl Pts',(0.438587235458233,1.,3.90490512938546));
#48442=CARTESIAN_POINT('Ctrl Pts',(0.441599824524047,-1.,3.91183704069146));
#48443=CARTESIAN_POINT('Ctrl Pts',(0.441599824524047,1.,3.91183704069146));
#48444=CARTESIAN_POINT('Ctrl Pts',(0.444660430230592,-1.,3.91875701610721));
#48445=CARTESIAN_POINT('Ctrl Pts',(0.444660430230592,1.,3.91875701610721));
#48446=CARTESIAN_POINT('Ctrl Pts',(0.447767416837296,-1.,3.92565674143424));
#48447=CARTESIAN_POINT('Ctrl Pts',(0.447767416837296,1.,3.92565674143424));
#48448=CARTESIAN_POINT('Ctrl Pts',(0.450919768356346,-1.,3.93253407403128));
#48449=CARTESIAN_POINT('Ctrl Pts',(0.450919768356346,1.,3.93253407403128));
#48450=CARTESIAN_POINT('Ctrl Pts',(0.454116879027575,-1.,3.93939080846298));
#48451=CARTESIAN_POINT('Ctrl Pts',(0.454116879027575,1.,3.93939080846298));
#48452=CARTESIAN_POINT('Ctrl Pts',(0.457358410451673,-1.,3.94623117206675));
#48453=CARTESIAN_POINT('Ctrl Pts',(0.457358410451673,1.,3.94623117206675));
#48454=CARTESIAN_POINT('Ctrl Pts',(0.460644124429119,-1.,3.95306005817363));
#48455=CARTESIAN_POINT('Ctrl Pts',(0.460644124429119,1.,3.95306005817363));
#48456=CARTESIAN_POINT('Ctrl Pts',(0.463973722115744,-1.,3.95988133243543));
#48457=CARTESIAN_POINT('Ctrl Pts',(0.463973722115744,1.,3.95988133243543));
#48458=CARTESIAN_POINT('Ctrl Pts',(0.467346690880671,-1.,3.96669622273946));
#48459=CARTESIAN_POINT('Ctrl Pts',(0.467346690880671,1.,3.96669622273946));
#48460=CARTESIAN_POINT('Ctrl Pts',(0.470762379613477,-1.,3.97350414289415));
#48461=CARTESIAN_POINT('Ctrl Pts',(0.470762379613477,1.,3.97350414289415));
#48462=CARTESIAN_POINT('Ctrl Pts',(0.474220061019542,-1.,3.9803033804443));
#48463=CARTESIAN_POINT('Ctrl Pts',(0.474220061019542,1.,3.9803033804443));
#48464=CARTESIAN_POINT('Ctrl Pts',(0.477718999122033,-1.,3.98709184306743));
#48465=CARTESIAN_POINT('Ctrl Pts',(0.477718999122033,1.,3.98709184306743));
#48466=CARTESIAN_POINT('Ctrl Pts',(0.481258512209637,-1.,3.99386775880655));
#48467=CARTESIAN_POINT('Ctrl Pts',(0.481258512209637,1.,3.99386775880655));
#48468=CARTESIAN_POINT('Ctrl Pts',(0.484838042421754,-1.,4.00063045119234));
#48469=CARTESIAN_POINT('Ctrl Pts',(0.484838042421754,1.,4.00063045119234));
#48470=CARTESIAN_POINT('Ctrl Pts',(0.48845713042453,-1.,4.0073800839092));
#48471=CARTESIAN_POINT('Ctrl Pts',(0.48845713042453,1.,4.0073800839092));
#48472=CARTESIAN_POINT('Ctrl Pts',(0.49211538341793,-1.,4.01411733503486));
#48473=CARTESIAN_POINT('Ctrl Pts',(0.49211538341793,1.,4.01411733503486));
#48474=CARTESIAN_POINT('Ctrl Pts',(0.495812444326222,-1.,4.02084308851813));
#48475=CARTESIAN_POINT('Ctrl Pts',(0.495812444326222,1.,4.02084308851813));
#48476=CARTESIAN_POINT('Ctrl Pts',(0.499547962340889,-1.,4.0275581398015));
#48477=CARTESIAN_POINT('Ctrl Pts',(0.499547962340889,1.,4.0275581398015));
#48478=CARTESIAN_POINT('Ctrl Pts',(0.503321556915513,-1.,4.0342628417439));
#48479=CARTESIAN_POINT('Ctrl Pts',(0.503321556915513,1.,4.0342628417439));
#48480=CARTESIAN_POINT('Ctrl Pts',(0.507132823288361,-1.,4.04095715149074));
#48481=CARTESIAN_POINT('Ctrl Pts',(0.507132823288361,1.,4.04095715149074));
#48482=CARTESIAN_POINT('Ctrl Pts',(0.510981349219173,-1.,4.04764078815591));
#48483=CARTESIAN_POINT('Ctrl Pts',(0.510981349219173,1.,4.04764078815591));
#48484=CARTESIAN_POINT('Ctrl Pts',(0.514866728193103,-1.,4.05431335771261));
#48485=CARTESIAN_POINT('Ctrl Pts',(0.514866728193103,1.,4.05431335771261));
#48486=CARTESIAN_POINT('Ctrl Pts',(0.518788572336809,-1.,4.06097448037934));
#48487=CARTESIAN_POINT('Ctrl Pts',(0.518788572336809,1.,4.06097448037934));
#48488=CARTESIAN_POINT('Ctrl Pts',(0.522746528602767,-1.,4.06762394471075));
#48489=CARTESIAN_POINT('Ctrl Pts',(0.522746528602767,1.,4.06762394471075));
#48490=CARTESIAN_POINT('Ctrl Pts',(0.526740277226999,-1.,4.07426172299496));
#48491=CARTESIAN_POINT('Ctrl Pts',(0.526740277226999,1.,4.07426172299496));
#48492=CARTESIAN_POINT('Ctrl Pts',(0.530769518728075,-1.,4.08088789536488));
#48493=CARTESIAN_POINT('Ctrl Pts',(0.530769518728075,1.,4.08088789536488));
#48494=CARTESIAN_POINT('Ctrl Pts',(0.534833963476999,-1.,4.08750259988693));
#48495=CARTESIAN_POINT('Ctrl Pts',(0.534833963476999,1.,4.08750259988693));
#48496=CARTESIAN_POINT('Ctrl Pts',(0.53893332117992,-1.,4.09410597627116));
#48497=CARTESIAN_POINT('Ctrl Pts',(0.53893332117992,1.,4.09410597627116));
#48498=CARTESIAN_POINT('Ctrl Pts',(0.543067286878457,-1.,4.10069810244473));
#48499=CARTESIAN_POINT('Ctrl Pts',(0.543067286878457,1.,4.10069810244473));
#48500=CARTESIAN_POINT('Ctrl Pts',(0.547235539486759,-1.,4.1072789702877));
#48501=CARTESIAN_POINT('Ctrl Pts',(0.547235539486759,1.,4.1072789702877));
#48502=CARTESIAN_POINT('Ctrl Pts',(0.551437758498246,-1.,4.11384852025578));
#48503=CARTESIAN_POINT('Ctrl Pts',(0.551437758498246,1.,4.11384852025578));
#48504=CARTESIAN_POINT('Ctrl Pts',(0.555673636130778,-1.,4.1204066619623));
#48505=CARTESIAN_POINT('Ctrl Pts',(0.555673636130778,1.,4.1204066619623));
#48506=CARTESIAN_POINT('Ctrl Pts',(0.559942890594628,-1.,4.12695329951859));
#48507=CARTESIAN_POINT('Ctrl Pts',(0.559942890594628,1.,4.12695329951859));
#48508=CARTESIAN_POINT('Ctrl Pts',(0.564245279535705,-1.,4.13348835726086));
#48509=CARTESIAN_POINT('Ctrl Pts',(0.564245279535705,1.,4.13348835726086));
#48510=CARTESIAN_POINT('Ctrl Pts',(0.568580610187115,-1.,4.14001179828669));
#48511=CARTESIAN_POINT('Ctrl Pts',(0.568580610187115,1.,4.14001179828669));
#48512=CARTESIAN_POINT('Ctrl Pts',(0.572948736066276,-1.,4.14652361065787));
#48513=CARTESIAN_POINT('Ctrl Pts',(0.572948736066276,1.,4.14652361065787));
#48514=CARTESIAN_POINT('Ctrl Pts',(0.576469391673916,-1.,4.1517237611974));
#48515=CARTESIAN_POINT('Ctrl Pts',(0.576469391673916,1.,4.1517237611974));
#48516=CARTESIAN_POINT('Ctrl Pts',(0.579124568912543,-1.,4.15561864787379));
#48517=CARTESIAN_POINT('Ctrl Pts',(0.579124568912543,1.,4.15561864787379));
#48518=CARTESIAN_POINT('Ctrl Pts',(0.580901211462913,-1.,4.15821291712391));
#48519=CARTESIAN_POINT('Ctrl Pts',(0.580901211462913,1.,4.15821291712391));
#48520=CARTESIAN_POINT('Ctrl Pts',(0.581791163835814,-1.,4.15950947128175));
#48521=CARTESIAN_POINT('Ctrl Pts',(0.581791163835814,1.,4.15950947128175));
#48522=CARTESIAN_POINT('',(0.385112848332548,1.,3.73017266276632));
#48523=CARTESIAN_POINT('Ctrl Pts',(0.385112848332548,-1.,3.73017266276632));
#48524=CARTESIAN_POINT('Ctrl Pts',(0.385112848332548,-0.666666666666667,
3.73017266276632));
#48525=CARTESIAN_POINT('Ctrl Pts',(0.385112848332548,-0.333333333333333,
3.73017266276632));
#48526=CARTESIAN_POINT('Ctrl Pts',(0.385112848332548,0.333333333333333,
3.73017266276632));
#48527=CARTESIAN_POINT('Ctrl Pts',(0.385112848332548,0.666666666666667,
3.73017266276632));
#48528=CARTESIAN_POINT('Ctrl Pts',(0.385112848332548,1.,3.73017266276632));
#48529=CARTESIAN_POINT('',(0.581791163835814,1.,4.15950947128175));
#48530=CARTESIAN_POINT('',(0.581791163835814,0.,4.15950947128175));
#48531=CARTESIAN_POINT('Ctrl Pts',(0.385112848332549,1.,3.73017266276632));
#48532=CARTESIAN_POINT('Ctrl Pts',(0.385087139001608,1.,3.73021431755218));
#48533=CARTESIAN_POINT('Ctrl Pts',(0.385037797882046,1.,3.73040527620929));
#48534=CARTESIAN_POINT('Ctrl Pts',(0.385031656499141,1.,3.731060828624));
#48535=CARTESIAN_POINT('Ctrl Pts',(0.385187124633964,1.,3.73273893363318));
#48536=CARTESIAN_POINT('Ctrl Pts',(0.385670806454744,1.,3.73621371845475));
#48537=CARTESIAN_POINT('Ctrl Pts',(0.386519576222035,1.,3.74144965781088));
#48538=CARTESIAN_POINT('Ctrl Pts',(0.387663020050396,1.,3.74792651696269));
#48539=CARTESIAN_POINT('Ctrl Pts',(0.38905477589825,1.,3.75529302894757));
#48540=CARTESIAN_POINT('Ctrl Pts',(0.390642072979258,1.,3.76315635032993));
#48541=CARTESIAN_POINT('Ctrl Pts',(0.392372786223346,1.,3.77114011595892));
#48542=CARTESIAN_POINT('Ctrl Pts',(0.394202481011595,1.,3.77894173114368));
#48543=CARTESIAN_POINT('Ctrl Pts',(0.396103205335028,1.,3.78640521279479));
#48544=CARTESIAN_POINT('Ctrl Pts',(0.398064818684158,1.,3.79352887163457));
#48545=CARTESIAN_POINT('Ctrl Pts',(0.400088346504726,1.,3.80040370384659));
#48546=CARTESIAN_POINT('Ctrl Pts',(0.402181320148474,1.,3.80716881962763));
#48547=CARTESIAN_POINT('Ctrl Pts',(0.404352694628236,1.,3.81396374287762));
#48548=CARTESIAN_POINT('Ctrl Pts',(0.406607038258906,1.,3.82087303913741));
#48549=CARTESIAN_POINT('Ctrl Pts',(0.408942371447376,1.,3.82790724256397));
#48550=CARTESIAN_POINT('Ctrl Pts',(0.411353038798459,1.,3.83503345578645));
#48551=CARTESIAN_POINT('Ctrl Pts',(0.413831367016726,1.,3.84219403994742));
#48552=CARTESIAN_POINT('Ctrl Pts',(0.41636967805292,1.,3.8493286415751));
#48553=CARTESIAN_POINT('Ctrl Pts',(0.418962468086809,1.,3.85639825648031));
#48554=CARTESIAN_POINT('Ctrl Pts',(0.421607423177575,1.,3.86339652542749));
#48555=CARTESIAN_POINT('Ctrl Pts',(0.424304173195142,1.,3.87033643487882));
#48556=CARTESIAN_POINT('Ctrl Pts',(0.427053541173469,1.,3.87724240306609));
#48557=CARTESIAN_POINT('Ctrl Pts',(0.429856640579733,1.,3.88414070943334));
#48558=CARTESIAN_POINT('Ctrl Pts',(0.432713929544439,1.,3.89104947940592));
#48559=CARTESIAN_POINT('Ctrl Pts',(0.435624629433505,1.,3.8979725665544));
#48560=CARTESIAN_POINT('Ctrl Pts',(0.438587235458233,1.,3.90490512938546));
#48561=CARTESIAN_POINT('Ctrl Pts',(0.441599824524047,1.,3.91183704069146));
#48562=CARTESIAN_POINT('Ctrl Pts',(0.444660430230592,1.,3.91875701610721));
#48563=CARTESIAN_POINT('Ctrl Pts',(0.447767416837296,1.,3.92565674143424));
#48564=CARTESIAN_POINT('Ctrl Pts',(0.450919768356346,1.,3.93253407403128));
#48565=CARTESIAN_POINT('Ctrl Pts',(0.454116879027575,1.,3.93939080846298));
#48566=CARTESIAN_POINT('Ctrl Pts',(0.457358410451673,1.,3.94623117206675));
#48567=CARTESIAN_POINT('Ctrl Pts',(0.460644124429119,1.,3.95306005817363));
#48568=CARTESIAN_POINT('Ctrl Pts',(0.463973722115744,1.,3.95988133243543));
#48569=CARTESIAN_POINT('Ctrl Pts',(0.467346690880671,1.,3.96669622273946));
#48570=CARTESIAN_POINT('Ctrl Pts',(0.470762379613477,1.,3.97350414289415));
#48571=CARTESIAN_POINT('Ctrl Pts',(0.474220061019542,1.,3.9803033804443));
#48572=CARTESIAN_POINT('Ctrl Pts',(0.477718999122033,1.,3.98709184306743));
#48573=CARTESIAN_POINT('Ctrl Pts',(0.481258512209637,1.,3.99386775880655));
#48574=CARTESIAN_POINT('Ctrl Pts',(0.484838042421754,1.,4.00063045119234));
#48575=CARTESIAN_POINT('Ctrl Pts',(0.48845713042453,1.,4.0073800839092));
#48576=CARTESIAN_POINT('Ctrl Pts',(0.49211538341793,1.,4.01411733503486));
#48577=CARTESIAN_POINT('Ctrl Pts',(0.495812444326222,1.,4.02084308851813));
#48578=CARTESIAN_POINT('Ctrl Pts',(0.499547962340889,1.,4.0275581398015));
#48579=CARTESIAN_POINT('Ctrl Pts',(0.503321556915513,1.,4.0342628417439));
#48580=CARTESIAN_POINT('Ctrl Pts',(0.507132823288361,1.,4.04095715149074));
#48581=CARTESIAN_POINT('Ctrl Pts',(0.510981349219173,1.,4.04764078815591));
#48582=CARTESIAN_POINT('Ctrl Pts',(0.514866728193103,1.,4.05431335771261));
#48583=CARTESIAN_POINT('Ctrl Pts',(0.518788572336809,1.,4.06097448037934));
#48584=CARTESIAN_POINT('Ctrl Pts',(0.522746528602767,1.,4.06762394471075));
#48585=CARTESIAN_POINT('Ctrl Pts',(0.526740277226999,1.,4.07426172299496));
#48586=CARTESIAN_POINT('Ctrl Pts',(0.530769518728075,1.,4.08088789536488));
#48587=CARTESIAN_POINT('Ctrl Pts',(0.534833963476999,1.,4.08750259988693));
#48588=CARTESIAN_POINT('Ctrl Pts',(0.53893332117992,1.,4.09410597627116));
#48589=CARTESIAN_POINT('Ctrl Pts',(0.543067286878457,1.,4.10069810244473));
#48590=CARTESIAN_POINT('Ctrl Pts',(0.547235539486759,1.,4.1072789702877));
#48591=CARTESIAN_POINT('Ctrl Pts',(0.551437758498246,1.,4.11384852025578));
#48592=CARTESIAN_POINT('Ctrl Pts',(0.555673636130778,1.,4.1204066619623));
#48593=CARTESIAN_POINT('Ctrl Pts',(0.559942890594628,1.,4.12695329951859));
#48594=CARTESIAN_POINT('Ctrl Pts',(0.564245279535705,1.,4.13348835726086));
#48595=CARTESIAN_POINT('Ctrl Pts',(0.568580610187115,1.,4.14001179828669));
#48596=CARTESIAN_POINT('Ctrl Pts',(0.572948736066276,1.,4.14652361065787));
#48597=CARTESIAN_POINT('Ctrl Pts',(0.576469391673916,1.,4.1517237611974));
#48598=CARTESIAN_POINT('Ctrl Pts',(0.579124568912543,1.,4.15561864787379));
#48599=CARTESIAN_POINT('Ctrl Pts',(0.580901211462913,1.,4.15821291712391));
#48600=CARTESIAN_POINT('Ctrl Pts',(0.581791163835814,1.,4.15950947128175));
#48601=CARTESIAN_POINT('Origin',(0.581791163835814,0.,4.15950947128175));
#48602=CARTESIAN_POINT('',(0.732042837400619,1.,4.13571194405636));
#48603=CARTESIAN_POINT('Origin',(0.,0.,0.));
#48604=CARTESIAN_POINT('',(0.203156094897895,1.,3.74449296982994));
#48605=CARTESIAN_POINT('Origin',(0.,1.,0.));
#48606=CARTESIAN_POINT('Ctrl Pts',(0.203156094897895,1.,3.74449296982994));
#48607=CARTESIAN_POINT('Ctrl Pts',(0.203156094897895,0.666666666666667,
3.74449296982994));
#48608=CARTESIAN_POINT('Ctrl Pts',(0.203156094897895,0.333333333333333,
3.74449296982994));
#48609=CARTESIAN_POINT('Ctrl Pts',(0.203156094897895,-0.333333333333333,
3.74449296982994));
#48610=CARTESIAN_POINT('Ctrl Pts',(0.203156094897895,-0.666666666666667,
3.74449296982994));
#48611=CARTESIAN_POINT('Ctrl Pts',(0.203156094897895,-1.,3.74449296982994));
#48612=CARTESIAN_POINT('Ctrl Pts',(0.0760622897878233,-1.,4.19931119685982));
#48613=CARTESIAN_POINT('Ctrl Pts',(0.0760622897878233,1.,4.19931119685982));
#48614=CARTESIAN_POINT('Ctrl Pts',(0.0767384596142192,-1.,4.19789138621624));
#48615=CARTESIAN_POINT('Ctrl Pts',(0.0767384596142192,1.,4.19789138621624));
#48616=CARTESIAN_POINT('Ctrl Pts',(0.0780873956244399,-1.,4.19505112860624));
#48617=CARTESIAN_POINT('Ctrl Pts',(0.0780873956244399,1.,4.19505112860624));
#48618=CARTESIAN_POINT('Ctrl Pts',(0.08010058871176,-1.,4.19078883322483));
#48619=CARTESIAN_POINT('Ctrl Pts',(0.08010058871176,1.,4.19078883322483));
#48620=CARTESIAN_POINT('Ctrl Pts',(0.0827644164389507,-1.,4.1851019532944));
#48621=CARTESIAN_POINT('Ctrl Pts',(0.0827644164389507,1.,4.1851019532944));
#48622=CARTESIAN_POINT('Ctrl Pts',(0.0860600915552512,-1.,4.17798698669991));
#48623=CARTESIAN_POINT('Ctrl Pts',(0.0860600915552512,1.,4.17798698669991));
#48624=CARTESIAN_POINT('Ctrl Pts',(0.0893215560850325,-1.,4.17086566491823));
#48625=CARTESIAN_POINT('Ctrl Pts',(0.0893215560850325,1.,4.17086566491823));
#48626=CARTESIAN_POINT('Ctrl Pts',(0.0925486672167687,-1.,4.16373802265942));
#48627=CARTESIAN_POINT('Ctrl Pts',(0.0925486672167687,1.,4.16373802265942));
#48628=CARTESIAN_POINT('Ctrl Pts',(0.0957412403297065,-1.,4.15660412653006));
#48629=CARTESIAN_POINT('Ctrl Pts',(0.0957412403297065,1.,4.15660412653006));
#48630=CARTESIAN_POINT('Ctrl Pts',(0.0988990478899809,-1.,4.1494640891762));
#48631=CARTESIAN_POINT('Ctrl Pts',(0.0988990478899809,1.,4.1494640891762));
#48632=CARTESIAN_POINT('Ctrl Pts',(0.102021826577453,-1.,4.14231804938737));
#48633=CARTESIAN_POINT('Ctrl Pts',(0.102021826577453,1.,4.14231804938737));
#48634=CARTESIAN_POINT('Ctrl Pts',(0.105109286538864,-1.,4.13516614458396));
#48635=CARTESIAN_POINT('Ctrl Pts',(0.105109286538864,1.,4.13516614458396));
#48636=CARTESIAN_POINT('Ctrl Pts',(0.10816112052835,-1.,4.12800848371386));
#48637=CARTESIAN_POINT('Ctrl Pts',(0.10816112052835,1.,4.12800848371386));
#48638=CARTESIAN_POINT('Ctrl Pts',(0.111177012683377,-1.,4.12084512502444));
#48639=CARTESIAN_POINT('Ctrl Pts',(0.111177012683377,1.,4.12084512502444));
#48640=CARTESIAN_POINT('Ctrl Pts',(0.114156649609601,-1.,4.11367603925313));
#48641=CARTESIAN_POINT('Ctrl Pts',(0.114156649609601,1.,4.11367603925313));
#48642=CARTESIAN_POINT('Ctrl Pts',(0.117099722731704,-1.,4.10650113382187));
#48643=CARTESIAN_POINT('Ctrl Pts',(0.117099722731704,1.,4.10650113382187));
#48644=CARTESIAN_POINT('Ctrl Pts',(0.120005924388162,-1.,4.09932031767243));
#48645=CARTESIAN_POINT('Ctrl Pts',(0.120005924388162,1.,4.09932031767243));
#48646=CARTESIAN_POINT('Ctrl Pts',(0.122874946249119,-1.,4.09213355850836));
#48647=CARTESIAN_POINT('Ctrl Pts',(0.122874946249119,1.,4.09213355850836));
#48648=CARTESIAN_POINT('Ctrl Pts',(0.125706476822529,-1.,4.08494093372315));
#48649=CARTESIAN_POINT('Ctrl Pts',(0.125706476822529,1.,4.08494093372315));
#48650=CARTESIAN_POINT('Ctrl Pts',(0.128500200484813,-1.,4.07774270738809));
#48651=CARTESIAN_POINT('Ctrl Pts',(0.128500200484813,1.,4.07774270738809));
#48652=CARTESIAN_POINT('Ctrl Pts',(0.131255793548914,-1.,4.07053931528579));
#48653=CARTESIAN_POINT('Ctrl Pts',(0.131255793548914,1.,4.07053931528579));
#48654=CARTESIAN_POINT('Ctrl Pts',(0.133972916144225,-1.,4.06333121018476));
#48655=CARTESIAN_POINT('Ctrl Pts',(0.133972916144225,1.,4.06333121018476));
#48656=CARTESIAN_POINT('Ctrl Pts',(0.136651205046111,-1.,4.05611873400122));
#48657=CARTESIAN_POINT('Ctrl Pts',(0.136651205046111,1.,4.05611873400122));
#48658=CARTESIAN_POINT('Ctrl Pts',(0.139290267180059,-1.,4.04890199238056));
#48659=CARTESIAN_POINT('Ctrl Pts',(0.139290267180059,1.,4.04890199238056));
#48660=CARTESIAN_POINT('Ctrl Pts',(0.141889671485507,-1.,4.04168069633842));
#48661=CARTESIAN_POINT('Ctrl Pts',(0.141889671485507,1.,4.04168069633842));
#48662=CARTESIAN_POINT('Ctrl Pts',(0.144448947038352,-1.,4.03445411510403));
#48663=CARTESIAN_POINT('Ctrl Pts',(0.144448947038352,1.,4.03445411510403));
#48664=CARTESIAN_POINT('Ctrl Pts',(0.146967602878998,-1.,4.02722143147048));
#48665=CARTESIAN_POINT('Ctrl Pts',(0.146967602878998,1.,4.02722143147048));
#48666=CARTESIAN_POINT('Ctrl Pts',(0.149445144968707,-1.,4.01998203715588));
#48667=CARTESIAN_POINT('Ctrl Pts',(0.149445144968707,1.,4.01998203715588));
#48668=CARTESIAN_POINT('Ctrl Pts',(0.151881094022909,-1.,4.01273584234684));
#48669=CARTESIAN_POINT('Ctrl Pts',(0.151881094022909,1.,4.01273584234684));
#48670=CARTESIAN_POINT('Ctrl Pts',(0.154275004872309,-1.,4.00548360245297));
#48671=CARTESIAN_POINT('Ctrl Pts',(0.154275004872309,1.,4.00548360245297));
#48672=CARTESIAN_POINT('Ctrl Pts',(0.156626481393735,-1.,3.99822717425869));
#48673=CARTESIAN_POINT('Ctrl Pts',(0.156626481393735,1.,3.99822717425869));
#48674=CARTESIAN_POINT('Ctrl Pts',(0.158935123982796,-1.,3.99096873945862));
#48675=CARTESIAN_POINT('Ctrl Pts',(0.158935123982796,1.,3.99096873945862));
#48676=CARTESIAN_POINT('Ctrl Pts',(0.161200482186087,-1.,3.98371010319866));
#48677=CARTESIAN_POINT('Ctrl Pts',(0.161200482186087,1.,3.98371010319866));
#48678=CARTESIAN_POINT('Ctrl Pts',(0.163422004609998,-1.,3.97645194630944));
#48679=CARTESIAN_POINT('Ctrl Pts',(0.163422004609998,1.,3.97645194630944));
#48680=CARTESIAN_POINT('Ctrl Pts',(0.165598992851097,-1.,3.9691931362141));
#48681=CARTESIAN_POINT('Ctrl Pts',(0.165598992851097,1.,3.9691931362141));
#48682=CARTESIAN_POINT('Ctrl Pts',(0.167730547023312,-1.,3.96192990160296));
#48683=CARTESIAN_POINT('Ctrl Pts',(0.167730547023312,1.,3.96192990160296));
#48684=CARTESIAN_POINT('Ctrl Pts',(0.16981566637413,-1.,3.95465744665263));
#48685=CARTESIAN_POINT('Ctrl Pts',(0.16981566637413,1.,3.95465744665263));
#48686=CARTESIAN_POINT('Ctrl Pts',(0.171853355369232,-1.,3.94737164900861));
#48687=CARTESIAN_POINT('Ctrl Pts',(0.171853355369232,1.,3.94737164900861));
#48688=CARTESIAN_POINT('Ctrl Pts',(0.173842734974607,-1.,3.94007083096214));
#48689=CARTESIAN_POINT('Ctrl Pts',(0.173842734974607,1.,3.94007083096214));
#48690=CARTESIAN_POINT('Ctrl Pts',(0.175783136893872,-1.,3.93275726771049));
#48691=CARTESIAN_POINT('Ctrl Pts',(0.175783136893872,1.,3.93275726771049));
#48692=CARTESIAN_POINT('Ctrl Pts',(0.177674246152328,-1.,3.92543942697672));
#48693=CARTESIAN_POINT('Ctrl Pts',(0.177674246152328,1.,3.92543942697672));
#48694=CARTESIAN_POINT('Ctrl Pts',(0.179515885822894,-1.,3.91812876180948));
#48695=CARTESIAN_POINT('Ctrl Pts',(0.179515885822894,1.,3.91812876180948));
#48696=CARTESIAN_POINT('Ctrl Pts',(0.181307740731795,-1.,3.91083557557193));
#48697=CARTESIAN_POINT('Ctrl Pts',(0.181307740731795,1.,3.91083557557193));
#48698=CARTESIAN_POINT('Ctrl Pts',(0.183049081993193,-1.,3.90356488555138));
#48699=CARTESIAN_POINT('Ctrl Pts',(0.183049081993193,1.,3.90356488555138));
#48700=CARTESIAN_POINT('Ctrl Pts',(0.184738537728034,-1.,3.89631300742633));
#48701=CARTESIAN_POINT('Ctrl Pts',(0.184738537728034,1.,3.89631300742633));
#48702=CARTESIAN_POINT('Ctrl Pts',(0.186373724985263,-1.,3.88906196725817));
#48703=CARTESIAN_POINT('Ctrl Pts',(0.186373724985263,1.,3.88906196725817));
#48704=CARTESIAN_POINT('Ctrl Pts',(0.187951632512663,-1.,3.88178563496187));
#48705=CARTESIAN_POINT('Ctrl Pts',(0.187951632512663,1.,3.88178563496187));
#48706=CARTESIAN_POINT('Ctrl Pts',(0.189469253358254,-1.,3.87445976418377));
#48707=CARTESIAN_POINT('Ctrl Pts',(0.189469253358254,1.,3.87445976418377));
#48708=CARTESIAN_POINT('Ctrl Pts',(0.190924190418612,-1.,3.8670715862477));
#48709=CARTESIAN_POINT('Ctrl Pts',(0.190924190418612,1.,3.8670715862477));
#48710=CARTESIAN_POINT('Ctrl Pts',(0.192315153044979,-1.,3.85962774407652));
#48711=CARTESIAN_POINT('Ctrl Pts',(0.192315153044979,1.,3.85962774407652));
#48712=CARTESIAN_POINT('Ctrl Pts',(0.193642806777747,-1.,3.85216762264019));
#48713=CARTESIAN_POINT('Ctrl Pts',(0.193642806777747,1.,3.85216762264019));
#48714=CARTESIAN_POINT('Ctrl Pts',(0.194909009460254,-1.,3.84475203347052));
#48715=CARTESIAN_POINT('Ctrl Pts',(0.194909009460254,1.,3.84475203347052));
#48716=CARTESIAN_POINT('Ctrl Pts',(0.196115198971889,-1.,3.83743910616265));
#48717=CARTESIAN_POINT('Ctrl Pts',(0.196115198971889,1.,3.83743910616265));
#48718=CARTESIAN_POINT('Ctrl Pts',(0.197260935827375,-1.,3.83026221776488));
#48719=CARTESIAN_POINT('Ctrl Pts',(0.197260935827375,1.,3.83026221776488));
#48720=CARTESIAN_POINT('Ctrl Pts',(0.198342616900469,-1.,3.82321127348981));
#48721=CARTESIAN_POINT('Ctrl Pts',(0.198342616900469,1.,3.82321127348981));
#48722=CARTESIAN_POINT('Ctrl Pts',(0.199351525297396,-1.,3.81620203429702));
#48723=CARTESIAN_POINT('Ctrl Pts',(0.199351525297396,1.,3.81620203429702));
#48724=CARTESIAN_POINT('Ctrl Pts',(0.200274679433289,-1.,3.80909529318501));
#48725=CARTESIAN_POINT('Ctrl Pts',(0.200274679433289,1.,3.80909529318501));
#48726=CARTESIAN_POINT('Ctrl Pts',(0.201097756307251,-1.,3.80175247447171));
#48727=CARTESIAN_POINT('Ctrl Pts',(0.201097756307251,1.,3.80175247447171));
#48728=CARTESIAN_POINT('Ctrl Pts',(0.201807533800798,-1.,3.79408354187274));
#48729=CARTESIAN_POINT('Ctrl Pts',(0.201807533800798,1.,3.79408354187274));
#48730=CARTESIAN_POINT('Ctrl Pts',(0.202394260512192,-1.,3.78609175019317));
#48731=CARTESIAN_POINT('Ctrl Pts',(0.202394260512192,1.,3.78609175019317));
#48732=CARTESIAN_POINT('Ctrl Pts',(0.202854729699196,-1.,3.77793553476879));
#48733=CARTESIAN_POINT('Ctrl Pts',(0.202854729699196,1.,3.77793553476879));
#48734=CARTESIAN_POINT('Ctrl Pts',(0.203192390045337,-1.,3.76992071595267));
#48735=CARTESIAN_POINT('Ctrl Pts',(0.203192390045337,1.,3.76992071595267));
#48736=CARTESIAN_POINT('Ctrl Pts',(0.203414634707646,-1.,3.76242717937273));
#48737=CARTESIAN_POINT('Ctrl Pts',(0.203414634707646,1.,3.76242717937273));
#48738=CARTESIAN_POINT('Ctrl Pts',(0.203530796848403,-1.,3.75585118707924));
#48739=CARTESIAN_POINT('Ctrl Pts',(0.203530796848403,1.,3.75585118707924));
#48740=CARTESIAN_POINT('Ctrl Pts',(0.203550035479096,-1.,3.75054693397716));
#48741=CARTESIAN_POINT('Ctrl Pts',(0.203550035479096,1.,3.75054693397716));
#48742=CARTESIAN_POINT('Ctrl Pts',(0.203478844530229,-1.,3.74675472018582));
#48743=CARTESIAN_POINT('Ctrl Pts',(0.203478844530229,1.,3.74675472018582));
#48744=CARTESIAN_POINT('Ctrl Pts',(0.203352057956055,-1.,3.7450208092684));
#48745=CARTESIAN_POINT('Ctrl Pts',(0.203352057956055,1.,3.7450208092684));
#48746=CARTESIAN_POINT('Ctrl Pts',(0.203218215747894,-1.,3.74446880195845));
#48747=CARTESIAN_POINT('Ctrl Pts',(0.203218215747894,1.,3.74446880195845));
#48748=CARTESIAN_POINT('Ctrl Pts',(0.20311176758786,-1.,3.74443319346666));
#48749=CARTESIAN_POINT('Ctrl Pts',(0.20311176758786,1.,3.74443319346666));
#48750=CARTESIAN_POINT('Ctrl Pts',(0.203054238699719,-1.,3.74449849461127));
#48751=CARTESIAN_POINT('Ctrl Pts',(0.203054238699719,1.,3.74449849461127));
#48752=CARTESIAN_POINT('',(0.0760622897878233,1.,4.19931119685982));
#48753=CARTESIAN_POINT('Ctrl Pts',(0.0760622897878233,1.,4.19931119685982));
#48754=CARTESIAN_POINT('Ctrl Pts',(0.0767384596142192,1.,4.19789138621624));
#48755=CARTESIAN_POINT('Ctrl Pts',(0.0780873956244399,1.,4.19505112860624));
#48756=CARTESIAN_POINT('Ctrl Pts',(0.08010058871176,1.,4.19078883322483));
#48757=CARTESIAN_POINT('Ctrl Pts',(0.0827644164389507,1.,4.1851019532944));
#48758=CARTESIAN_POINT('Ctrl Pts',(0.0860600915552512,1.,4.17798698669991));
#48759=CARTESIAN_POINT('Ctrl Pts',(0.0893215560850325,1.,4.17086566491823));
#48760=CARTESIAN_POINT('Ctrl Pts',(0.0925486672167687,1.,4.16373802265942));
#48761=CARTESIAN_POINT('Ctrl Pts',(0.0957412403297065,1.,4.15660412653006));
#48762=CARTESIAN_POINT('Ctrl Pts',(0.0988990478899809,1.,4.1494640891762));
#48763=CARTESIAN_POINT('Ctrl Pts',(0.102021826577453,1.,4.14231804938737));
#48764=CARTESIAN_POINT('Ctrl Pts',(0.105109286538864,1.,4.13516614458396));
#48765=CARTESIAN_POINT('Ctrl Pts',(0.10816112052835,1.,4.12800848371386));
#48766=CARTESIAN_POINT('Ctrl Pts',(0.111177012683377,1.,4.12084512502444));
#48767=CARTESIAN_POINT('Ctrl Pts',(0.114156649609601,1.,4.11367603925313));
#48768=CARTESIAN_POINT('Ctrl Pts',(0.117099722731704,1.,4.10650113382187));
#48769=CARTESIAN_POINT('Ctrl Pts',(0.120005924388162,1.,4.09932031767243));
#48770=CARTESIAN_POINT('Ctrl Pts',(0.122874946249119,1.,4.09213355850836));
#48771=CARTESIAN_POINT('Ctrl Pts',(0.125706476822529,1.,4.08494093372315));
#48772=CARTESIAN_POINT('Ctrl Pts',(0.128500200484813,1.,4.07774270738809));
#48773=CARTESIAN_POINT('Ctrl Pts',(0.131255793548914,1.,4.07053931528579));
#48774=CARTESIAN_POINT('Ctrl Pts',(0.133972916144225,1.,4.06333121018476));
#48775=CARTESIAN_POINT('Ctrl Pts',(0.136651205046111,1.,4.05611873400122));
#48776=CARTESIAN_POINT('Ctrl Pts',(0.139290267180059,1.,4.04890199238056));
#48777=CARTESIAN_POINT('Ctrl Pts',(0.141889671485507,1.,4.04168069633842));
#48778=CARTESIAN_POINT('Ctrl Pts',(0.144448947038352,1.,4.03445411510403));
#48779=CARTESIAN_POINT('Ctrl Pts',(0.146967602878998,1.,4.02722143147048));
#48780=CARTESIAN_POINT('Ctrl Pts',(0.149445144968707,1.,4.01998203715588));
#48781=CARTESIAN_POINT('Ctrl Pts',(0.151881094022909,1.,4.01273584234684));
#48782=CARTESIAN_POINT('Ctrl Pts',(0.154275004872309,1.,4.00548360245297));
#48783=CARTESIAN_POINT('Ctrl Pts',(0.156626481393735,1.,3.99822717425869));
#48784=CARTESIAN_POINT('Ctrl Pts',(0.158935123982796,1.,3.99096873945862));
#48785=CARTESIAN_POINT('Ctrl Pts',(0.161200482186087,1.,3.98371010319866));
#48786=CARTESIAN_POINT('Ctrl Pts',(0.163422004609998,1.,3.97645194630944));
#48787=CARTESIAN_POINT('Ctrl Pts',(0.165598992851097,1.,3.9691931362141));
#48788=CARTESIAN_POINT('Ctrl Pts',(0.167730547023312,1.,3.96192990160296));
#48789=CARTESIAN_POINT('Ctrl Pts',(0.16981566637413,1.,3.95465744665263));
#48790=CARTESIAN_POINT('Ctrl Pts',(0.171853355369232,1.,3.94737164900861));
#48791=CARTESIAN_POINT('Ctrl Pts',(0.173842734974607,1.,3.94007083096214));
#48792=CARTESIAN_POINT('Ctrl Pts',(0.175783136893872,1.,3.93275726771049));
#48793=CARTESIAN_POINT('Ctrl Pts',(0.177674246152328,1.,3.92543942697672));
#48794=CARTESIAN_POINT('Ctrl Pts',(0.179515885822894,1.,3.91812876180948));
#48795=CARTESIAN_POINT('Ctrl Pts',(0.181307740731795,1.,3.91083557557193));
#48796=CARTESIAN_POINT('Ctrl Pts',(0.183049081993193,1.,3.90356488555138));
#48797=CARTESIAN_POINT('Ctrl Pts',(0.184738537728034,1.,3.89631300742633));
#48798=CARTESIAN_POINT('Ctrl Pts',(0.186373724985263,1.,3.88906196725817));
#48799=CARTESIAN_POINT('Ctrl Pts',(0.187951632512663,1.,3.88178563496187));
#48800=CARTESIAN_POINT('Ctrl Pts',(0.189469253358254,1.,3.87445976418377));
#48801=CARTESIAN_POINT('Ctrl Pts',(0.190924190418612,1.,3.8670715862477));
#48802=CARTESIAN_POINT('Ctrl Pts',(0.192315153044979,1.,3.85962774407652));
#48803=CARTESIAN_POINT('Ctrl Pts',(0.193642806777747,1.,3.85216762264019));
#48804=CARTESIAN_POINT('Ctrl Pts',(0.194909009460254,1.,3.84475203347052));
#48805=CARTESIAN_POINT('Ctrl Pts',(0.196115198971889,1.,3.83743910616265));
#48806=CARTESIAN_POINT('Ctrl Pts',(0.197260935827375,1.,3.83026221776488));
#48807=CARTESIAN_POINT('Ctrl Pts',(0.198342616900469,1.,3.82321127348981));
#48808=CARTESIAN_POINT('Ctrl Pts',(0.199351525297396,1.,3.81620203429702));
#48809=CARTESIAN_POINT('Ctrl Pts',(0.200274679433289,1.,3.80909529318501));
#48810=CARTESIAN_POINT('Ctrl Pts',(0.201097756307251,1.,3.80175247447171));
#48811=CARTESIAN_POINT('Ctrl Pts',(0.201807533800798,1.,3.79408354187274));
#48812=CARTESIAN_POINT('Ctrl Pts',(0.202394260512192,1.,3.78609175019317));
#48813=CARTESIAN_POINT('Ctrl Pts',(0.202854729699196,1.,3.77793553476879));
#48814=CARTESIAN_POINT('Ctrl Pts',(0.203192390045337,1.,3.76992071595267));
#48815=CARTESIAN_POINT('Ctrl Pts',(0.203414634707646,1.,3.76242717937273));
#48816=CARTESIAN_POINT('Ctrl Pts',(0.203530796848403,1.,3.75585118707924));
#48817=CARTESIAN_POINT('Ctrl Pts',(0.203550035479096,1.,3.75054693397716));
#48818=CARTESIAN_POINT('Ctrl Pts',(0.203484186269314,1.,3.74703926501843));
#48819=CARTESIAN_POINT('Ctrl Pts',(0.203375226874331,1.,3.74535749969262));
#48820=CARTESIAN_POINT('Ctrl Pts',(0.203266610111263,1.,3.74471097893961));
#48821=CARTESIAN_POINT('Ctrl Pts',(0.203188003947964,1.,3.74453008995129));
#48822=CARTESIAN_POINT('Ctrl Pts',(0.203156094897895,1.,3.74449296982994));
#48823=CARTESIAN_POINT('',(0.0760622897878233,0.,4.19931119685982));
#48824=CARTESIAN_POINT('Ctrl Pts',(-0.20305423869972,-1.,3.74449849461127));
#48825=CARTESIAN_POINT('Ctrl Pts',(-0.20305423869972,1.,3.74449849461127));
#48826=CARTESIAN_POINT('Ctrl Pts',(-0.203111767587923,-1.,3.7444331934681));
#48827=CARTESIAN_POINT('Ctrl Pts',(-0.203111767587923,1.,3.7444331934681));
#48828=CARTESIAN_POINT('Ctrl Pts',(-0.203218215748059,-1.,3.7444688019622));
#48829=CARTESIAN_POINT('Ctrl Pts',(-0.203218215748059,1.,3.7444688019622));
#48830=CARTESIAN_POINT('Ctrl Pts',(-0.203352057956297,-1.,3.74502080927395));
#48831=CARTESIAN_POINT('Ctrl Pts',(-0.203352057956297,1.,3.74502080927395));
#48832=CARTESIAN_POINT('Ctrl Pts',(-0.203478844530447,-1.,3.7467547201908));
#48833=CARTESIAN_POINT('Ctrl Pts',(-0.203478844530447,1.,3.7467547201908));
#48834=CARTESIAN_POINT('Ctrl Pts',(-0.203550035479166,-1.,3.75054693397875));
#48835=CARTESIAN_POINT('Ctrl Pts',(-0.203550035479166,1.,3.75054693397875));
#48836=CARTESIAN_POINT('Ctrl Pts',(-0.203530796848322,-1.,3.75585118707734));
#48837=CARTESIAN_POINT('Ctrl Pts',(-0.203530796848322,1.,3.75585118707734));
#48838=CARTESIAN_POINT('Ctrl Pts',(-0.203414634707479,-1.,3.76242717936885));
#48839=CARTESIAN_POINT('Ctrl Pts',(-0.203414634707479,1.,3.76242717936885));
#48840=CARTESIAN_POINT('Ctrl Pts',(-0.203192390045165,-1.,3.7699207159487));
#48841=CARTESIAN_POINT('Ctrl Pts',(-0.203192390045165,1.,3.7699207159487));
#48842=CARTESIAN_POINT('Ctrl Pts',(-0.202854729699081,-1.,3.77793553476614));
#48843=CARTESIAN_POINT('Ctrl Pts',(-0.202854729699081,1.,3.77793553476614));
#48844=CARTESIAN_POINT('Ctrl Pts',(-0.20239426051216,-1.,3.78609175019242));
#48845=CARTESIAN_POINT('Ctrl Pts',(-0.20239426051216,1.,3.78609175019242));
#48846=CARTESIAN_POINT('Ctrl Pts',(-0.201807533800837,-1.,3.7940835418736));
#48847=CARTESIAN_POINT('Ctrl Pts',(-0.201807533800837,1.,3.7940835418736));
#48848=CARTESIAN_POINT('Ctrl Pts',(-0.201097756307326,-1.,3.80175247447337));
#48849=CARTESIAN_POINT('Ctrl Pts',(-0.201097756307326,1.,3.80175247447337));
#48850=CARTESIAN_POINT('Ctrl Pts',(-0.200274679433365,-1.,3.80909529318669));
#48851=CARTESIAN_POINT('Ctrl Pts',(-0.200274679433365,1.,3.80909529318669));
#48852=CARTESIAN_POINT('Ctrl Pts',(-0.199351525297447,-1.,3.81620203429815));
#48853=CARTESIAN_POINT('Ctrl Pts',(-0.199351525297447,1.,3.81620203429815));
#48854=CARTESIAN_POINT('Ctrl Pts',(-0.198342616900487,-1.,3.82321127349016));
#48855=CARTESIAN_POINT('Ctrl Pts',(-0.198342616900487,1.,3.82321127349016));
#48856=CARTESIAN_POINT('Ctrl Pts',(-0.197260935827362,-1.,3.83026221776456));
#48857=CARTESIAN_POINT('Ctrl Pts',(-0.197260935827362,1.,3.83026221776456));
#48858=CARTESIAN_POINT('Ctrl Pts',(-0.196115198971859,-1.,3.83743910616195));
#48859=CARTESIAN_POINT('Ctrl Pts',(-0.196115198971859,1.,3.83743910616195));
#48860=CARTESIAN_POINT('Ctrl Pts',(-0.194909009460221,-1.,3.84475203346977));
#48861=CARTESIAN_POINT('Ctrl Pts',(-0.194909009460221,1.,3.84475203346977));
#48862=CARTESIAN_POINT('Ctrl Pts',(-0.193642806777723,-1.,3.85216762263966));
#48863=CARTESIAN_POINT('Ctrl Pts',(-0.193642806777723,1.,3.85216762263966));
#48864=CARTESIAN_POINT('Ctrl Pts',(-0.192315153044971,-1.,3.85962774407633));
#48865=CARTESIAN_POINT('Ctrl Pts',(-0.192315153044971,1.,3.85962774407633));
#48866=CARTESIAN_POINT('Ctrl Pts',(-0.19092419041862,-1.,3.86707158624783));
#48867=CARTESIAN_POINT('Ctrl Pts',(-0.19092419041862,1.,3.86707158624783));
#48868=CARTESIAN_POINT('Ctrl Pts',(-0.189469253358273,-1.,3.87445976418412));
#48869=CARTESIAN_POINT('Ctrl Pts',(-0.189469253358273,1.,3.87445976418412));
#48870=CARTESIAN_POINT('Ctrl Pts',(-0.187951632512685,-1.,3.88178563496228));
#48871=CARTESIAN_POINT('Ctrl Pts',(-0.187951632512685,1.,3.88178563496228));
#48872=CARTESIAN_POINT('Ctrl Pts',(-0.186373724985281,-1.,3.88906196725848));
#48873=CARTESIAN_POINT('Ctrl Pts',(-0.186373724985281,1.,3.88906196725848));
#48874=CARTESIAN_POINT('Ctrl Pts',(-0.184738537728043,-1.,3.89631300742646));
#48875=CARTESIAN_POINT('Ctrl Pts',(-0.184738537728043,1.,3.89631300742646));
#48876=CARTESIAN_POINT('Ctrl Pts',(-0.183049081993191,-1.,3.90356488555132));
#48877=CARTESIAN_POINT('Ctrl Pts',(-0.183049081993191,1.,3.90356488555132));
#48878=CARTESIAN_POINT('Ctrl Pts',(-0.181307740731786,-1.,3.91083557557175));
#48879=CARTESIAN_POINT('Ctrl Pts',(-0.181307740731786,1.,3.91083557557175));
#48880=CARTESIAN_POINT('Ctrl Pts',(-0.179515885822882,-1.,3.91812876180926));
#48881=CARTESIAN_POINT('Ctrl Pts',(-0.179515885822882,1.,3.91812876180926));
#48882=CARTESIAN_POINT('Ctrl Pts',(-0.177674246152318,-1.,3.92543942697655));
#48883=CARTESIAN_POINT('Ctrl Pts',(-0.177674246152318,1.,3.92543942697655));
#48884=CARTESIAN_POINT('Ctrl Pts',(-0.175783136893868,-1.,3.93275726771042));
#48885=CARTESIAN_POINT('Ctrl Pts',(-0.175783136893868,1.,3.93275726771042));
#48886=CARTESIAN_POINT('Ctrl Pts',(-0.17384273497461,-1.,3.94007083096217));
#48887=CARTESIAN_POINT('Ctrl Pts',(-0.17384273497461,1.,3.94007083096217));
#48888=CARTESIAN_POINT('Ctrl Pts',(-0.17185335536924,-1.,3.94737164900868));
#48889=CARTESIAN_POINT('Ctrl Pts',(-0.17185335536924,1.,3.94737164900868));
#48890=CARTESIAN_POINT('Ctrl Pts',(-0.169815666374139,-1.,3.95465744665268));
#48891=CARTESIAN_POINT('Ctrl Pts',(-0.169815666374139,1.,3.95465744665268));
#48892=CARTESIAN_POINT('Ctrl Pts',(-0.16773054702332,-1.,3.96192990160296));
#48893=CARTESIAN_POINT('Ctrl Pts',(-0.16773054702332,1.,3.96192990160296));
#48894=CARTESIAN_POINT('Ctrl Pts',(-0.165598992851102,-1.,3.96919313621407));
#48895=CARTESIAN_POINT('Ctrl Pts',(-0.165598992851102,1.,3.96919313621407));
#48896=CARTESIAN_POINT('Ctrl Pts',(-0.163422004609999,-1.,3.97645194630943));
#48897=CARTESIAN_POINT('Ctrl Pts',(-0.163422004609999,1.,3.97645194630943));
#48898=CARTESIAN_POINT('Ctrl Pts',(-0.161200482186085,-1.,3.98371010319872));
#48899=CARTESIAN_POINT('Ctrl Pts',(-0.161200482186085,1.,3.98371010319872));
#48900=CARTESIAN_POINT('Ctrl Pts',(-0.158935123982793,-1.,3.99096873945878));
#48901=CARTESIAN_POINT('Ctrl Pts',(-0.158935123982793,1.,3.99096873945878));
#48902=CARTESIAN_POINT('Ctrl Pts',(-0.156626481393734,-1.,3.99822717425893));
#48903=CARTESIAN_POINT('Ctrl Pts',(-0.156626481393734,1.,3.99822717425893));
#48904=CARTESIAN_POINT('Ctrl Pts',(-0.154275004872311,-1.,4.00548360245319));
#48905=CARTESIAN_POINT('Ctrl Pts',(-0.154275004872311,1.,4.00548360245319));
#48906=CARTESIAN_POINT('Ctrl Pts',(-0.151881094022911,-1.,4.01273584234689));
#48907=CARTESIAN_POINT('Ctrl Pts',(-0.151881094022911,1.,4.01273584234689));
#48908=CARTESIAN_POINT('Ctrl Pts',(-0.149445144968707,-1.,4.01998203715564));
#48909=CARTESIAN_POINT('Ctrl Pts',(-0.149445144968707,1.,4.01998203715564));
#48910=CARTESIAN_POINT('Ctrl Pts',(-0.146967602878994,-1.,4.02722143146994));
#48911=CARTESIAN_POINT('Ctrl Pts',(-0.146967602878994,1.,4.02722143146994));
#48912=CARTESIAN_POINT('Ctrl Pts',(-0.144448947038345,-1.,4.03445411510333));
#48913=CARTESIAN_POINT('Ctrl Pts',(-0.144448947038345,1.,4.03445411510333));
#48914=CARTESIAN_POINT('Ctrl Pts',(-0.1418896714855,-1.,4.04168069633781));
#48915=CARTESIAN_POINT('Ctrl Pts',(-0.1418896714855,1.,4.04168069633781));
#48916=CARTESIAN_POINT('Ctrl Pts',(-0.139290267180057,-1.,4.04890199238036));
#48917=CARTESIAN_POINT('Ctrl Pts',(-0.139290267180057,1.,4.04890199238036));
#48918=CARTESIAN_POINT('Ctrl Pts',(-0.136651205046119,-1.,4.05611873400172));
#48919=CARTESIAN_POINT('Ctrl Pts',(-0.136651205046119,1.,4.05611873400172));
#48920=CARTESIAN_POINT('Ctrl Pts',(-0.133972916144245,-1.,4.06333121018596));
#48921=CARTESIAN_POINT('Ctrl Pts',(-0.133972916144245,1.,4.06333121018596));
#48922=CARTESIAN_POINT('Ctrl Pts',(-0.131255793548941,-1.,4.0705393152874));
#48923=CARTESIAN_POINT('Ctrl Pts',(-0.131255793548941,1.,4.0705393152874));
#48924=CARTESIAN_POINT('Ctrl Pts',(-0.128500200484838,-1.,4.07774270738954));
#48925=CARTESIAN_POINT('Ctrl Pts',(-0.128500200484838,1.,4.07774270738954));
#48926=CARTESIAN_POINT('Ctrl Pts',(-0.12570647682254,-1.,4.08494093372377));
#48927=CARTESIAN_POINT('Ctrl Pts',(-0.12570647682254,1.,4.08494093372377));
#48928=CARTESIAN_POINT('Ctrl Pts',(-0.122874946249107,-1.,4.09213355850756));
#48929=CARTESIAN_POINT('Ctrl Pts',(-0.122874946249107,1.,4.09213355850756));
#48930=CARTESIAN_POINT('Ctrl Pts',(-0.120005924388124,-1.,4.09932031767002));
#48931=CARTESIAN_POINT('Ctrl Pts',(-0.120005924388124,1.,4.09932031767002));
#48932=CARTESIAN_POINT('Ctrl Pts',(-0.117099722731648,-1.,4.10650113381833));
#48933=CARTESIAN_POINT('Ctrl Pts',(-0.117099722731648,1.,4.10650113381833));
#48934=CARTESIAN_POINT('Ctrl Pts',(-0.114156649609546,-1.,4.11367603924961));
#48935=CARTESIAN_POINT('Ctrl Pts',(-0.114156649609546,1.,4.11367603924961));
#48936=CARTESIAN_POINT('Ctrl Pts',(-0.111177012683347,-1.,4.1208451250225));
#48937=CARTESIAN_POINT('Ctrl Pts',(-0.111177012683347,1.,4.1208451250225));
#48938=CARTESIAN_POINT('Ctrl Pts',(-0.10816112052837,-1.,4.12800848371504));
#48939=CARTESIAN_POINT('Ctrl Pts',(-0.10816112052837,1.,4.12800848371504));
#48940=CARTESIAN_POINT('Ctrl Pts',(-0.105109286538945,-1.,4.13516614458895));
#48941=CARTESIAN_POINT('Ctrl Pts',(-0.105109286538945,1.,4.13516614458895));
#48942=CARTESIAN_POINT('Ctrl Pts',(-0.102021826577584,-1.,4.14231804939538));
#48943=CARTESIAN_POINT('Ctrl Pts',(-0.102021826577584,1.,4.14231804939538));
#48944=CARTESIAN_POINT('Ctrl Pts',(-0.0988990478901228,-1.,4.14946408918485));
#48945=CARTESIAN_POINT('Ctrl Pts',(-0.0988990478901228,1.,4.14946408918485));
#48946=CARTESIAN_POINT('Ctrl Pts',(-0.0957412403298009,-1.,4.15660412653577));
#48947=CARTESIAN_POINT('Ctrl Pts',(-0.0957412403298009,1.,4.15660412653577));
#48948=CARTESIAN_POINT('Ctrl Pts',(-0.0925486672167534,-1.,4.16373802265839));
#48949=CARTESIAN_POINT('Ctrl Pts',(-0.0925486672167534,1.,4.16373802265839));
#48950=CARTESIAN_POINT('Ctrl Pts',(-0.0893215560848652,-1.,4.17086566490794));
#48951=CARTESIAN_POINT('Ctrl Pts',(-0.0893215560848652,1.,4.17086566490794));
#48952=CARTESIAN_POINT('Ctrl Pts',(-0.0860600915549399,-1.,4.17798698668094));
#48953=CARTESIAN_POINT('Ctrl Pts',(-0.0860600915549399,1.,4.17798698668094));
#48954=CARTESIAN_POINT('Ctrl Pts',(-0.0827644164385681,-1.,4.18510195327123));
#48955=CARTESIAN_POINT('Ctrl Pts',(-0.0827644164385681,1.,4.18510195327123));
#48956=CARTESIAN_POINT('Ctrl Pts',(-0.0801005887114322,-1.,4.19078883320504));
#48957=CARTESIAN_POINT('Ctrl Pts',(-0.0801005887114322,1.,4.19078883320504));
#48958=CARTESIAN_POINT('Ctrl Pts',(-0.07808739562424,-1.,4.19505112859416));
#48959=CARTESIAN_POINT('Ctrl Pts',(-0.07808739562424,1.,4.19505112859416));
#48960=CARTESIAN_POINT('Ctrl Pts',(-0.0767384596141467,-1.,4.1978913862118));
#48961=CARTESIAN_POINT('Ctrl Pts',(-0.0767384596141467,1.,4.1978913862118));
#48962=CARTESIAN_POINT('Ctrl Pts',(-0.0760622897878249,-1.,4.19931119685982));
#48963=CARTESIAN_POINT('Ctrl Pts',(-0.0760622897878249,1.,4.19931119685982));
#48964=CARTESIAN_POINT('',(-0.203156094896102,1.,3.74449296983004));
#48965=CARTESIAN_POINT('Ctrl Pts',(-0.203156094896101,-1.,3.74449296983004));
#48966=CARTESIAN_POINT('Ctrl Pts',(-0.203156094896101,-0.666666666666667,
3.74449296983004));
#48967=CARTESIAN_POINT('Ctrl Pts',(-0.203156094896101,-0.333333333333333,
3.74449296983004));
#48968=CARTESIAN_POINT('Ctrl Pts',(-0.203156094896101,0.333333333333333,
3.74449296983004));
#48969=CARTESIAN_POINT('Ctrl Pts',(-0.203156094896101,0.666666666666667,
3.74449296983004));
#48970=CARTESIAN_POINT('Ctrl Pts',(-0.203156094896101,1.,3.74449296983004));
#48971=CARTESIAN_POINT('',(-0.0760622897878249,1.,4.19931119685982));
#48972=CARTESIAN_POINT('',(-0.0760622897878249,0.,4.19931119685982));
#48973=CARTESIAN_POINT('Ctrl Pts',(-0.203156094896101,1.,3.74449296983004));
#48974=CARTESIAN_POINT('Ctrl Pts',(-0.203188003946657,1.,3.74453008995092));
#48975=CARTESIAN_POINT('Ctrl Pts',(-0.203266610110531,1.,3.74471097893845));
#48976=CARTESIAN_POINT('Ctrl Pts',(-0.203375226874122,1.,3.74535749969115));
#48977=CARTESIAN_POINT('Ctrl Pts',(-0.203484186269415,1.,3.74703926501752));
#48978=CARTESIAN_POINT('Ctrl Pts',(-0.203550035479166,1.,3.75054693397875));
#48979=CARTESIAN_POINT('Ctrl Pts',(-0.203530796848322,1.,3.75585118707734));
#48980=CARTESIAN_POINT('Ctrl Pts',(-0.203414634707479,1.,3.76242717936885));
#48981=CARTESIAN_POINT('Ctrl Pts',(-0.203192390045165,1.,3.7699207159487));
#48982=CARTESIAN_POINT('Ctrl Pts',(-0.202854729699081,1.,3.77793553476614));
#48983=CARTESIAN_POINT('Ctrl Pts',(-0.20239426051216,1.,3.78609175019242));
#48984=CARTESIAN_POINT('Ctrl Pts',(-0.201807533800837,1.,3.7940835418736));
#48985=CARTESIAN_POINT('Ctrl Pts',(-0.201097756307326,1.,3.80175247447337));
#48986=CARTESIAN_POINT('Ctrl Pts',(-0.200274679433365,1.,3.80909529318669));
#48987=CARTESIAN_POINT('Ctrl Pts',(-0.199351525297447,1.,3.81620203429815));
#48988=CARTESIAN_POINT('Ctrl Pts',(-0.198342616900487,1.,3.82321127349016));
#48989=CARTESIAN_POINT('Ctrl Pts',(-0.197260935827362,1.,3.83026221776456));
#48990=CARTESIAN_POINT('Ctrl Pts',(-0.196115198971859,1.,3.83743910616195));
#48991=CARTESIAN_POINT('Ctrl Pts',(-0.194909009460221,1.,3.84475203346977));
#48992=CARTESIAN_POINT('Ctrl Pts',(-0.193642806777723,1.,3.85216762263966));
#48993=CARTESIAN_POINT('Ctrl Pts',(-0.192315153044971,1.,3.85962774407633));
#48994=CARTESIAN_POINT('Ctrl Pts',(-0.19092419041862,1.,3.86707158624783));
#48995=CARTESIAN_POINT('Ctrl Pts',(-0.189469253358273,1.,3.87445976418412));
#48996=CARTESIAN_POINT('Ctrl Pts',(-0.187951632512685,1.,3.88178563496228));
#48997=CARTESIAN_POINT('Ctrl Pts',(-0.186373724985281,1.,3.88906196725848));
#48998=CARTESIAN_POINT('Ctrl Pts',(-0.184738537728043,1.,3.89631300742646));
#48999=CARTESIAN_POINT('Ctrl Pts',(-0.183049081993191,1.,3.90356488555132));
#49000=CARTESIAN_POINT('Ctrl Pts',(-0.181307740731786,1.,3.91083557557175));
#49001=CARTESIAN_POINT('Ctrl Pts',(-0.179515885822882,1.,3.91812876180926));
#49002=CARTESIAN_POINT('Ctrl Pts',(-0.177674246152318,1.,3.92543942697655));
#49003=CARTESIAN_POINT('Ctrl Pts',(-0.175783136893868,1.,3.93275726771042));
#49004=CARTESIAN_POINT('Ctrl Pts',(-0.17384273497461,1.,3.94007083096217));
#49005=CARTESIAN_POINT('Ctrl Pts',(-0.17185335536924,1.,3.94737164900868));
#49006=CARTESIAN_POINT('Ctrl Pts',(-0.169815666374139,1.,3.95465744665268));
#49007=CARTESIAN_POINT('Ctrl Pts',(-0.16773054702332,1.,3.96192990160296));
#49008=CARTESIAN_POINT('Ctrl Pts',(-0.165598992851102,1.,3.96919313621407));
#49009=CARTESIAN_POINT('Ctrl Pts',(-0.163422004609999,1.,3.97645194630943));
#49010=CARTESIAN_POINT('Ctrl Pts',(-0.161200482186085,1.,3.98371010319872));
#49011=CARTESIAN_POINT('Ctrl Pts',(-0.158935123982793,1.,3.99096873945878));
#49012=CARTESIAN_POINT('Ctrl Pts',(-0.156626481393734,1.,3.99822717425893));
#49013=CARTESIAN_POINT('Ctrl Pts',(-0.154275004872311,1.,4.00548360245319));
#49014=CARTESIAN_POINT('Ctrl Pts',(-0.151881094022911,1.,4.01273584234689));
#49015=CARTESIAN_POINT('Ctrl Pts',(-0.149445144968707,1.,4.01998203715564));
#49016=CARTESIAN_POINT('Ctrl Pts',(-0.146967602878994,1.,4.02722143146994));
#49017=CARTESIAN_POINT('Ctrl Pts',(-0.144448947038345,1.,4.03445411510333));
#49018=CARTESIAN_POINT('Ctrl Pts',(-0.1418896714855,1.,4.04168069633781));
#49019=CARTESIAN_POINT('Ctrl Pts',(-0.139290267180057,1.,4.04890199238036));
#49020=CARTESIAN_POINT('Ctrl Pts',(-0.136651205046119,1.,4.05611873400172));
#49021=CARTESIAN_POINT('Ctrl Pts',(-0.133972916144245,1.,4.06333121018596));
#49022=CARTESIAN_POINT('Ctrl Pts',(-0.131255793548941,1.,4.0705393152874));
#49023=CARTESIAN_POINT('Ctrl Pts',(-0.128500200484838,1.,4.07774270738954));
#49024=CARTESIAN_POINT('Ctrl Pts',(-0.12570647682254,1.,4.08494093372377));
#49025=CARTESIAN_POINT('Ctrl Pts',(-0.122874946249107,1.,4.09213355850756));
#49026=CARTESIAN_POINT('Ctrl Pts',(-0.120005924388124,1.,4.09932031767002));
#49027=CARTESIAN_POINT('Ctrl Pts',(-0.117099722731648,1.,4.10650113381833));
#49028=CARTESIAN_POINT('Ctrl Pts',(-0.114156649609546,1.,4.11367603924961));
#49029=CARTESIAN_POINT('Ctrl Pts',(-0.111177012683347,1.,4.1208451250225));
#49030=CARTESIAN_POINT('Ctrl Pts',(-0.10816112052837,1.,4.12800848371504));
#49031=CARTESIAN_POINT('Ctrl Pts',(-0.105109286538945,1.,4.13516614458895));
#49032=CARTESIAN_POINT('Ctrl Pts',(-0.102021826577584,1.,4.14231804939538));
#49033=CARTESIAN_POINT('Ctrl Pts',(-0.0988990478901228,1.,4.14946408918485));
#49034=CARTESIAN_POINT('Ctrl Pts',(-0.0957412403298009,1.,4.15660412653577));
#49035=CARTESIAN_POINT('Ctrl Pts',(-0.0925486672167534,1.,4.16373802265839));
#49036=CARTESIAN_POINT('Ctrl Pts',(-0.0893215560848652,1.,4.17086566490794));
#49037=CARTESIAN_POINT('Ctrl Pts',(-0.0860600915549399,1.,4.17798698668094));
#49038=CARTESIAN_POINT('Ctrl Pts',(-0.0827644164385681,1.,4.18510195327123));
#49039=CARTESIAN_POINT('Ctrl Pts',(-0.0801005887114322,1.,4.19078883320504));
#49040=CARTESIAN_POINT('Ctrl Pts',(-0.07808739562424,1.,4.19505112859416));
#49041=CARTESIAN_POINT('Ctrl Pts',(-0.0767384596141467,1.,4.1978913862118));
#49042=CARTESIAN_POINT('Ctrl Pts',(-0.0760622897878249,1.,4.19931119685982));
#49043=CARTESIAN_POINT('Origin',(-0.0760622897878249,0.,4.19931119685982));
#49044=CARTESIAN_POINT('',(0.0760622897878233,1.,4.19931119685982));
#49045=CARTESIAN_POINT('Origin',(0.,0.,0.));
#49046=CARTESIAN_POINT('',(-0.385112848330762,1.,3.73017266276651));
#49047=CARTESIAN_POINT('Origin',(0.,1.,0.));
#49048=CARTESIAN_POINT('Ctrl Pts',(-0.385112848330762,1.,3.73017266276651));
#49049=CARTESIAN_POINT('Ctrl Pts',(-0.385112848330762,0.666666666666667,
3.73017266276651));
#49050=CARTESIAN_POINT('Ctrl Pts',(-0.385112848330762,0.333333333333333,
3.73017266276651));
#49051=CARTESIAN_POINT('Ctrl Pts',(-0.385112848330762,-0.333333333333333,
3.73017266276651));
#49052=CARTESIAN_POINT('Ctrl Pts',(-0.385112848330762,-0.666666666666667,
3.73017266276651));
#49053=CARTESIAN_POINT('Ctrl Pts',(-0.385112848330762,-1.,3.73017266276651));
#49054=CARTESIAN_POINT('Ctrl Pts',(-0.581791163835815,-1.,4.15950947128175));
#49055=CARTESIAN_POINT('Ctrl Pts',(-0.581791163835815,1.,4.15950947128175));
#49056=CARTESIAN_POINT('Ctrl Pts',(-0.580901211463535,-1.,4.1582129171283));
#49057=CARTESIAN_POINT('Ctrl Pts',(-0.580901211463535,1.,4.1582129171283));
#49058=CARTESIAN_POINT('Ctrl Pts',(-0.579124568914235,-1.,4.15561864788576));
#49059=CARTESIAN_POINT('Ctrl Pts',(-0.579124568914235,1.,4.15561864788576));
#49060=CARTESIAN_POINT('Ctrl Pts',(-0.576469391676688,-1.,4.151723761217));
#49061=CARTESIAN_POINT('Ctrl Pts',(-0.576469391676688,1.,4.151723761217));
#49062=CARTESIAN_POINT('Ctrl Pts',(-0.572948736069522,-1.,4.14652361068081));
#49063=CARTESIAN_POINT('Ctrl Pts',(-0.572948736069522,1.,4.14652361068081));
#49064=CARTESIAN_POINT('Ctrl Pts',(-0.568580610189775,-1.,4.14001179830547));
#49065=CARTESIAN_POINT('Ctrl Pts',(-0.568580610189775,1.,4.14001179830547));
#49066=CARTESIAN_POINT('Ctrl Pts',(-0.564245279537149,-1.,4.13348835727104));
#49067=CARTESIAN_POINT('Ctrl Pts',(-0.564245279537149,1.,4.13348835727104));
#49068=CARTESIAN_POINT('Ctrl Pts',(-0.559942890594774,-1.,4.12695329951961));
#49069=CARTESIAN_POINT('Ctrl Pts',(-0.559942890594774,1.,4.12695329951961));
#49070=CARTESIAN_POINT('Ctrl Pts',(-0.555673636129977,-1.,4.12040666195664));
#49071=CARTESIAN_POINT('Ctrl Pts',(-0.555673636129977,1.,4.12040666195664));
#49072=CARTESIAN_POINT('Ctrl Pts',(-0.551437758497033,-1.,4.11384852024721));
#49073=CARTESIAN_POINT('Ctrl Pts',(-0.551437758497033,1.,4.11384852024721));
#49074=CARTESIAN_POINT('Ctrl Pts',(-0.547235539485637,-1.,4.10727897027977));
#49075=CARTESIAN_POINT('Ctrl Pts',(-0.547235539485637,1.,4.10727897027977));
#49076=CARTESIAN_POINT('Ctrl Pts',(-0.543067286877757,-1.,4.10069810243979));
#49077=CARTESIAN_POINT('Ctrl Pts',(-0.543067286877757,1.,4.10069810243979));
#49078=CARTESIAN_POINT('Ctrl Pts',(-0.538933321179756,-1.,4.09410597627));
#49079=CARTESIAN_POINT('Ctrl Pts',(-0.538933321179756,1.,4.09410597627));
#49080=CARTESIAN_POINT('Ctrl Pts',(-0.534833963477273,-1.,4.08750259988885));
#49081=CARTESIAN_POINT('Ctrl Pts',(-0.534833963477273,1.,4.08750259988885));
#49082=CARTESIAN_POINT('Ctrl Pts',(-0.530769518728571,-1.,4.08088789536836));
#49083=CARTESIAN_POINT('Ctrl Pts',(-0.530769518728571,1.,4.08088789536836));
#49084=CARTESIAN_POINT('Ctrl Pts',(-0.526740277227498,-1.,4.07426172299847));
#49085=CARTESIAN_POINT('Ctrl Pts',(-0.526740277227498,1.,4.07426172299847));
#49086=CARTESIAN_POINT('Ctrl Pts',(-0.522746528603107,-1.,4.06762394471314));
#49087=CARTESIAN_POINT('Ctrl Pts',(-0.522746528603107,1.,4.06762394471314));
#49088=CARTESIAN_POINT('Ctrl Pts',(-0.518788572336924,-1.,4.06097448038013));
#49089=CARTESIAN_POINT('Ctrl Pts',(-0.518788572336924,1.,4.06097448038013));
#49090=CARTESIAN_POINT('Ctrl Pts',(-0.514866728193017,-1.,4.05431335771199));
#49091=CARTESIAN_POINT('Ctrl Pts',(-0.514866728193017,1.,4.05431335771199));
#49092=CARTESIAN_POINT('Ctrl Pts',(-0.51098134921897,-1.,4.04764078815447));
#49093=CARTESIAN_POINT('Ctrl Pts',(-0.51098134921897,1.,4.04764078815447));
#49094=CARTESIAN_POINT('Ctrl Pts',(-0.507132823288136,-1.,4.04095715148915));
#49095=CARTESIAN_POINT('Ctrl Pts',(-0.507132823288136,1.,4.04095715148915));
#49096=CARTESIAN_POINT('Ctrl Pts',(-0.503321556915346,-1.,4.03426284174272));
#49097=CARTESIAN_POINT('Ctrl Pts',(-0.503321556915346,1.,4.03426284174272));
#49098=CARTESIAN_POINT('Ctrl Pts',(-0.499547962340821,-1.,4.02755813980101));
#49099=CARTESIAN_POINT('Ctrl Pts',(-0.499547962340821,1.,4.02755813980101));
#49100=CARTESIAN_POINT('Ctrl Pts',(-0.495812444326251,-1.,4.02084308851832));
#49101=CARTESIAN_POINT('Ctrl Pts',(-0.495812444326251,1.,4.02084308851832));
#49102=CARTESIAN_POINT('Ctrl Pts',(-0.492115383418018,-1.,4.01411733503546));
#49103=CARTESIAN_POINT('Ctrl Pts',(-0.492115383418018,1.,4.01411733503546));
#49104=CARTESIAN_POINT('Ctrl Pts',(-0.488457130424633,-1.,4.0073800839099));
#49105=CARTESIAN_POINT('Ctrl Pts',(-0.488457130424633,1.,4.0073800839099));
#49106=CARTESIAN_POINT('Ctrl Pts',(-0.484838042421835,-1.,4.00063045119288));
#49107=CARTESIAN_POINT('Ctrl Pts',(-0.484838042421835,1.,4.00063045119288));
#49108=CARTESIAN_POINT('Ctrl Pts',(-0.481258512209675,-1.,3.99386775880679));
#49109=CARTESIAN_POINT('Ctrl Pts',(-0.481258512209675,1.,3.99386775880679));
#49110=CARTESIAN_POINT('Ctrl Pts',(-0.477718999122027,-1.,3.98709184306738));
#49111=CARTESIAN_POINT('Ctrl Pts',(-0.477718999122027,1.,3.98709184306738));
#49112=CARTESIAN_POINT('Ctrl Pts',(-0.47422006101951,-1.,3.98030338044409));
#49113=CARTESIAN_POINT('Ctrl Pts',(-0.47422006101951,1.,3.98030338044409));
#49114=CARTESIAN_POINT('Ctrl Pts',(-0.470762379613439,-1.,3.97350414289392));
#49115=CARTESIAN_POINT('Ctrl Pts',(-0.470762379613439,1.,3.97350414289392));
#49116=CARTESIAN_POINT('Ctrl Pts',(-0.467346690880643,-1.,3.9666962227393));
#49117=CARTESIAN_POINT('Ctrl Pts',(-0.467346690880643,1.,3.9666962227393));
#49118=CARTESIAN_POINT('Ctrl Pts',(-0.463973722115733,-1.,3.95988133243538));
#49119=CARTESIAN_POINT('Ctrl Pts',(-0.463973722115733,1.,3.95988133243538));
#49120=CARTESIAN_POINT('Ctrl Pts',(-0.460644124429121,-1.,3.95306005817364));
#49121=CARTESIAN_POINT('Ctrl Pts',(-0.460644124429121,1.,3.95306005817364));
#49122=CARTESIAN_POINT('Ctrl Pts',(-0.457358410451683,-1.,3.94623117206678));
#49123=CARTESIAN_POINT('Ctrl Pts',(-0.457358410451683,1.,3.94623117206678));
#49124=CARTESIAN_POINT('Ctrl Pts',(-0.454116879027584,-1.,3.93939080846298));
#49125=CARTESIAN_POINT('Ctrl Pts',(-0.454116879027584,1.,3.93939080846298));
#49126=CARTESIAN_POINT('Ctrl Pts',(-0.450919768356348,-1.,3.93253407403123));
#49127=CARTESIAN_POINT('Ctrl Pts',(-0.450919768356348,1.,3.93253407403123));
#49128=CARTESIAN_POINT('Ctrl Pts',(-0.447767416837293,-1.,3.92565674143416));
#49129=CARTESIAN_POINT('Ctrl Pts',(-0.447767416837293,1.,3.92565674143416));
#49130=CARTESIAN_POINT('Ctrl Pts',(-0.444660430230591,-1.,3.91875701610719));
#49131=CARTESIAN_POINT('Ctrl Pts',(-0.444660430230591,1.,3.91875701610719));
#49132=CARTESIAN_POINT('Ctrl Pts',(-0.441599824524054,-1.,3.91183704069153));
#49133=CARTESIAN_POINT('Ctrl Pts',(-0.441599824524054,1.,3.91183704069153));
#49134=CARTESIAN_POINT('Ctrl Pts',(-0.43858723545825,-1.,3.90490512938563));
#49135=CARTESIAN_POINT('Ctrl Pts',(-0.43858723545825,1.,3.90490512938563));
#49136=CARTESIAN_POINT('Ctrl Pts',(-0.435624629433528,-1.,3.89797256655462));
#49137=CARTESIAN_POINT('Ctrl Pts',(-0.435624629433528,1.,3.89797256655462));
#49138=CARTESIAN_POINT('Ctrl Pts',(-0.432713929544458,-1.,3.89104947940611));
#49139=CARTESIAN_POINT('Ctrl Pts',(-0.432713929544458,1.,3.89104947940611));
#49140=CARTESIAN_POINT('Ctrl Pts',(-0.429856640579741,-1.,3.88414070943341));
#49141=CARTESIAN_POINT('Ctrl Pts',(-0.429856640579741,1.,3.88414070943341));
#49142=CARTESIAN_POINT('Ctrl Pts',(-0.427053541173457,-1.,3.87724240306597));
#49143=CARTESIAN_POINT('Ctrl Pts',(-0.427053541173457,1.,3.87724240306597));
#49144=CARTESIAN_POINT('Ctrl Pts',(-0.424304173195111,-1.,3.87033643487851));
#49145=CARTESIAN_POINT('Ctrl Pts',(-0.424304173195111,1.,3.87033643487851));
#49146=CARTESIAN_POINT('Ctrl Pts',(-0.421607423177534,-1.,3.86339652542709));
#49147=CARTESIAN_POINT('Ctrl Pts',(-0.421607423177534,1.,3.86339652542709));
#49148=CARTESIAN_POINT('Ctrl Pts',(-0.418962468086773,-1.,3.85639825647996));
#49149=CARTESIAN_POINT('Ctrl Pts',(-0.418962468086773,1.,3.85639825647996));
#49150=CARTESIAN_POINT('Ctrl Pts',(-0.416369678052907,-1.,3.84932864157497));
#49151=CARTESIAN_POINT('Ctrl Pts',(-0.416369678052907,1.,3.84932864157497));
#49152=CARTESIAN_POINT('Ctrl Pts',(-0.413831367016748,-1.,3.84219403994762));
#49153=CARTESIAN_POINT('Ctrl Pts',(-0.413831367016748,1.,3.84219403994762));
#49154=CARTESIAN_POINT('Ctrl Pts',(-0.411353038798519,-1.,3.83503345578698));
#49155=CARTESIAN_POINT('Ctrl Pts',(-0.411353038798519,1.,3.83503345578698));
#49156=CARTESIAN_POINT('Ctrl Pts',(-0.40894237144746,-1.,3.82790724256471));
#49157=CARTESIAN_POINT('Ctrl Pts',(-0.40894237144746,1.,3.82790724256471));
#49158=CARTESIAN_POINT('Ctrl Pts',(-0.406607038258985,-1.,3.8208730391381));
#49159=CARTESIAN_POINT('Ctrl Pts',(-0.406607038258985,1.,3.8208730391381));
#49160=CARTESIAN_POINT('Ctrl Pts',(-0.404352694628273,-1.,3.81396374287793));
#49161=CARTESIAN_POINT('Ctrl Pts',(-0.404352694628273,1.,3.81396374287793));
#49162=CARTESIAN_POINT('Ctrl Pts',(-0.402181320148436,-1.,3.80716881962728));
#49163=CARTESIAN_POINT('Ctrl Pts',(-0.402181320148436,1.,3.80716881962728));
#49164=CARTESIAN_POINT('Ctrl Pts',(-0.4000883465046,-1.,3.80040370384546));
#49165=CARTESIAN_POINT('Ctrl Pts',(-0.4000883465046,1.,3.80040370384546));
#49166=CARTESIAN_POINT('Ctrl Pts',(-0.39806481868397,-1.,3.7935288716329));
#49167=CARTESIAN_POINT('Ctrl Pts',(-0.39806481868397,1.,3.7935288716329));
#49168=CARTESIAN_POINT('Ctrl Pts',(-0.396103205334841,-1.,3.78640521279313));
#49169=CARTESIAN_POINT('Ctrl Pts',(-0.396103205334841,1.,3.78640521279313));
#49170=CARTESIAN_POINT('Ctrl Pts',(-0.394202481011499,-1.,3.77894173114283));
#49171=CARTESIAN_POINT('Ctrl Pts',(-0.394202481011499,1.,3.77894173114283));
#49172=CARTESIAN_POINT('Ctrl Pts',(-0.392372786223433,-1.,3.77114011595967));
#49173=CARTESIAN_POINT('Ctrl Pts',(-0.392372786223433,1.,3.77114011595967));
#49174=CARTESIAN_POINT('Ctrl Pts',(-0.39064207297956,-1.,3.76315635033257));
#49175=CARTESIAN_POINT('Ctrl Pts',(-0.39064207297956,1.,3.76315635033257));
#49176=CARTESIAN_POINT('Ctrl Pts',(-0.389054775898702,-1.,3.75529302895152));
#49177=CARTESIAN_POINT('Ctrl Pts',(-0.389054775898702,1.,3.75529302895152));
#49178=CARTESIAN_POINT('Ctrl Pts',(-0.387663020050836,-1.,3.74792651696654));
#49179=CARTESIAN_POINT('Ctrl Pts',(-0.387663020050836,1.,3.74792651696654));
#49180=CARTESIAN_POINT('Ctrl Pts',(-0.386519576222251,-1.,3.74144965781276));
#49181=CARTESIAN_POINT('Ctrl Pts',(-0.386519576222251,1.,3.74144965781276));
#49182=CARTESIAN_POINT('Ctrl Pts',(-0.385670806454566,-1.,3.73621371845318));
#49183=CARTESIAN_POINT('Ctrl Pts',(-0.385670806454566,1.,3.73621371845318));
#49184=CARTESIAN_POINT('Ctrl Pts',(-0.385147887988951,-1.,3.73245705638843));
#49185=CARTESIAN_POINT('Ctrl Pts',(-0.385147887988951,1.,3.73245705638843));
#49186=CARTESIAN_POINT('Ctrl Pts',(-0.385001870183213,-1.,3.73072465900175));
#49187=CARTESIAN_POINT('Ctrl Pts',(-0.385001870183213,1.,3.73072465900175));
#49188=CARTESIAN_POINT('Ctrl Pts',(-0.385047711603462,-1.,3.73015851028356));
#49189=CARTESIAN_POINT('Ctrl Pts',(-0.385047711603462,1.,3.73015851028356));
#49190=CARTESIAN_POINT('Ctrl Pts',(-0.385147278814642,-1.,3.73010668803042));
#49191=CARTESIAN_POINT('Ctrl Pts',(-0.385147278814642,1.,3.73010668803042));
#49192=CARTESIAN_POINT('Ctrl Pts',(-0.38521431477633,-1.,3.73016218570874));
#49193=CARTESIAN_POINT('Ctrl Pts',(-0.38521431477633,1.,3.73016218570874));
#49194=CARTESIAN_POINT('',(-0.581791163835815,1.,4.15950947128175));
#49195=CARTESIAN_POINT('Ctrl Pts',(-0.581791163835815,1.,4.15950947128175));
#49196=CARTESIAN_POINT('Ctrl Pts',(-0.580901211463535,1.,4.1582129171283));
#49197=CARTESIAN_POINT('Ctrl Pts',(-0.579124568914235,1.,4.15561864788576));
#49198=CARTESIAN_POINT('Ctrl Pts',(-0.576469391676688,1.,4.151723761217));
#49199=CARTESIAN_POINT('Ctrl Pts',(-0.572948736069522,1.,4.14652361068081));
#49200=CARTESIAN_POINT('Ctrl Pts',(-0.568580610189775,1.,4.14001179830547));
#49201=CARTESIAN_POINT('Ctrl Pts',(-0.564245279537149,1.,4.13348835727104));
#49202=CARTESIAN_POINT('Ctrl Pts',(-0.559942890594774,1.,4.12695329951961));
#49203=CARTESIAN_POINT('Ctrl Pts',(-0.555673636129977,1.,4.12040666195664));
#49204=CARTESIAN_POINT('Ctrl Pts',(-0.551437758497033,1.,4.11384852024721));
#49205=CARTESIAN_POINT('Ctrl Pts',(-0.547235539485637,1.,4.10727897027977));
#49206=CARTESIAN_POINT('Ctrl Pts',(-0.543067286877757,1.,4.10069810243979));
#49207=CARTESIAN_POINT('Ctrl Pts',(-0.538933321179756,1.,4.09410597627));
#49208=CARTESIAN_POINT('Ctrl Pts',(-0.534833963477273,1.,4.08750259988885));
#49209=CARTESIAN_POINT('Ctrl Pts',(-0.530769518728571,1.,4.08088789536836));
#49210=CARTESIAN_POINT('Ctrl Pts',(-0.526740277227498,1.,4.07426172299847));
#49211=CARTESIAN_POINT('Ctrl Pts',(-0.522746528603107,1.,4.06762394471314));
#49212=CARTESIAN_POINT('Ctrl Pts',(-0.518788572336924,1.,4.06097448038013));
#49213=CARTESIAN_POINT('Ctrl Pts',(-0.514866728193017,1.,4.05431335771199));
#49214=CARTESIAN_POINT('Ctrl Pts',(-0.51098134921897,1.,4.04764078815447));
#49215=CARTESIAN_POINT('Ctrl Pts',(-0.507132823288136,1.,4.04095715148915));
#49216=CARTESIAN_POINT('Ctrl Pts',(-0.503321556915346,1.,4.03426284174272));
#49217=CARTESIAN_POINT('Ctrl Pts',(-0.499547962340821,1.,4.02755813980101));
#49218=CARTESIAN_POINT('Ctrl Pts',(-0.495812444326251,1.,4.02084308851832));
#49219=CARTESIAN_POINT('Ctrl Pts',(-0.492115383418018,1.,4.01411733503546));
#49220=CARTESIAN_POINT('Ctrl Pts',(-0.488457130424633,1.,4.0073800839099));
#49221=CARTESIAN_POINT('Ctrl Pts',(-0.484838042421835,1.,4.00063045119288));
#49222=CARTESIAN_POINT('Ctrl Pts',(-0.481258512209675,1.,3.99386775880679));
#49223=CARTESIAN_POINT('Ctrl Pts',(-0.477718999122027,1.,3.98709184306738));
#49224=CARTESIAN_POINT('Ctrl Pts',(-0.47422006101951,1.,3.98030338044409));
#49225=CARTESIAN_POINT('Ctrl Pts',(-0.470762379613439,1.,3.97350414289392));
#49226=CARTESIAN_POINT('Ctrl Pts',(-0.467346690880643,1.,3.9666962227393));
#49227=CARTESIAN_POINT('Ctrl Pts',(-0.463973722115733,1.,3.95988133243538));
#49228=CARTESIAN_POINT('Ctrl Pts',(-0.460644124429121,1.,3.95306005817364));
#49229=CARTESIAN_POINT('Ctrl Pts',(-0.457358410451683,1.,3.94623117206678));
#49230=CARTESIAN_POINT('Ctrl Pts',(-0.454116879027584,1.,3.93939080846298));
#49231=CARTESIAN_POINT('Ctrl Pts',(-0.450919768356348,1.,3.93253407403123));
#49232=CARTESIAN_POINT('Ctrl Pts',(-0.447767416837293,1.,3.92565674143416));
#49233=CARTESIAN_POINT('Ctrl Pts',(-0.444660430230591,1.,3.91875701610719));
#49234=CARTESIAN_POINT('Ctrl Pts',(-0.441599824524054,1.,3.91183704069153));
#49235=CARTESIAN_POINT('Ctrl Pts',(-0.43858723545825,1.,3.90490512938563));
#49236=CARTESIAN_POINT('Ctrl Pts',(-0.435624629433528,1.,3.89797256655462));
#49237=CARTESIAN_POINT('Ctrl Pts',(-0.432713929544458,1.,3.89104947940611));
#49238=CARTESIAN_POINT('Ctrl Pts',(-0.429856640579741,1.,3.88414070943341));
#49239=CARTESIAN_POINT('Ctrl Pts',(-0.427053541173457,1.,3.87724240306597));
#49240=CARTESIAN_POINT('Ctrl Pts',(-0.424304173195111,1.,3.87033643487851));
#49241=CARTESIAN_POINT('Ctrl Pts',(-0.421607423177534,1.,3.86339652542709));
#49242=CARTESIAN_POINT('Ctrl Pts',(-0.418962468086773,1.,3.85639825647996));
#49243=CARTESIAN_POINT('Ctrl Pts',(-0.416369678052907,1.,3.84932864157497));
#49244=CARTESIAN_POINT('Ctrl Pts',(-0.413831367016748,1.,3.84219403994762));
#49245=CARTESIAN_POINT('Ctrl Pts',(-0.411353038798519,1.,3.83503345578698));
#49246=CARTESIAN_POINT('Ctrl Pts',(-0.40894237144746,1.,3.82790724256471));
#49247=CARTESIAN_POINT('Ctrl Pts',(-0.406607038258985,1.,3.8208730391381));
#49248=CARTESIAN_POINT('Ctrl Pts',(-0.404352694628273,1.,3.81396374287793));
#49249=CARTESIAN_POINT('Ctrl Pts',(-0.402181320148436,1.,3.80716881962728));
#49250=CARTESIAN_POINT('Ctrl Pts',(-0.4000883465046,1.,3.80040370384546));
#49251=CARTESIAN_POINT('Ctrl Pts',(-0.39806481868397,1.,3.7935288716329));
#49252=CARTESIAN_POINT('Ctrl Pts',(-0.396103205334841,1.,3.78640521279313));
#49253=CARTESIAN_POINT('Ctrl Pts',(-0.394202481011499,1.,3.77894173114283));
#49254=CARTESIAN_POINT('Ctrl Pts',(-0.392372786223433,1.,3.77114011595967));
#49255=CARTESIAN_POINT('Ctrl Pts',(-0.39064207297956,1.,3.76315635033257));
#49256=CARTESIAN_POINT('Ctrl Pts',(-0.389054775898702,1.,3.75529302895152));
#49257=CARTESIAN_POINT('Ctrl Pts',(-0.387663020050836,1.,3.74792651696654));
#49258=CARTESIAN_POINT('Ctrl Pts',(-0.386519576222251,1.,3.74144965781276));
#49259=CARTESIAN_POINT('Ctrl Pts',(-0.385670806454566,1.,3.73621371845318));
#49260=CARTESIAN_POINT('Ctrl Pts',(-0.385187124634206,1.,3.73273893363406));
#49261=CARTESIAN_POINT('Ctrl Pts',(-0.385031656499164,1.,3.73106082862548));
#49262=CARTESIAN_POINT('Ctrl Pts',(-0.385037797881504,1.,3.73040527621055));
#49263=CARTESIAN_POINT('Ctrl Pts',(-0.385087139000375,1.,3.73021431755274));
#49264=CARTESIAN_POINT('Ctrl Pts',(-0.385112848330762,1.,3.73017266276651));
#49265=CARTESIAN_POINT('',(-0.581791163835815,0.,4.15950947128175));
#49266=CARTESIAN_POINT('Ctrl Pts',(-0.7863229229206,-1.,3.66663282329846));
#49267=CARTESIAN_POINT('Ctrl Pts',(-0.7863229229206,1.,3.66663282329846));
#49268=CARTESIAN_POINT('Ctrl Pts',(-0.786369528183326,-1.,3.66655932661986));
#49269=CARTESIAN_POINT('Ctrl Pts',(-0.786369528183326,1.,3.66655932661986));
#49270=CARTESIAN_POINT('Ctrl Pts',(-0.786480236185697,-1.,3.66657784455334));
#49271=CARTESIAN_POINT('Ctrl Pts',(-0.786480236185697,1.,3.66657784455334));
#49272=CARTESIAN_POINT('Ctrl Pts',(-0.786698783542764,-1.,3.66710211820482));
#49273=CARTESIAN_POINT('Ctrl Pts',(-0.786698783542764,1.,3.66710211820482));
#49274=CARTESIAN_POINT('Ctrl Pts',(-0.787095252590501,-1.,3.66879484801113));
#49275=CARTESIAN_POINT('Ctrl Pts',(-0.787095252590501,1.,3.66879484801113));
#49276=CARTESIAN_POINT('Ctrl Pts',(-0.787758799995743,-1.,3.67252923663655));
#49277=CARTESIAN_POINT('Ctrl Pts',(-0.787758799995743,1.,3.67252923663655));
#49278=CARTESIAN_POINT('Ctrl Pts',(-0.788569566220285,-1.,3.67777119516252));
#49279=CARTESIAN_POINT('Ctrl Pts',(-0.788569566220285,1.,3.67777119516252));
#49280=CARTESIAN_POINT('Ctrl Pts',(-0.789483546064387,-1.,3.68428439783905));
#49281=CARTESIAN_POINT('Ctrl Pts',(-0.789483546064387,1.,3.68428439783905));
#49282=CARTESIAN_POINT('Ctrl Pts',(-0.790436284988788,-1.,3.69172044327364));
#49283=CARTESIAN_POINT('Ctrl Pts',(-0.790436284988788,1.,3.69172044327364));
#49284=CARTESIAN_POINT('Ctrl Pts',(-0.79135657569598,-1.,3.69968940808721));
#49285=CARTESIAN_POINT('Ctrl Pts',(-0.79135657569598,1.,3.69968940808721));
#49286=CARTESIAN_POINT('Ctrl Pts',(-0.792177688845818,-1.,3.70781724021806));
#49287=CARTESIAN_POINT('Ctrl Pts',(-0.792177688845818,1.,3.70781724021806));
#49288=CARTESIAN_POINT('Ctrl Pts',(-0.792848377370287,-1.,3.71580242396124));
#49289=CARTESIAN_POINT('Ctrl Pts',(-0.792848377370287,1.,3.71580242396124));
#49290=CARTESIAN_POINT('Ctrl Pts',(-0.793347023784205,-1.,3.72348797293734));
#49291=CARTESIAN_POINT('Ctrl Pts',(-0.793347023784205,1.,3.72348797293734));
#49292=CARTESIAN_POINT('Ctrl Pts',(-0.793682750269684,-1.,3.73086914695805));
#49293=CARTESIAN_POINT('Ctrl Pts',(-0.793682750269684,1.,3.73086914695805));
#49294=CARTESIAN_POINT('Ctrl Pts',(-0.793882700937017,-1.,3.73803280541687));
#49295=CARTESIAN_POINT('Ctrl Pts',(-0.793882700937017,1.,3.73803280541687));
#49296=CARTESIAN_POINT('Ctrl Pts',(-0.793982700459952,-1.,3.74511357728861));
#49297=CARTESIAN_POINT('Ctrl Pts',(-0.793982700459952,1.,3.74511357728861));
#49298=CARTESIAN_POINT('Ctrl Pts',(-0.794017347371377,-1.,3.75224692493864));
#49299=CARTESIAN_POINT('Ctrl Pts',(-0.794017347371377,1.,3.75224692493864));
#49300=CARTESIAN_POINT('Ctrl Pts',(-0.794008429134907,-1.,3.75951468666257));
#49301=CARTESIAN_POINT('Ctrl Pts',(-0.794008429134907,1.,3.75951468666257));
#49302=CARTESIAN_POINT('Ctrl Pts',(-0.793961083688992,-1.,3.76692626931111));
#49303=CARTESIAN_POINT('Ctrl Pts',(-0.793961083688992,1.,3.76692626931111));
#49304=CARTESIAN_POINT('Ctrl Pts',(-0.793870523787408,-1.,3.77444863801212));
#49305=CARTESIAN_POINT('Ctrl Pts',(-0.793870523787408,1.,3.77444863801212));
#49306=CARTESIAN_POINT('Ctrl Pts',(-0.7937262357813,-1.,3.78202460377598));
#49307=CARTESIAN_POINT('Ctrl Pts',(-0.7937262357813,1.,3.78202460377598));
#49308=CARTESIAN_POINT('Ctrl Pts',(-0.793516871680993,-1.,3.78959439439235));
#49309=CARTESIAN_POINT('Ctrl Pts',(-0.793516871680993,1.,3.78959439439235));
#49310=CARTESIAN_POINT('Ctrl Pts',(-0.793235612973273,-1.,3.79711921389897));
#49311=CARTESIAN_POINT('Ctrl Pts',(-0.793235612973273,1.,3.79711921389897));
#49312=CARTESIAN_POINT('Ctrl Pts',(-0.792882695234778,-1.,3.80459229925637));
#49313=CARTESIAN_POINT('Ctrl Pts',(-0.792882695234778,1.,3.80459229925637));
#49314=CARTESIAN_POINT('Ctrl Pts',(-0.792462483517634,-1.,3.81202588694756));
#49315=CARTESIAN_POINT('Ctrl Pts',(-0.792462483517634,1.,3.81202588694756));
#49316=CARTESIAN_POINT('Ctrl Pts',(-0.791981740718635,-1.,3.81944345442249));
#49317=CARTESIAN_POINT('Ctrl Pts',(-0.791981740718635,1.,3.81944345442249));
#49318=CARTESIAN_POINT('Ctrl Pts',(-0.791447528662369,-1.,3.82687033899792));
#49319=CARTESIAN_POINT('Ctrl Pts',(-0.791447528662369,1.,3.82687033899792));
#49320=CARTESIAN_POINT('Ctrl Pts',(-0.790865012705301,-1.,3.83432392054786));
#49321=CARTESIAN_POINT('Ctrl Pts',(-0.790865012705301,1.,3.83432392054786));
#49322=CARTESIAN_POINT('Ctrl Pts',(-0.790236124191242,-1.,3.84180762342454));
#49323=CARTESIAN_POINT('Ctrl Pts',(-0.790236124191242,1.,3.84180762342454));
#49324=CARTESIAN_POINT('Ctrl Pts',(-0.789560798155582,-1.,3.84931637808894));
#49325=CARTESIAN_POINT('Ctrl Pts',(-0.789560798155582,1.,3.84931637808894));
#49326=CARTESIAN_POINT('Ctrl Pts',(-0.788837734090672,-1.,3.85683995872529));
#49327=CARTESIAN_POINT('Ctrl Pts',(-0.788837734090672,1.,3.85683995872529));
#49328=CARTESIAN_POINT('Ctrl Pts',(-0.788065315093778,-1.,3.86436702561345));
#49329=CARTESIAN_POINT('Ctrl Pts',(-0.788065315093778,1.,3.86436702561345));
#49330=CARTESIAN_POINT('Ctrl Pts',(-0.787242527617999,-1.,3.87188916600912));
#49331=CARTESIAN_POINT('Ctrl Pts',(-0.787242527617999,1.,3.87188916600912));
#49332=CARTESIAN_POINT('Ctrl Pts',(-0.786369675812609,-1.,3.8794040281819));
#49333=CARTESIAN_POINT('Ctrl Pts',(-0.786369675812609,1.,3.8794040281819));
#49334=CARTESIAN_POINT('Ctrl Pts',(-0.78544789034073,-1.,3.88691313167398));
#49335=CARTESIAN_POINT('Ctrl Pts',(-0.78544789034073,1.,3.88691313167398));
#49336=CARTESIAN_POINT('Ctrl Pts',(-0.784478799358336,-1.,3.89442039235103));
#49337=CARTESIAN_POINT('Ctrl Pts',(-0.784478799358336,1.,3.89442039235103));
#49338=CARTESIAN_POINT('Ctrl Pts',(-0.783464141529081,-1.,3.9019303904397));
#49339=CARTESIAN_POINT('Ctrl Pts',(-0.783464141529081,1.,3.9019303904397));
#49340=CARTESIAN_POINT('Ctrl Pts',(-0.782405395622764,-1.,3.90944671004542));
#49341=CARTESIAN_POINT('Ctrl Pts',(-0.782405395622764,1.,3.90944671004542));
#49342=CARTESIAN_POINT('Ctrl Pts',(-0.781303428618367,-1.,3.91697036054676));
#49343=CARTESIAN_POINT('Ctrl Pts',(-0.781303428618367,1.,3.91697036054676));
#49344=CARTESIAN_POINT('Ctrl Pts',(-0.780158678615543,-1.,3.92450058323823));
#49345=CARTESIAN_POINT('Ctrl Pts',(-0.780158678615543,1.,3.92450058323823));
#49346=CARTESIAN_POINT('Ctrl Pts',(-0.778971308134821,-1.,3.93203552473174));
#49347=CARTESIAN_POINT('Ctrl Pts',(-0.778971308134821,1.,3.93203552473174));
#49348=CARTESIAN_POINT('Ctrl Pts',(-0.777741370568559,-1.,3.93957296768103));
#49349=CARTESIAN_POINT('Ctrl Pts',(-0.777741370568559,1.,3.93957296768103));
#49350=CARTESIAN_POINT('Ctrl Pts',(-0.776468966697921,-1.,3.94711101619447));
#49351=CARTESIAN_POINT('Ctrl Pts',(-0.776468966697921,1.,3.94711101619447));
#49352=CARTESIAN_POINT('Ctrl Pts',(-0.775154418039352,-1.,3.9546488545231));
#49353=CARTESIAN_POINT('Ctrl Pts',(-0.775154418039352,1.,3.9546488545231));
#49354=CARTESIAN_POINT('Ctrl Pts',(-0.773798212026566,-1.,3.96218649639807));
#49355=CARTESIAN_POINT('Ctrl Pts',(-0.773798212026566,1.,3.96218649639807));
#49356=CARTESIAN_POINT('Ctrl Pts',(-0.772400931772136,-1.,3.96972446532772));
#49357=CARTESIAN_POINT('Ctrl Pts',(-0.772400931772136,1.,3.96972446532772));
#49358=CARTESIAN_POINT('Ctrl Pts',(-0.770963190030471,-1.,3.97726349165488));
#49359=CARTESIAN_POINT('Ctrl Pts',(-0.770963190030471,1.,3.97726349165488));
#49360=CARTESIAN_POINT('Ctrl Pts',(-0.769485566245544,-1.,3.98480422348451));
#49361=CARTESIAN_POINT('Ctrl Pts',(-0.769485566245544,1.,3.98480422348451));
#49362=CARTESIAN_POINT('Ctrl Pts',(-0.767968531377915,-1.,3.9923468788101));
#49363=CARTESIAN_POINT('Ctrl Pts',(-0.767968531377915,1.,3.9923468788101));
#49364=CARTESIAN_POINT('Ctrl Pts',(-0.766412457136064,-1.,3.99989129179622));
#49365=CARTESIAN_POINT('Ctrl Pts',(-0.766412457136064,1.,3.99989129179622));
#49366=CARTESIAN_POINT('Ctrl Pts',(-0.764817648785198,-1.,4.00743706791509));
#49367=CARTESIAN_POINT('Ctrl Pts',(-0.764817648785198,1.,4.00743706791509));
#49368=CARTESIAN_POINT('Ctrl Pts',(-0.763184371182935,-1.,4.01498370680496));
#49369=CARTESIAN_POINT('Ctrl Pts',(-0.763184371182935,1.,4.01498370680496));
#49370=CARTESIAN_POINT('Ctrl Pts',(-0.761512875859804,-1.,4.02253072741268));
#49371=CARTESIAN_POINT('Ctrl Pts',(-0.761512875859804,1.,4.02253072741268));
#49372=CARTESIAN_POINT('Ctrl Pts',(-0.759803433243752,-1.,4.03007781954412));
#49373=CARTESIAN_POINT('Ctrl Pts',(-0.759803433243752,1.,4.03007781954412));
#49374=CARTESIAN_POINT('Ctrl Pts',(-0.758056338884944,-1.,4.03762485803119));
#49375=CARTESIAN_POINT('Ctrl Pts',(-0.758056338884944,1.,4.03762485803119));
#49376=CARTESIAN_POINT('Ctrl Pts',(-0.756271902369581,-1.,4.04517182653997));
#49377=CARTESIAN_POINT('Ctrl Pts',(-0.756271902369581,1.,4.04517182653997));
#49378=CARTESIAN_POINT('Ctrl Pts',(-0.754450441816078,-1.,4.05271876687915));
#49379=CARTESIAN_POINT('Ctrl Pts',(-0.754450441816078,1.,4.05271876687915));
#49380=CARTESIAN_POINT('Ctrl Pts',(-0.752592276483072,-1.,4.06026572221515));
#49381=CARTESIAN_POINT('Ctrl Pts',(-0.752592276483072,1.,4.06026572221515));
#49382=CARTESIAN_POINT('Ctrl Pts',(-0.750697720484036,-1.,4.06781267242378));
#49383=CARTESIAN_POINT('Ctrl Pts',(-0.750697720484036,1.,4.06781267242378));
#49384=CARTESIAN_POINT('Ctrl Pts',(-0.748767076680557,-1.,4.07535951056152));
#49385=CARTESIAN_POINT('Ctrl Pts',(-0.748767076680557,1.,4.07535951056152));
#49386=CARTESIAN_POINT('Ctrl Pts',(-0.746800631492315,-1.,4.08290608095642));
#49387=CARTESIAN_POINT('Ctrl Pts',(-0.746800631492315,1.,4.08290608095642));
#49388=CARTESIAN_POINT('Ctrl Pts',(-0.7447986497065,-1.,4.09045220253573));
#49389=CARTESIAN_POINT('Ctrl Pts',(-0.7447986497065,1.,4.09045220253573));
#49390=CARTESIAN_POINT('Ctrl Pts',(-0.742761369689841,-1.,4.09799769702611));
#49391=CARTESIAN_POINT('Ctrl Pts',(-0.742761369689841,1.,4.09799769702611));
#49392=CARTESIAN_POINT('Ctrl Pts',(-0.740688998553377,-1.,4.10554241757547));
#49393=CARTESIAN_POINT('Ctrl Pts',(-0.740688998553377,1.,4.10554241757547));
#49394=CARTESIAN_POINT('Ctrl Pts',(-0.738581708225844,-1.,4.11308626951927));
#49395=CARTESIAN_POINT('Ctrl Pts',(-0.738581708225844,1.,4.11308626951927));
#49396=CARTESIAN_POINT('Ctrl Pts',(-0.736439634331345,-1.,4.120629196238));
#49397=CARTESIAN_POINT('Ctrl Pts',(-0.736439634331345,1.,4.120629196238));
#49398=CARTESIAN_POINT('Ctrl Pts',(-0.734698226764092,-1.,4.12666277570844));
#49399=CARTESIAN_POINT('Ctrl Pts',(-0.734698226764092,1.,4.12666277570844));
#49400=CARTESIAN_POINT('Ctrl Pts',(-0.733376589323546,-1.,4.13118752795207));
#49401=CARTESIAN_POINT('Ctrl Pts',(-0.733376589323546,1.,4.13118752795207));
#49402=CARTESIAN_POINT('Ctrl Pts',(-0.73248857513516,-1.,4.1342038373684));
#49403=CARTESIAN_POINT('Ctrl Pts',(-0.73248857513516,1.,4.1342038373684));
#49404=CARTESIAN_POINT('Ctrl Pts',(-0.73204283740062,-1.,4.13571194405636));
#49405=CARTESIAN_POINT('Ctrl Pts',(-0.73204283740062,1.,4.13571194405636));
#49406=CARTESIAN_POINT('',(-0.786422660831985,1.,3.66661143271685));
#49407=CARTESIAN_POINT('Ctrl Pts',(-0.786422660831985,-1.,3.66661143271685));
#49408=CARTESIAN_POINT('Ctrl Pts',(-0.786422660831985,-0.666666666666667,
3.66661143271685));
#49409=CARTESIAN_POINT('Ctrl Pts',(-0.786422660831985,-0.333333333333333,
3.66661143271685));
#49410=CARTESIAN_POINT('Ctrl Pts',(-0.786422660831985,0.333333333333333,
3.66661143271685));
#49411=CARTESIAN_POINT('Ctrl Pts',(-0.786422660831985,0.666666666666667,
3.66661143271685));
#49412=CARTESIAN_POINT('Ctrl Pts',(-0.786422660831985,1.,3.66661143271685));
#49413=CARTESIAN_POINT('',(-0.73204283740062,1.,4.13571194405636));
#49414=CARTESIAN_POINT('',(-0.73204283740062,0.,4.13571194405636));
#49415=CARTESIAN_POINT('Ctrl Pts',(-0.786422660831985,1.,3.66661143271685));
#49416=CARTESIAN_POINT('Ctrl Pts',(-0.786459983895432,1.,3.6666431041522));
#49417=CARTESIAN_POINT('Ctrl Pts',(-0.786565919558984,1.,3.66680946938292));
#49418=CARTESIAN_POINT('Ctrl Pts',(-0.786774337198062,1.,3.66743103898702));
#49419=CARTESIAN_POINT('Ctrl Pts',(-0.787145041181546,1.,3.66907505398677));
#49420=CARTESIAN_POINT('Ctrl Pts',(-0.787758799995743,1.,3.67252923663655));
#49421=CARTESIAN_POINT('Ctrl Pts',(-0.788569566220285,1.,3.67777119516252));
#49422=CARTESIAN_POINT('Ctrl Pts',(-0.789483546064387,1.,3.68428439783905));
#49423=CARTESIAN_POINT('Ctrl Pts',(-0.790436284988788,1.,3.69172044327364));
#49424=CARTESIAN_POINT('Ctrl Pts',(-0.79135657569598,1.,3.69968940808721));
#49425=CARTESIAN_POINT('Ctrl Pts',(-0.792177688845818,1.,3.70781724021806));
#49426=CARTESIAN_POINT('Ctrl Pts',(-0.792848377370287,1.,3.71580242396124));
#49427=CARTESIAN_POINT('Ctrl Pts',(-0.793347023784205,1.,3.72348797293734));
#49428=CARTESIAN_POINT('Ctrl Pts',(-0.793682750269684,1.,3.73086914695805));
#49429=CARTESIAN_POINT('Ctrl Pts',(-0.793882700937017,1.,3.73803280541687));
#49430=CARTESIAN_POINT('Ctrl Pts',(-0.793982700459952,1.,3.74511357728861));
#49431=CARTESIAN_POINT('Ctrl Pts',(-0.794017347371377,1.,3.75224692493864));
#49432=CARTESIAN_POINT('Ctrl Pts',(-0.794008429134907,1.,3.75951468666257));
#49433=CARTESIAN_POINT('Ctrl Pts',(-0.793961083688992,1.,3.76692626931111));
#49434=CARTESIAN_POINT('Ctrl Pts',(-0.793870523787408,1.,3.77444863801212));
#49435=CARTESIAN_POINT('Ctrl Pts',(-0.7937262357813,1.,3.78202460377598));
#49436=CARTESIAN_POINT('Ctrl Pts',(-0.793516871680993,1.,3.78959439439235));
#49437=CARTESIAN_POINT('Ctrl Pts',(-0.793235612973273,1.,3.79711921389897));
#49438=CARTESIAN_POINT('Ctrl Pts',(-0.792882695234778,1.,3.80459229925637));
#49439=CARTESIAN_POINT('Ctrl Pts',(-0.792462483517634,1.,3.81202588694756));
#49440=CARTESIAN_POINT('Ctrl Pts',(-0.791981740718635,1.,3.81944345442249));
#49441=CARTESIAN_POINT('Ctrl Pts',(-0.791447528662369,1.,3.82687033899792));
#49442=CARTESIAN_POINT('Ctrl Pts',(-0.790865012705301,1.,3.83432392054786));
#49443=CARTESIAN_POINT('Ctrl Pts',(-0.790236124191242,1.,3.84180762342454));
#49444=CARTESIAN_POINT('Ctrl Pts',(-0.789560798155582,1.,3.84931637808894));
#49445=CARTESIAN_POINT('Ctrl Pts',(-0.788837734090672,1.,3.85683995872529));
#49446=CARTESIAN_POINT('Ctrl Pts',(-0.788065315093778,1.,3.86436702561345));
#49447=CARTESIAN_POINT('Ctrl Pts',(-0.787242527617999,1.,3.87188916600912));
#49448=CARTESIAN_POINT('Ctrl Pts',(-0.786369675812609,1.,3.8794040281819));
#49449=CARTESIAN_POINT('Ctrl Pts',(-0.78544789034073,1.,3.88691313167398));
#49450=CARTESIAN_POINT('Ctrl Pts',(-0.784478799358336,1.,3.89442039235103));
#49451=CARTESIAN_POINT('Ctrl Pts',(-0.783464141529081,1.,3.9019303904397));
#49452=CARTESIAN_POINT('Ctrl Pts',(-0.782405395622764,1.,3.90944671004542));
#49453=CARTESIAN_POINT('Ctrl Pts',(-0.781303428618367,1.,3.91697036054676));
#49454=CARTESIAN_POINT('Ctrl Pts',(-0.780158678615543,1.,3.92450058323823));
#49455=CARTESIAN_POINT('Ctrl Pts',(-0.778971308134821,1.,3.93203552473174));
#49456=CARTESIAN_POINT('Ctrl Pts',(-0.777741370568559,1.,3.93957296768103));
#49457=CARTESIAN_POINT('Ctrl Pts',(-0.776468966697921,1.,3.94711101619447));
#49458=CARTESIAN_POINT('Ctrl Pts',(-0.775154418039352,1.,3.9546488545231));
#49459=CARTESIAN_POINT('Ctrl Pts',(-0.773798212026566,1.,3.96218649639807));
#49460=CARTESIAN_POINT('Ctrl Pts',(-0.772400931772136,1.,3.96972446532772));
#49461=CARTESIAN_POINT('Ctrl Pts',(-0.770963190030471,1.,3.97726349165488));
#49462=CARTESIAN_POINT('Ctrl Pts',(-0.769485566245544,1.,3.98480422348451));
#49463=CARTESIAN_POINT('Ctrl Pts',(-0.767968531377915,1.,3.9923468788101));
#49464=CARTESIAN_POINT('Ctrl Pts',(-0.766412457136064,1.,3.99989129179622));
#49465=CARTESIAN_POINT('Ctrl Pts',(-0.764817648785198,1.,4.00743706791509));
#49466=CARTESIAN_POINT('Ctrl Pts',(-0.763184371182935,1.,4.01498370680496));
#49467=CARTESIAN_POINT('Ctrl Pts',(-0.761512875859804,1.,4.02253072741268));
#49468=CARTESIAN_POINT('Ctrl Pts',(-0.759803433243752,1.,4.03007781954412));
#49469=CARTESIAN_POINT('Ctrl Pts',(-0.758056338884944,1.,4.03762485803119));
#49470=CARTESIAN_POINT('Ctrl Pts',(-0.756271902369581,1.,4.04517182653997));
#49471=CARTESIAN_POINT('Ctrl Pts',(-0.754450441816078,1.,4.05271876687915));
#49472=CARTESIAN_POINT('Ctrl Pts',(-0.752592276483072,1.,4.06026572221515));
#49473=CARTESIAN_POINT('Ctrl Pts',(-0.750697720484036,1.,4.06781267242378));
#49474=CARTESIAN_POINT('Ctrl Pts',(-0.748767076680557,1.,4.07535951056152));
#49475=CARTESIAN_POINT('Ctrl Pts',(-0.746800631492315,1.,4.08290608095642));
#49476=CARTESIAN_POINT('Ctrl Pts',(-0.7447986497065,1.,4.09045220253573));
#49477=CARTESIAN_POINT('Ctrl Pts',(-0.742761369689841,1.,4.09799769702611));
#49478=CARTESIAN_POINT('Ctrl Pts',(-0.740688998553377,1.,4.10554241757547));
#49479=CARTESIAN_POINT('Ctrl Pts',(-0.738581708225844,1.,4.11308626951927));
#49480=CARTESIAN_POINT('Ctrl Pts',(-0.736439634331345,1.,4.120629196238));
#49481=CARTESIAN_POINT('Ctrl Pts',(-0.734698226764092,1.,4.12666277570844));
#49482=CARTESIAN_POINT('Ctrl Pts',(-0.733376589323546,1.,4.13118752795207));
#49483=CARTESIAN_POINT('Ctrl Pts',(-0.73248857513516,1.,4.1342038373684));
#49484=CARTESIAN_POINT('Ctrl Pts',(-0.73204283740062,1.,4.13571194405636));
#49485=CARTESIAN_POINT('Origin',(-0.73204283740062,0.,4.13571194405636));
#49486=CARTESIAN_POINT('',(-0.581791163835815,1.,4.15950947128175));
#49487=CARTESIAN_POINT('Origin',(0.,0.,0.));
#49488=CARTESIAN_POINT('',(-0.963899035117249,1.,3.62400312501245));
#49489=CARTESIAN_POINT('Origin',(0.,1.,0.));
#49490=CARTESIAN_POINT('Ctrl Pts',(-0.963899035117249,1.,3.62400312501245));
#49491=CARTESIAN_POINT('Ctrl Pts',(-0.963899035117249,0.666666666666667,
3.62400312501245));
#49492=CARTESIAN_POINT('Ctrl Pts',(-0.963899035117249,0.333333333333333,
3.62400312501245));
#49493=CARTESIAN_POINT('Ctrl Pts',(-0.963899035117249,-0.333333333333333,
3.62400312501245));
#49494=CARTESIAN_POINT('Ctrl Pts',(-0.963899035117249,-0.666666666666667,
3.62400312501245));
#49495=CARTESIAN_POINT('Ctrl Pts',(-0.963899035117249,-1.,3.62400312501245));
#49496=CARTESIAN_POINT('Ctrl Pts',(-1.22531898815164,-1.,4.01728681790024));
#49497=CARTESIAN_POINT('Ctrl Pts',(-1.22531898815164,1.,4.01728681790024));
#49498=CARTESIAN_POINT('Ctrl Pts',(-1.22423716681447,-1.,4.0161454457032));
#49499=CARTESIAN_POINT('Ctrl Pts',(-1.22423716681447,1.,4.0161454457032));
#49500=CARTESIAN_POINT('Ctrl Pts',(-1.22207656456199,-1.,4.01386104434674));
#49501=CARTESIAN_POINT('Ctrl Pts',(-1.22207656456199,1.,4.01386104434674));
#49502=CARTESIAN_POINT('Ctrl Pts',(-1.21884478244983,-1.,4.01042947142681));
#49503=CARTESIAN_POINT('Ctrl Pts',(-1.21884478244983,1.,4.01042947142681));
#49504=CARTESIAN_POINT('Ctrl Pts',(-1.21455398918813,-1.,4.00584409524937));
#49505=CARTESIAN_POINT('Ctrl Pts',(-1.21455398918813,1.,4.00584409524937));
#49506=CARTESIAN_POINT('Ctrl Pts',(-1.20922097030107,-1.,4.00009577952534));
#49507=CARTESIAN_POINT('Ctrl Pts',(-1.20922097030107,1.,4.00009577952534));
#49508=CARTESIAN_POINT('Ctrl Pts',(-1.2039185237544,-1.,3.99433084800649));
#49509=CARTESIAN_POINT('Ctrl Pts',(-1.2039185237544,1.,3.99433084800649));
#49510=CARTESIAN_POINT('Ctrl Pts',(-1.19864679609596,-1.,3.98854928957287));
#49511=CARTESIAN_POINT('Ctrl Pts',(-1.19864679609596,1.,3.98854928957287));
#49512=CARTESIAN_POINT('Ctrl Pts',(-1.19340598349307,-1.,3.98275111052015));
#49513=CARTESIAN_POINT('Ctrl Pts',(-1.19340598349307,1.,3.98275111052015));
#49514=CARTESIAN_POINT('Ctrl Pts',(-1.18819633715285,-1.,3.97693634766926));
#49515=CARTESIAN_POINT('Ctrl Pts',(-1.18819633715285,1.,3.97693634766926));
#49516=CARTESIAN_POINT('Ctrl Pts',(-1.18301815039596,-1.,3.9711050516465));
#49517=CARTESIAN_POINT('Ctrl Pts',(-1.18301815039596,1.,3.9711050516465));
#49518=CARTESIAN_POINT('Ctrl Pts',(-1.17787174135445,-1.,3.96525726357682));
#49519=CARTESIAN_POINT('Ctrl Pts',(-1.17787174135445,1.,3.96525726357682));
#49520=CARTESIAN_POINT('Ctrl Pts',(-1.17275743590327,-1.,3.95939299213164));
#49521=CARTESIAN_POINT('Ctrl Pts',(-1.17275743590327,1.,3.95939299213164));
#49522=CARTESIAN_POINT('Ctrl Pts',(-1.16767555244495,-1.,3.95351219510062));
#49523=CARTESIAN_POINT('Ctrl Pts',(-1.16767555244495,1.,3.95351219510062));
#49524=CARTESIAN_POINT('Ctrl Pts',(-1.16262637999261,-1.,3.9476147478092));
#49525=CARTESIAN_POINT('Ctrl Pts',(-1.16262637999261,1.,3.9476147478092));
#49526=CARTESIAN_POINT('Ctrl Pts',(-1.1576101834106,-1.,3.94170046685542));
#49527=CARTESIAN_POINT('Ctrl Pts',(-1.1576101834106,1.,3.94170046685542));
#49528=CARTESIAN_POINT('Ctrl Pts',(-1.15262722716391,-1.,3.9357691705651));
#49529=CARTESIAN_POINT('Ctrl Pts',(-1.15262722716391,1.,3.9357691705651));
#49530=CARTESIAN_POINT('Ctrl Pts',(-1.14767779451147,-1.,3.92982073294334));
#49531=CARTESIAN_POINT('Ctrl Pts',(-1.14767779451147,1.,3.92982073294334));
#49532=CARTESIAN_POINT('Ctrl Pts',(-1.14276220561575,-1.,3.92385513133937));
#49533=CARTESIAN_POINT('Ctrl Pts',(-1.14276220561575,1.,3.92385513133937));
#49534=CARTESIAN_POINT('Ctrl Pts',(-1.13788084225511,-1.,3.91787251936688));
#49535=CARTESIAN_POINT('Ctrl Pts',(-1.13788084225511,1.,3.91787251936688));
#49536=CARTESIAN_POINT('Ctrl Pts',(-1.13303414693849,-1.,3.91187321145495));
#49537=CARTESIAN_POINT('Ctrl Pts',(-1.13303414693849,1.,3.91187321145495));
#49538=CARTESIAN_POINT('Ctrl Pts',(-1.12822258281518,-1.,3.90585753318622));
#49539=CARTESIAN_POINT('Ctrl Pts',(-1.12822258281518,1.,3.90585753318622));
#49540=CARTESIAN_POINT('Ctrl Pts',(-1.12344660099029,-1.,3.89982569749978));
#49541=CARTESIAN_POINT('Ctrl Pts',(-1.12344660099029,1.,3.89982569749978));
#49542=CARTESIAN_POINT('Ctrl Pts',(-1.11870660794609,-1.,3.89377768340362));
#49543=CARTESIAN_POINT('Ctrl Pts',(-1.11870660794609,1.,3.89377768340362));
#49544=CARTESIAN_POINT('Ctrl Pts',(-1.11400292434447,-1.,3.88771308285229));
#49545=CARTESIAN_POINT('Ctrl Pts',(-1.11400292434447,1.,3.88771308285229));
#49546=CARTESIAN_POINT('Ctrl Pts',(-1.10933577224029,-1.,3.88163105531791));
#49547=CARTESIAN_POINT('Ctrl Pts',(-1.10933577224029,1.,3.88163105531791));
#49548=CARTESIAN_POINT('Ctrl Pts',(-1.10470536603303,-1.,3.87553067187566));
#49549=CARTESIAN_POINT('Ctrl Pts',(-1.10470536603303,1.,3.87553067187566));
#49550=CARTESIAN_POINT('Ctrl Pts',(-1.10011198761202,-1.,3.86941120134872));
#49551=CARTESIAN_POINT('Ctrl Pts',(-1.10011198761202,1.,3.86941120134872));
#49552=CARTESIAN_POINT('Ctrl Pts',(-1.09555606505012,-1.,3.86327241021242));
#49553=CARTESIAN_POINT('Ctrl Pts',(-1.09555606505012,1.,3.86327241021242));
#49554=CARTESIAN_POINT('Ctrl Pts',(-1.09103825516288,-1.,3.85711487933911));
#49555=CARTESIAN_POINT('Ctrl Pts',(-1.09103825516288,1.,3.85711487933911));
#49556=CARTESIAN_POINT('Ctrl Pts',(-1.08655950846377,-1.,3.8509402522269));
#49557=CARTESIAN_POINT('Ctrl Pts',(-1.08655950846377,1.,3.8509402522269));
#49558=CARTESIAN_POINT('Ctrl Pts',(-1.08212087917986,-1.,3.84475048030615));
#49559=CARTESIAN_POINT('Ctrl Pts',(-1.08212087917986,1.,3.84475048030615));
#49560=CARTESIAN_POINT('Ctrl Pts',(-1.07772335353856,-1.,3.83854714117486));
#49561=CARTESIAN_POINT('Ctrl Pts',(-1.07772335353856,1.,3.83854714117486));
#49562=CARTESIAN_POINT('Ctrl Pts',(-1.0733676663346,-1.,3.83233071195145));
#49563=CARTESIAN_POINT('Ctrl Pts',(-1.0733676663346,1.,3.83233071195145));
#49564=CARTESIAN_POINT('Ctrl Pts',(-1.0690541318036,-1.,3.82609989967278));
#49565=CARTESIAN_POINT('Ctrl Pts',(-1.0690541318036,1.,3.82609989967278));
#49566=CARTESIAN_POINT('Ctrl Pts',(-1.06478244038931,-1.,3.81985083953012));
#49567=CARTESIAN_POINT('Ctrl Pts',(-1.06478244038931,1.,3.81985083953012));
#49568=CARTESIAN_POINT('Ctrl Pts',(-1.06055206187298,-1.,3.81357866117485));
#49569=CARTESIAN_POINT('Ctrl Pts',(-1.06055206187298,1.,3.81357866117485));
#49570=CARTESIAN_POINT('Ctrl Pts',(-1.05636266918643,-1.,3.80727913637784));
#49571=CARTESIAN_POINT('Ctrl Pts',(-1.05636266918643,1.,3.80727913637784));
#49572=CARTESIAN_POINT('Ctrl Pts',(-1.05221457990015,-1.,3.80095039790678));
#49573=CARTESIAN_POINT('Ctrl Pts',(-1.05221457990015,1.,3.80095039790678));
#49574=CARTESIAN_POINT('Ctrl Pts',(-1.04810913267641,-1.,3.79459440308793));
#49575=CARTESIAN_POINT('Ctrl Pts',(-1.04810913267641,1.,3.79459440308793));
#49576=CARTESIAN_POINT('Ctrl Pts',(-1.04404924374426,-1.,3.78821910787195));
#49577=CARTESIAN_POINT('Ctrl Pts',(-1.04404924374426,1.,3.78821910787195));
#49578=CARTESIAN_POINT('Ctrl Pts',(-1.04003862055804,-1.,3.78183535008192));
#49579=CARTESIAN_POINT('Ctrl Pts',(-1.04003862055804,1.,3.78183535008192));
#49580=CARTESIAN_POINT('Ctrl Pts',(-1.03608074678013,-1.,3.77545283140445));
#49581=CARTESIAN_POINT('Ctrl Pts',(-1.03608074678013,1.,3.77545283140445));
#49582=CARTESIAN_POINT('Ctrl Pts',(-1.0321778660492,-1.,3.76907609832522));
#49583=CARTESIAN_POINT('Ctrl Pts',(-1.0321778660492,1.,3.76907609832522));
#49584=CARTESIAN_POINT('Ctrl Pts',(-1.02833014458181,-1.,3.76270122291232));
#49585=CARTESIAN_POINT('Ctrl Pts',(-1.02833014458181,1.,3.76270122291232));
#49586=CARTESIAN_POINT('Ctrl Pts',(-1.0245342944466,-1.,3.75631037456194));
#49587=CARTESIAN_POINT('Ctrl Pts',(-1.0245342944466,1.,3.75631037456194));
#49588=CARTESIAN_POINT('Ctrl Pts',(-1.02078510487428,-1.,3.74987777155834));
#49589=CARTESIAN_POINT('Ctrl Pts',(-1.02078510487428,1.,3.74987777155834));
#49590=CARTESIAN_POINT('Ctrl Pts',(-1.01707794311079,-1.,3.74337942504959));
#49591=CARTESIAN_POINT('Ctrl Pts',(-1.01707794311079,1.,3.74337942504959));
#49592=CARTESIAN_POINT('Ctrl Pts',(-1.01341114319903,-1.,3.73680245055734));
#49593=CARTESIAN_POINT('Ctrl Pts',(-1.01341114319903,1.,3.73680245055734));
#49594=CARTESIAN_POINT('Ctrl Pts',(-1.00978798539496,-1.,3.73015276704426));
#49595=CARTESIAN_POINT('Ctrl Pts',(-1.00978798539496,1.,3.73015276704426));
#49596=CARTESIAN_POINT('Ctrl Pts',(-1.0062200073571,-1.,3.72346803750595));
#49597=CARTESIAN_POINT('Ctrl Pts',(-1.0062200073571,1.,3.72346803750595));
#49598=CARTESIAN_POINT('Ctrl Pts',(-1.00272423396822,-1.,3.71680667125118));
#49599=CARTESIAN_POINT('Ctrl Pts',(-1.00272423396822,1.,3.71680667125118));
#49600=CARTESIAN_POINT('Ctrl Pts',(-0.999317260756531,-1.,3.71022439713938));
#49601=CARTESIAN_POINT('Ctrl Pts',(-0.999317260756531,1.,3.71022439713938));
#49602=CARTESIAN_POINT('Ctrl Pts',(-0.996009819772518,-1.,3.70375282282138));
#49603=CARTESIAN_POINT('Ctrl Pts',(-0.996009819772518,1.,3.70375282282138));
#49604=CARTESIAN_POINT('Ctrl Pts',(-0.99280221833201,-1.,3.69738123415662));
#49605=CARTESIAN_POINT('Ctrl Pts',(-0.99280221833201,1.,3.69738123415662));
#49606=CARTESIAN_POINT('Ctrl Pts',(-0.989676715398558,-1.,3.69102682138846));
#49607=CARTESIAN_POINT('Ctrl Pts',(-0.989676715398558,1.,3.69102682138846));
#49608=CARTESIAN_POINT('Ctrl Pts',(-0.986602639863838,-1.,3.68455317926068));
#49609=CARTESIAN_POINT('Ctrl Pts',(-0.986602639863838,1.,3.68455317926068));
#49610=CARTESIAN_POINT('Ctrl Pts',(-0.983550791470419,-1.,3.67782408841715));
#49611=CARTESIAN_POINT('Ctrl Pts',(-0.983550791470419,1.,3.67782408841715));
#49612=CARTESIAN_POINT('Ctrl Pts',(-0.980505922458267,-1.,3.67074983340361));
#49613=CARTESIAN_POINT('Ctrl Pts',(-0.980505922458267,1.,3.67074983340361));
#49614=CARTESIAN_POINT('Ctrl Pts',(-0.977478312751618,-1.,3.66333049637475));
#49615=CARTESIAN_POINT('Ctrl Pts',(-0.977478312751618,1.,3.66333049637475));
#49616=CARTESIAN_POINT('Ctrl Pts',(-0.974519971354848,-1.,3.65571576735126));
#49617=CARTESIAN_POINT('Ctrl Pts',(-0.974519971354848,1.,3.65571576735126));
#49618=CARTESIAN_POINT('Ctrl Pts',(-0.971722122061341,-1.,3.64819756447455));
#49619=CARTESIAN_POINT('Ctrl Pts',(-0.971722122061341,1.,3.64819756447455));
#49620=CARTESIAN_POINT('Ctrl Pts',(-0.969195124675866,-1.,3.64113946505766));
#49621=CARTESIAN_POINT('Ctrl Pts',(-0.969195124675866,1.,3.64113946505766));
#49622=CARTESIAN_POINT('Ctrl Pts',(-0.967052554541386,-1.,3.63492122081143));
#49623=CARTESIAN_POINT('Ctrl Pts',(-0.967052554541386,1.,3.63492122081143));
#49624=CARTESIAN_POINT('Ctrl Pts',(-0.965395153165293,-1.,3.62988252139846));
#49625=CARTESIAN_POINT('Ctrl Pts',(-0.965395153165293,1.,3.62988252139846));
#49626=CARTESIAN_POINT('Ctrl Pts',(-0.964291001273288,-1.,3.62625391254797));
#49627=CARTESIAN_POINT('Ctrl Pts',(-0.964291001273288,1.,3.62625391254797));
#49628=CARTESIAN_POINT('Ctrl Pts',(-0.963875774530619,-1.,3.6245656860652));
#49629=CARTESIAN_POINT('Ctrl Pts',(-0.963875774530619,1.,3.6245656860652));
#49630=CARTESIAN_POINT('Ctrl Pts',(-0.963832486395051,-1.,3.62399933639914));
#49631=CARTESIAN_POINT('Ctrl Pts',(-0.963832486395051,1.,3.62399933639914));
#49632=CARTESIAN_POINT('Ctrl Pts',(-0.963922720982193,-1.,3.62393257642052));
#49633=CARTESIAN_POINT('Ctrl Pts',(-0.963922720982193,1.,3.62393257642052));
#49634=CARTESIAN_POINT('Ctrl Pts',(-0.963997613369571,-1.,3.62397690409552));
#49635=CARTESIAN_POINT('Ctrl Pts',(-0.963997613369571,1.,3.62397690409552));
#49636=CARTESIAN_POINT('',(-1.22531898815164,1.,4.01728681790024));
#49637=CARTESIAN_POINT('Ctrl Pts',(-1.22531898815164,1.,4.01728681790024));
#49638=CARTESIAN_POINT('Ctrl Pts',(-1.22423716681447,1.,4.0161454457032));
#49639=CARTESIAN_POINT('Ctrl Pts',(-1.22207656456199,1.,4.01386104434674));
#49640=CARTESIAN_POINT('Ctrl Pts',(-1.21884478244983,1.,4.01042947142681));
#49641=CARTESIAN_POINT('Ctrl Pts',(-1.21455398918813,1.,4.00584409524937));
#49642=CARTESIAN_POINT('Ctrl Pts',(-1.20922097030107,1.,4.00009577952534));
#49643=CARTESIAN_POINT('Ctrl Pts',(-1.2039185237544,1.,3.99433084800649));
#49644=CARTESIAN_POINT('Ctrl Pts',(-1.19864679609596,1.,3.98854928957287));
#49645=CARTESIAN_POINT('Ctrl Pts',(-1.19340598349307,1.,3.98275111052015));
#49646=CARTESIAN_POINT('Ctrl Pts',(-1.18819633715285,1.,3.97693634766926));
#49647=CARTESIAN_POINT('Ctrl Pts',(-1.18301815039596,1.,3.9711050516465));
#49648=CARTESIAN_POINT('Ctrl Pts',(-1.17787174135445,1.,3.96525726357682));
#49649=CARTESIAN_POINT('Ctrl Pts',(-1.17275743590327,1.,3.95939299213164));
#49650=CARTESIAN_POINT('Ctrl Pts',(-1.16767555244495,1.,3.95351219510062));
#49651=CARTESIAN_POINT('Ctrl Pts',(-1.16262637999261,1.,3.9476147478092));
#49652=CARTESIAN_POINT('Ctrl Pts',(-1.1576101834106,1.,3.94170046685542));
#49653=CARTESIAN_POINT('Ctrl Pts',(-1.15262722716391,1.,3.9357691705651));
#49654=CARTESIAN_POINT('Ctrl Pts',(-1.14767779451147,1.,3.92982073294334));
#49655=CARTESIAN_POINT('Ctrl Pts',(-1.14276220561575,1.,3.92385513133937));
#49656=CARTESIAN_POINT('Ctrl Pts',(-1.13788084225511,1.,3.91787251936688));
#49657=CARTESIAN_POINT('Ctrl Pts',(-1.13303414693849,1.,3.91187321145495));
#49658=CARTESIAN_POINT('Ctrl Pts',(-1.12822258281518,1.,3.90585753318622));
#49659=CARTESIAN_POINT('Ctrl Pts',(-1.12344660099029,1.,3.89982569749978));
#49660=CARTESIAN_POINT('Ctrl Pts',(-1.11870660794609,1.,3.89377768340362));
#49661=CARTESIAN_POINT('Ctrl Pts',(-1.11400292434447,1.,3.88771308285229));
#49662=CARTESIAN_POINT('Ctrl Pts',(-1.10933577224029,1.,3.88163105531791));
#49663=CARTESIAN_POINT('Ctrl Pts',(-1.10470536603303,1.,3.87553067187566));
#49664=CARTESIAN_POINT('Ctrl Pts',(-1.10011198761202,1.,3.86941120134872));
#49665=CARTESIAN_POINT('Ctrl Pts',(-1.09555606505012,1.,3.86327241021242));
#49666=CARTESIAN_POINT('Ctrl Pts',(-1.09103825516288,1.,3.85711487933911));
#49667=CARTESIAN_POINT('Ctrl Pts',(-1.08655950846377,1.,3.8509402522269));
#49668=CARTESIAN_POINT('Ctrl Pts',(-1.08212087917986,1.,3.84475048030615));
#49669=CARTESIAN_POINT('Ctrl Pts',(-1.07772335353856,1.,3.83854714117486));
#49670=CARTESIAN_POINT('Ctrl Pts',(-1.0733676663346,1.,3.83233071195145));
#49671=CARTESIAN_POINT('Ctrl Pts',(-1.0690541318036,1.,3.82609989967278));
#49672=CARTESIAN_POINT('Ctrl Pts',(-1.06478244038931,1.,3.81985083953012));
#49673=CARTESIAN_POINT('Ctrl Pts',(-1.06055206187298,1.,3.81357866117485));
#49674=CARTESIAN_POINT('Ctrl Pts',(-1.05636266918643,1.,3.80727913637784));
#49675=CARTESIAN_POINT('Ctrl Pts',(-1.05221457990015,1.,3.80095039790678));
#49676=CARTESIAN_POINT('Ctrl Pts',(-1.04810913267641,1.,3.79459440308793));
#49677=CARTESIAN_POINT('Ctrl Pts',(-1.04404924374426,1.,3.78821910787195));
#49678=CARTESIAN_POINT('Ctrl Pts',(-1.04003862055804,1.,3.78183535008192));
#49679=CARTESIAN_POINT('Ctrl Pts',(-1.03608074678013,1.,3.77545283140445));
#49680=CARTESIAN_POINT('Ctrl Pts',(-1.0321778660492,1.,3.76907609832522));
#49681=CARTESIAN_POINT('Ctrl Pts',(-1.02833014458181,1.,3.76270122291232));
#49682=CARTESIAN_POINT('Ctrl Pts',(-1.0245342944466,1.,3.75631037456194));
#49683=CARTESIAN_POINT('Ctrl Pts',(-1.02078510487428,1.,3.74987777155834));
#49684=CARTESIAN_POINT('Ctrl Pts',(-1.01707794311079,1.,3.74337942504959));
#49685=CARTESIAN_POINT('Ctrl Pts',(-1.01341114319903,1.,3.73680245055734));
#49686=CARTESIAN_POINT('Ctrl Pts',(-1.00978798539496,1.,3.73015276704426));
#49687=CARTESIAN_POINT('Ctrl Pts',(-1.0062200073571,1.,3.72346803750595));
#49688=CARTESIAN_POINT('Ctrl Pts',(-1.00272423396822,1.,3.71680667125118));
#49689=CARTESIAN_POINT('Ctrl Pts',(-0.999317260756531,1.,3.71022439713938));
#49690=CARTESIAN_POINT('Ctrl Pts',(-0.996009819772518,1.,3.70375282282138));
#49691=CARTESIAN_POINT('Ctrl Pts',(-0.99280221833201,1.,3.69738123415662));
#49692=CARTESIAN_POINT('Ctrl Pts',(-0.989676715398558,1.,3.69102682138846));
#49693=CARTESIAN_POINT('Ctrl Pts',(-0.986602639863838,1.,3.68455317926068));
#49694=CARTESIAN_POINT('Ctrl Pts',(-0.983550791470419,1.,3.67782408841715));
#49695=CARTESIAN_POINT('Ctrl Pts',(-0.980505922458267,1.,3.67074983340361));
#49696=CARTESIAN_POINT('Ctrl Pts',(-0.977478312751618,1.,3.66333049637475));
#49697=CARTESIAN_POINT('Ctrl Pts',(-0.974519971354848,1.,3.65571576735126));
#49698=CARTESIAN_POINT('Ctrl Pts',(-0.971722122061341,1.,3.64819756447455));
#49699=CARTESIAN_POINT('Ctrl Pts',(-0.969195124675866,1.,3.64113946505766));
#49700=CARTESIAN_POINT('Ctrl Pts',(-0.967052554541386,1.,3.63492122081143));
#49701=CARTESIAN_POINT('Ctrl Pts',(-0.965395153165293,1.,3.62988252139846));
#49702=CARTESIAN_POINT('Ctrl Pts',(-0.964373850166457,1.,3.62652618145335));
#49703=CARTESIAN_POINT('Ctrl Pts',(-0.963957782642843,1.,3.62489305727662));
#49704=CARTESIAN_POINT('Ctrl Pts',(-0.963861297423241,1.,3.62424461507588));
#49705=CARTESIAN_POINT('Ctrl Pts',(-0.963880158555582,1.,3.6240482887845));
#49706=CARTESIAN_POINT('Ctrl Pts',(-0.963899035117249,1.,3.62400312501245));
#49707=CARTESIAN_POINT('',(-1.22531898815164,0.,4.01728681790024));
#49708=CARTESIAN_POINT('Ctrl Pts',(-1.35022972712301,-1.,3.49848248301936));
#49709=CARTESIAN_POINT('Ctrl Pts',(-1.35022972712301,1.,3.49848248301936));
#49710=CARTESIAN_POINT('Ctrl Pts',(-1.35026426118402,-1.,3.4984026005375));
#49711=CARTESIAN_POINT('Ctrl Pts',(-1.35026426118402,1.,3.4984026005375));
#49712=CARTESIAN_POINT('Ctrl Pts',(-1.35037650303019,-1.,3.49840357193736));
#49713=CARTESIAN_POINT('Ctrl Pts',(-1.35037650303019,1.,3.49840357193736));
#49714=CARTESIAN_POINT('Ctrl Pts',(-1.35067437417483,-1.,3.49888720257132));
#49715=CARTESIAN_POINT('Ctrl Pts',(-1.35067437417483,1.,3.49888720257132));
#49716=CARTESIAN_POINT('Ctrl Pts',(-1.3513307633124,-1.,3.5004970706414));
#49717=CARTESIAN_POINT('Ctrl Pts',(-1.3513307633124,1.,3.5004970706414));
#49718=CARTESIAN_POINT('Ctrl Pts',(-1.35257032843486,-1.,3.50408168106261));
#49719=CARTESIAN_POINT('Ctrl Pts',(-1.35257032843486,1.,3.50408168106261));
#49720=CARTESIAN_POINT('Ctrl Pts',(-1.35419113575956,-1.,3.50913227059999));
#49721=CARTESIAN_POINT('Ctrl Pts',(-1.35419113575956,1.,3.50913227059999));
#49722=CARTESIAN_POINT('Ctrl Pts',(-1.35611275237152,-1.,3.51542230699556));
#49723=CARTESIAN_POINT('Ctrl Pts',(-1.35611275237152,1.,3.51542230699556));
#49724=CARTESIAN_POINT('Ctrl Pts',(-1.35821701528836,-1.,3.52261776116748));
#49725=CARTESIAN_POINT('Ctrl Pts',(-1.35821701528836,1.,3.52261776116748));
#49726=CARTESIAN_POINT('Ctrl Pts',(-1.36037259643734,-1.,3.530344649616));
#49727=CARTESIAN_POINT('Ctrl Pts',(-1.36037259643734,1.,3.530344649616));
#49728=CARTESIAN_POINT('Ctrl Pts',(-1.36245507339307,-1.,3.53824396424961));
#49729=CARTESIAN_POINT('Ctrl Pts',(-1.36245507339307,1.,3.53824396424961));
#49730=CARTESIAN_POINT('Ctrl Pts',(-1.36436666257598,-1.,3.54602591832973));
#49731=CARTESIAN_POINT('Ctrl Pts',(-1.36436666257598,1.,3.54602591832973));
#49732=CARTESIAN_POINT('Ctrl Pts',(-1.3660614545677,-1.,3.55353883995949));
#49733=CARTESIAN_POINT('Ctrl Pts',(-1.3660614545677,1.,3.55353883995949));
#49734=CARTESIAN_POINT('Ctrl Pts',(-1.36754771771233,-1.,3.56077662028649));
#49735=CARTESIAN_POINT('Ctrl Pts',(-1.36754771771233,1.,3.56077662028649));
#49736=CARTESIAN_POINT('Ctrl Pts',(-1.36886584973389,-1.,3.5678208030466));
#49737=CARTESIAN_POINT('Ctrl Pts',(-1.36886584973389,1.,3.5678208030466));
#49738=CARTESIAN_POINT('Ctrl Pts',(-1.37007229485659,-1.,3.57479875549486));
#49739=CARTESIAN_POINT('Ctrl Pts',(-1.37007229485659,1.,3.57479875549486));
#49740=CARTESIAN_POINT('Ctrl Pts',(-1.37122241663062,-1.,3.58183885982715));
#49741=CARTESIAN_POINT('Ctrl Pts',(-1.37122241663062,1.,3.58183885982715));
#49742=CARTESIAN_POINT('Ctrl Pts',(-1.37235053660976,-1.,3.58901853846365));
#49743=CARTESIAN_POINT('Ctrl Pts',(-1.37235053660976,1.,3.58901853846365));
#49744=CARTESIAN_POINT('Ctrl Pts',(-1.37346320103157,-1.,3.59634627869048));
#49745=CARTESIAN_POINT('Ctrl Pts',(-1.37346320103157,1.,3.59634627869048));
#49746=CARTESIAN_POINT('Ctrl Pts',(-1.37455051379623,-1.,3.60379020123988));
#49747=CARTESIAN_POINT('Ctrl Pts',(-1.37455051379623,1.,3.60379020123988));
#49748=CARTESIAN_POINT('Ctrl Pts',(-1.37559314436634,-1.,3.61129546591064));
#49749=CARTESIAN_POINT('Ctrl Pts',(-1.37559314436634,1.,3.61129546591064));
#49750=CARTESIAN_POINT('Ctrl Pts',(-1.37657053403107,-1.,3.6188048116042));
#49751=CARTESIAN_POINT('Ctrl Pts',(-1.37657053403107,1.,3.6188048116042));
#49752=CARTESIAN_POINT('Ctrl Pts',(-1.37746987919881,-1.,3.62628098665145));
#49753=CARTESIAN_POINT('Ctrl Pts',(-1.37746987919881,1.,3.62628098665145));
#49754=CARTESIAN_POINT('Ctrl Pts',(-1.37829035457339,-1.,3.63371727442486));
#49755=CARTESIAN_POINT('Ctrl Pts',(-1.37829035457339,1.,3.63371727442486));
#49756=CARTESIAN_POINT('Ctrl Pts',(-1.37903818567359,-1.,3.64112507791141));
#49757=CARTESIAN_POINT('Ctrl Pts',(-1.37903818567359,1.,3.64112507791141));
#49758=CARTESIAN_POINT('Ctrl Pts',(-1.37972372481603,-1.,3.64852652756456));
#49759=CARTESIAN_POINT('Ctrl Pts',(-1.37972372481603,1.,3.64852652756456));
#49760=CARTESIAN_POINT('Ctrl Pts',(-1.38035791051213,-1.,3.6559455440439));
#49761=CARTESIAN_POINT('Ctrl Pts',(-1.38035791051213,1.,3.6559455440439));
#49762=CARTESIAN_POINT('Ctrl Pts',(-1.38094856333552,-1.,3.66339848520857));
#49763=CARTESIAN_POINT('Ctrl Pts',(-1.38094856333552,1.,3.66339848520857));
#49764=CARTESIAN_POINT('Ctrl Pts',(-1.38149812653868,-1.,3.67088843112262));
#49765=CARTESIAN_POINT('Ctrl Pts',(-1.38149812653868,1.,3.67088843112262));
#49766=CARTESIAN_POINT('Ctrl Pts',(-1.3820057429062,-1.,3.67841038482414));
#49767=CARTESIAN_POINT('Ctrl Pts',(-1.3820057429062,1.,3.67841038482414));
#49768=CARTESIAN_POINT('Ctrl Pts',(-1.38246852827182,-1.,3.68595444983837));
#49769=CARTESIAN_POINT('Ctrl Pts',(-1.38246852827182,1.,3.68595444983837));
#49770=CARTESIAN_POINT('Ctrl Pts',(-1.38288311171651,-1.,3.69350967899526));
#49771=CARTESIAN_POINT('Ctrl Pts',(-1.38288311171651,1.,3.69350967899526));
#49772=CARTESIAN_POINT('Ctrl Pts',(-1.38324717612865,-1.,3.701067921679));
#49773=CARTESIAN_POINT('Ctrl Pts',(-1.38324717612865,1.,3.701067921679));
#49774=CARTESIAN_POINT('Ctrl Pts',(-1.38356065402124,-1.,3.70862680753347));
#49775=CARTESIAN_POINT('Ctrl Pts',(-1.38356065402124,1.,3.70862680753347));
#49776=CARTESIAN_POINT('Ctrl Pts',(-1.38382489984586,-1.,3.7161876605181));
#49777=CARTESIAN_POINT('Ctrl Pts',(-1.38382489984586,1.,3.7161876605181));
#49778=CARTESIAN_POINT('Ctrl Pts',(-1.3840421342895,-1.,3.72375409358803));
#49779=CARTESIAN_POINT('Ctrl Pts',(-1.3840421342895,1.,3.72375409358803));
#49780=CARTESIAN_POINT('Ctrl Pts',(-1.38421479111531,-1.,3.73133035859282));
#49781=CARTESIAN_POINT('Ctrl Pts',(-1.38421479111531,1.,3.73133035859282));
#49782=CARTESIAN_POINT('Ctrl Pts',(-1.38434489156458,-1.,3.73891976418104));
#49783=CARTESIAN_POINT('Ctrl Pts',(-1.38434489156458,1.,3.73891976418104));
#49784=CARTESIAN_POINT('Ctrl Pts',(-1.38443344984394,-1.,3.74652317167876));
#49785=CARTESIAN_POINT('Ctrl Pts',(-1.38443344984394,1.,3.74652317167876));
#49786=CARTESIAN_POINT('Ctrl Pts',(-1.38448077997163,-1.,3.7541397631875));
#49787=CARTESIAN_POINT('Ctrl Pts',(-1.38448077997163,1.,3.7541397631875));
#49788=CARTESIAN_POINT('Ctrl Pts',(-1.3844867525335,-1.,3.76176768271367));
#49789=CARTESIAN_POINT('Ctrl Pts',(-1.3844867525335,1.,3.76176768271367));
#49790=CARTESIAN_POINT('Ctrl Pts',(-1.38445107339518,-1.,3.76940473185779));
#49791=CARTESIAN_POINT('Ctrl Pts',(-1.38445107339518,1.,3.76940473185779));
#49792=CARTESIAN_POINT('Ctrl Pts',(-1.38437354551428,-1.,3.77704902230418));
#49793=CARTESIAN_POINT('Ctrl Pts',(-1.38437354551428,1.,3.77704902230418));
#49794=CARTESIAN_POINT('Ctrl Pts',(-1.38425435883756,-1.,3.78469969805082));
#49795=CARTESIAN_POINT('Ctrl Pts',(-1.38425435883756,1.,3.78469969805082));
#49796=CARTESIAN_POINT('Ctrl Pts',(-1.38409399694566,-1.,3.79235669640841));
#49797=CARTESIAN_POINT('Ctrl Pts',(-1.38409399694566,1.,3.79235669640841));
#49798=CARTESIAN_POINT('Ctrl Pts',(-1.38389311766682,-1.,3.80002044322111));
#49799=CARTESIAN_POINT('Ctrl Pts',(-1.38389311766682,1.,3.80002044322111));
#49800=CARTESIAN_POINT('Ctrl Pts',(-1.3836524404622,-1.,3.80769156398411));
#49801=CARTESIAN_POINT('Ctrl Pts',(-1.3836524404622,1.,3.80769156398411));
#49802=CARTESIAN_POINT('Ctrl Pts',(-1.38337263902782,-1.,3.81537060817811));
#49803=CARTESIAN_POINT('Ctrl Pts',(-1.38337263902782,1.,3.81537060817811));
#49804=CARTESIAN_POINT('Ctrl Pts',(-1.38305421262763,-1.,3.82305771743829));
#49805=CARTESIAN_POINT('Ctrl Pts',(-1.38305421262763,1.,3.82305771743829));
#49806=CARTESIAN_POINT('Ctrl Pts',(-1.38269750245138,-1.,3.8307526698229));
#49807=CARTESIAN_POINT('Ctrl Pts',(-1.38269750245138,1.,3.8307526698229));
#49808=CARTESIAN_POINT('Ctrl Pts',(-1.38230274828822,-1.,3.83845502790746));
#49809=CARTESIAN_POINT('Ctrl Pts',(-1.38230274828822,1.,3.83845502790746));
#49810=CARTESIAN_POINT('Ctrl Pts',(-1.38187013346109,-1.,3.84616425605764));
#49811=CARTESIAN_POINT('Ctrl Pts',(-1.38187013346109,1.,3.84616425605764));
#49812=CARTESIAN_POINT('Ctrl Pts',(-1.38139983115049,-1.,3.85387983979481));
#49813=CARTESIAN_POINT('Ctrl Pts',(-1.38139983115049,1.,3.85387983979481));
#49814=CARTESIAN_POINT('Ctrl Pts',(-1.38089205992989,-1.,3.86160143043959));
#49815=CARTESIAN_POINT('Ctrl Pts',(-1.38089205992989,1.,3.86160143043959));
#49816=CARTESIAN_POINT('Ctrl Pts',(-1.38034709213014,-1.,3.86932885813068));
#49817=CARTESIAN_POINT('Ctrl Pts',(-1.38034709213014,1.,3.86932885813068));
#49818=CARTESIAN_POINT('Ctrl Pts',(-1.37976523097073,-1.,3.87706205830532));
#49819=CARTESIAN_POINT('Ctrl Pts',(-1.37976523097073,1.,3.87706205830532));
#49820=CARTESIAN_POINT('Ctrl Pts',(-1.37914679719383,-1.,3.88480102249277));
#49821=CARTESIAN_POINT('Ctrl Pts',(-1.37914679719383,1.,3.88480102249277));
#49822=CARTESIAN_POINT('Ctrl Pts',(-1.3784921128802,-1.,3.89254574338496));
#49823=CARTESIAN_POINT('Ctrl Pts',(-1.3784921128802,1.,3.89254574338496));
#49824=CARTESIAN_POINT('Ctrl Pts',(-1.37780148512792,-1.,3.90029615196727));
#49825=CARTESIAN_POINT('Ctrl Pts',(-1.37780148512792,1.,3.90029615196727));
#49826=CARTESIAN_POINT('Ctrl Pts',(-1.3770751963402,-1.,3.90805209523486));
#49827=CARTESIAN_POINT('Ctrl Pts',(-1.3770751963402,1.,3.90805209523486));
#49828=CARTESIAN_POINT('Ctrl Pts',(-1.37631350505797,-1.,3.91581337462644));
#49829=CARTESIAN_POINT('Ctrl Pts',(-1.37631350505797,1.,3.91581337462644));
#49830=CARTESIAN_POINT('Ctrl Pts',(-1.37551664448242,-1.,3.92357976987672));
#49831=CARTESIAN_POINT('Ctrl Pts',(-1.37551664448242,1.,3.92357976987672));
#49832=CARTESIAN_POINT('Ctrl Pts',(-1.37468482215751,-1.,3.93135106761844));
#49833=CARTESIAN_POINT('Ctrl Pts',(-1.37468482215751,1.,3.93135106761844));
#49834=CARTESIAN_POINT('Ctrl Pts',(-1.37381821967165,-1.,3.93912709040818));
#49835=CARTESIAN_POINT('Ctrl Pts',(-1.37381821967165,1.,3.93912709040818));
#49836=CARTESIAN_POINT('Ctrl Pts',(-1.37291699202807,-1.,3.94690771785133));
#49837=CARTESIAN_POINT('Ctrl Pts',(-1.37291699202807,1.,3.94690771785133));
#49838=CARTESIAN_POINT('Ctrl Pts',(-1.37198126432386,-1.,3.95469287280914));
#49839=CARTESIAN_POINT('Ctrl Pts',(-1.37198126432386,1.,3.95469287280914));
#49840=CARTESIAN_POINT('Ctrl Pts',(-1.3712051561502,-1.,3.96092458506535));
#49841=CARTESIAN_POINT('Ctrl Pts',(-1.3712051561502,1.,3.96092458506535));
#49842=CARTESIAN_POINT('Ctrl Pts',(-1.37060761745635,-1.,3.96560037974645));
#49843=CARTESIAN_POINT('Ctrl Pts',(-1.37060761745635,1.,3.96560037974645));
#49844=CARTESIAN_POINT('Ctrl Pts',(-1.37020239094614,-1.,3.9687184694131));
#49845=CARTESIAN_POINT('Ctrl Pts',(-1.37020239094614,1.,3.9687184694131));
#49846=CARTESIAN_POINT('Ctrl Pts',(-1.36999806084572,-1.,3.97027773754922));
#49847=CARTESIAN_POINT('Ctrl Pts',(-1.36999806084572,1.,3.97027773754922));
#49848=CARTESIAN_POINT('',(-1.35032489087101,1.,3.4984457533445));
#49849=CARTESIAN_POINT('Ctrl Pts',(-1.35032489087101,-1.,3.4984457533445));
#49850=CARTESIAN_POINT('Ctrl Pts',(-1.35032489087101,-0.666666666666667,
3.4984457533445));
#49851=CARTESIAN_POINT('Ctrl Pts',(-1.35032489087101,-0.333333333333333,
3.4984457533445));
#49852=CARTESIAN_POINT('Ctrl Pts',(-1.35032489087101,0.333333333333333,
3.4984457533445));
#49853=CARTESIAN_POINT('Ctrl Pts',(-1.35032489087101,0.666666666666667,
3.4984457533445));
#49854=CARTESIAN_POINT('Ctrl Pts',(-1.35032489087101,1.,3.4984457533445));
#49855=CARTESIAN_POINT('',(-1.36999806084572,1.,3.97027773754922));
#49856=CARTESIAN_POINT('',(-1.36999806084572,0.,3.97027773754922));
#49857=CARTESIAN_POINT('Ctrl Pts',(-1.35032489087101,1.,3.4984457533445));
#49858=CARTESIAN_POINT('Ctrl Pts',(-1.35036670892966,1.,3.49847119623846));
#49859=CARTESIAN_POINT('Ctrl Pts',(-1.35049736560527,1.,3.49861894124827));
#49860=CARTESIAN_POINT('Ctrl Pts',(-1.35080045218587,1.,3.49920025459723));
#49861=CARTESIAN_POINT('Ctrl Pts',(-1.35142377279517,1.,3.5007660381649));
#49862=CARTESIAN_POINT('Ctrl Pts',(-1.35257032843486,1.,3.50408168106261));
#49863=CARTESIAN_POINT('Ctrl Pts',(-1.35419113575956,1.,3.50913227059999));
#49864=CARTESIAN_POINT('Ctrl Pts',(-1.35611275237152,1.,3.51542230699556));
#49865=CARTESIAN_POINT('Ctrl Pts',(-1.35821701528836,1.,3.52261776116748));
#49866=CARTESIAN_POINT('Ctrl Pts',(-1.36037259643734,1.,3.530344649616));
#49867=CARTESIAN_POINT('Ctrl Pts',(-1.36245507339307,1.,3.53824396424961));
#49868=CARTESIAN_POINT('Ctrl Pts',(-1.36436666257598,1.,3.54602591832973));
#49869=CARTESIAN_POINT('Ctrl Pts',(-1.3660614545677,1.,3.55353883995949));
#49870=CARTESIAN_POINT('Ctrl Pts',(-1.36754771771233,1.,3.56077662028649));
#49871=CARTESIAN_POINT('Ctrl Pts',(-1.36886584973389,1.,3.5678208030466));
#49872=CARTESIAN_POINT('Ctrl Pts',(-1.37007229485659,1.,3.57479875549486));
#49873=CARTESIAN_POINT('Ctrl Pts',(-1.37122241663062,1.,3.58183885982715));
#49874=CARTESIAN_POINT('Ctrl Pts',(-1.37235053660976,1.,3.58901853846365));
#49875=CARTESIAN_POINT('Ctrl Pts',(-1.37346320103157,1.,3.59634627869048));
#49876=CARTESIAN_POINT('Ctrl Pts',(-1.37455051379623,1.,3.60379020123988));
#49877=CARTESIAN_POINT('Ctrl Pts',(-1.37559314436634,1.,3.61129546591064));
#49878=CARTESIAN_POINT('Ctrl Pts',(-1.37657053403107,1.,3.6188048116042));
#49879=CARTESIAN_POINT('Ctrl Pts',(-1.37746987919881,1.,3.62628098665145));
#49880=CARTESIAN_POINT('Ctrl Pts',(-1.37829035457339,1.,3.63371727442486));
#49881=CARTESIAN_POINT('Ctrl Pts',(-1.37903818567359,1.,3.64112507791141));
#49882=CARTESIAN_POINT('Ctrl Pts',(-1.37972372481603,1.,3.64852652756456));
#49883=CARTESIAN_POINT('Ctrl Pts',(-1.38035791051213,1.,3.6559455440439));
#49884=CARTESIAN_POINT('Ctrl Pts',(-1.38094856333552,1.,3.66339848520857));
#49885=CARTESIAN_POINT('Ctrl Pts',(-1.38149812653868,1.,3.67088843112262));
#49886=CARTESIAN_POINT('Ctrl Pts',(-1.3820057429062,1.,3.67841038482414));
#49887=CARTESIAN_POINT('Ctrl Pts',(-1.38246852827182,1.,3.68595444983837));
#49888=CARTESIAN_POINT('Ctrl Pts',(-1.38288311171651,1.,3.69350967899526));
#49889=CARTESIAN_POINT('Ctrl Pts',(-1.38324717612865,1.,3.701067921679));
#49890=CARTESIAN_POINT('Ctrl Pts',(-1.38356065402124,1.,3.70862680753347));
#49891=CARTESIAN_POINT('Ctrl Pts',(-1.38382489984586,1.,3.7161876605181));
#49892=CARTESIAN_POINT('Ctrl Pts',(-1.3840421342895,1.,3.72375409358803));
#49893=CARTESIAN_POINT('Ctrl Pts',(-1.38421479111531,1.,3.73133035859282));
#49894=CARTESIAN_POINT('Ctrl Pts',(-1.38434489156458,1.,3.73891976418104));
#49895=CARTESIAN_POINT('Ctrl Pts',(-1.38443344984394,1.,3.74652317167876));
#49896=CARTESIAN_POINT('Ctrl Pts',(-1.38448077997163,1.,3.7541397631875));
#49897=CARTESIAN_POINT('Ctrl Pts',(-1.3844867525335,1.,3.76176768271367));
#49898=CARTESIAN_POINT('Ctrl Pts',(-1.38445107339518,1.,3.76940473185779));
#49899=CARTESIAN_POINT('Ctrl Pts',(-1.38437354551428,1.,3.77704902230418));
#49900=CARTESIAN_POINT('Ctrl Pts',(-1.38425435883756,1.,3.78469969805082));
#49901=CARTESIAN_POINT('Ctrl Pts',(-1.38409399694566,1.,3.79235669640841));
#49902=CARTESIAN_POINT('Ctrl Pts',(-1.38389311766682,1.,3.80002044322111));
#49903=CARTESIAN_POINT('Ctrl Pts',(-1.3836524404622,1.,3.80769156398411));
#49904=CARTESIAN_POINT('Ctrl Pts',(-1.38337263902782,1.,3.81537060817811));
#49905=CARTESIAN_POINT('Ctrl Pts',(-1.38305421262763,1.,3.82305771743829));
#49906=CARTESIAN_POINT('Ctrl Pts',(-1.38269750245138,1.,3.8307526698229));
#49907=CARTESIAN_POINT('Ctrl Pts',(-1.38230274828822,1.,3.83845502790746));
#49908=CARTESIAN_POINT('Ctrl Pts',(-1.38187013346109,1.,3.84616425605764));
#49909=CARTESIAN_POINT('Ctrl Pts',(-1.38139983115049,1.,3.85387983979481));
#49910=CARTESIAN_POINT('Ctrl Pts',(-1.38089205992989,1.,3.86160143043959));
#49911=CARTESIAN_POINT('Ctrl Pts',(-1.38034709213014,1.,3.86932885813068));
#49912=CARTESIAN_POINT('Ctrl Pts',(-1.37976523097073,1.,3.87706205830532));
#49913=CARTESIAN_POINT('Ctrl Pts',(-1.37914679719383,1.,3.88480102249277));
#49914=CARTESIAN_POINT('Ctrl Pts',(-1.3784921128802,1.,3.89254574338496));
#49915=CARTESIAN_POINT('Ctrl Pts',(-1.37780148512792,1.,3.90029615196727));
#49916=CARTESIAN_POINT('Ctrl Pts',(-1.3770751963402,1.,3.90805209523486));
#49917=CARTESIAN_POINT('Ctrl Pts',(-1.37631350505797,1.,3.91581337462644));
#49918=CARTESIAN_POINT('Ctrl Pts',(-1.37551664448242,1.,3.92357976987672));
#49919=CARTESIAN_POINT('Ctrl Pts',(-1.37468482215751,1.,3.93135106761844));
#49920=CARTESIAN_POINT('Ctrl Pts',(-1.37381821967165,1.,3.93912709040818));
#49921=CARTESIAN_POINT('Ctrl Pts',(-1.37291699202807,1.,3.94690771785133));
#49922=CARTESIAN_POINT('Ctrl Pts',(-1.37198126432386,1.,3.95469287280914));
#49923=CARTESIAN_POINT('Ctrl Pts',(-1.3712051561502,1.,3.96092458506535));
#49924=CARTESIAN_POINT('Ctrl Pts',(-1.37060761745635,1.,3.96560037974645));
#49925=CARTESIAN_POINT('Ctrl Pts',(-1.37020239094614,1.,3.9687184694131));
#49926=CARTESIAN_POINT('Ctrl Pts',(-1.36999806084572,1.,3.97027773754922));
#49927=CARTESIAN_POINT('Origin',(-1.36999806084572,0.,3.97027773754922));
#49928=CARTESIAN_POINT('',(-1.22531898815164,1.,4.01728681790024));
#49929=CARTESIAN_POINT('Origin',(0.,0.,0.));
#49930=CARTESIAN_POINT('',(-1.51895082866166,1.,3.42859860294378));
#49931=CARTESIAN_POINT('Origin',(0.,1.,0.));
#49932=CARTESIAN_POINT('Ctrl Pts',(-1.51895082866166,1.,3.42859860294378));
#49933=CARTESIAN_POINT('Ctrl Pts',(-1.51895082866166,0.666666666666667,
3.42859860294378));
#49934=CARTESIAN_POINT('Ctrl Pts',(-1.51895082866166,0.333333333333333,
3.42859860294378));
#49935=CARTESIAN_POINT('Ctrl Pts',(-1.51895082866166,-0.333333333333333,
3.42859860294378));
#49936=CARTESIAN_POINT('Ctrl Pts',(-1.51895082866166,-0.666666666666667,
3.42859860294378));
#49937=CARTESIAN_POINT('Ctrl Pts',(-1.51895082866166,-1.,3.42859860294378));
#49938=CARTESIAN_POINT('Ctrl Pts',(-1.83867539237861,-1.,3.77614523045147));
#49939=CARTESIAN_POINT('Ctrl Pts',(-1.83867539237861,1.,3.77614523045147));
#49940=CARTESIAN_POINT('Ctrl Pts',(-1.83742834010821,-1.,3.77518714458232));
#49941=CARTESIAN_POINT('Ctrl Pts',(-1.83742834010821,1.,3.77518714458232));
#49942=CARTESIAN_POINT('Ctrl Pts',(-1.83493697935064,-1.,3.77326886065484));
#49943=CARTESIAN_POINT('Ctrl Pts',(-1.83493697935064,1.,3.77326886065484));
#49944=CARTESIAN_POINT('Ctrl Pts',(-1.83120816956515,-1.,3.77038509819777));
#49945=CARTESIAN_POINT('Ctrl Pts',(-1.83120816956515,1.,3.77038509819777));
#49946=CARTESIAN_POINT('Ctrl Pts',(-1.82625289221933,-1.,3.76652740355856));
#49947=CARTESIAN_POINT('Ctrl Pts',(-1.82625289221933,1.,3.76652740355856));
#49948=CARTESIAN_POINT('Ctrl Pts',(-1.82008629694924,-1.,3.76168412709652));
#49949=CARTESIAN_POINT('Ctrl Pts',(-1.82008629694924,1.,3.76168412709652));
#49950=CARTESIAN_POINT('Ctrl Pts',(-1.81394729834032,-1.,3.75681965683995));
#49951=CARTESIAN_POINT('Ctrl Pts',(-1.81394729834032,1.,3.75681965683995));
#49952=CARTESIAN_POINT('Ctrl Pts',(-1.80783603939662,-1.,3.75193395888069));
#49953=CARTESIAN_POINT('Ctrl Pts',(-1.80783603939662,1.,3.75193395888069));
#49954=CARTESIAN_POINT('Ctrl Pts',(-1.80175271485519,-1.,3.74702700874954));
#49955=CARTESIAN_POINT('Ctrl Pts',(-1.80175271485519,1.,3.74702700874954));
#49956=CARTESIAN_POINT('Ctrl Pts',(-1.79569757859041,-1.,3.74209880351667));
#49957=CARTESIAN_POINT('Ctrl Pts',(-1.79569757859041,1.,3.74209880351667));
#49958=CARTESIAN_POINT('Ctrl Pts',(-1.78967092823139,-1.,3.73714934729962));
#49959=CARTESIAN_POINT('Ctrl Pts',(-1.78967092823139,1.,3.73714934729962));
#49960=CARTESIAN_POINT('Ctrl Pts',(-1.78367308442682,-1.,3.73217863095022));
#49961=CARTESIAN_POINT('Ctrl Pts',(-1.78367308442682,1.,3.73217863095022));
#49962=CARTESIAN_POINT('Ctrl Pts',(-1.77770437039606,-1.,3.72718661205504));
#49963=CARTESIAN_POINT('Ctrl Pts',(-1.77770437039606,1.,3.72718661205504));
#49964=CARTESIAN_POINT('Ctrl Pts',(-1.77176509401846,-1.,3.72217319911429));
#49965=CARTESIAN_POINT('Ctrl Pts',(-1.77176509401846,1.,3.72217319911429));
#49966=CARTESIAN_POINT('Ctrl Pts',(-1.76585552124549,-1.,3.71713822377675));
#49967=CARTESIAN_POINT('Ctrl Pts',(-1.76585552124549,1.,3.71713822377675));
#49968=CARTESIAN_POINT('Ctrl Pts',(-1.75997588499021,-1.,3.71208146346454));
#49969=CARTESIAN_POINT('Ctrl Pts',(-1.75997588499021,1.,3.71208146346454));
#49970=CARTESIAN_POINT('Ctrl Pts',(-1.75412641804148,-1.,3.70700269736876));
#49971=CARTESIAN_POINT('Ctrl Pts',(-1.75412641804148,1.,3.70700269736876));
#49972=CARTESIAN_POINT('Ctrl Pts',(-1.74830738046092,-1.,3.70190175673422));
#49973=CARTESIAN_POINT('Ctrl Pts',(-1.74830738046092,1.,3.70190175673422));
#49974=CARTESIAN_POINT('Ctrl Pts',(-1.74251908492589,-1.,3.6967785691046));
#49975=CARTESIAN_POINT('Ctrl Pts',(-1.74251908492589,1.,3.6967785691046));
#49976=CARTESIAN_POINT('Ctrl Pts',(-1.73676193254493,-1.,3.69163322647906));
#49977=CARTESIAN_POINT('Ctrl Pts',(-1.73676193254493,1.,3.69163322647906));
#49978=CARTESIAN_POINT('Ctrl Pts',(-1.73103640956647,-1.,3.68646597019188));
#49979=CARTESIAN_POINT('Ctrl Pts',(-1.73103640956647,1.,3.68646597019188));
#49980=CARTESIAN_POINT('Ctrl Pts',(-1.72534302437003,-1.,3.68127704936472));
#49981=CARTESIAN_POINT('Ctrl Pts',(-1.72534302437003,1.,3.68127704936472));
#49982=CARTESIAN_POINT('Ctrl Pts',(-1.71968225581787,-1.,3.67606660374665));
#49983=CARTESIAN_POINT('Ctrl Pts',(-1.71968225581787,1.,3.67606660374665));
#49984=CARTESIAN_POINT('Ctrl Pts',(-1.71405450210392,-1.,3.67083454901629));
#49985=CARTESIAN_POINT('Ctrl Pts',(-1.71405450210392,1.,3.67083454901629));
#49986=CARTESIAN_POINT('Ctrl Pts',(-1.70846001610983,-1.,3.6655804319893));
#49987=CARTESIAN_POINT('Ctrl Pts',(-1.70846001610983,1.,3.6655804319893));
#49988=CARTESIAN_POINT('Ctrl Pts',(-1.70289888566904,-1.,3.6603033877491));
#49989=CARTESIAN_POINT('Ctrl Pts',(-1.70289888566904,1.,3.6603033877491));
#49990=CARTESIAN_POINT('Ctrl Pts',(-1.69737117722559,-1.,3.65500246526798));
#49991=CARTESIAN_POINT('Ctrl Pts',(-1.69737117722559,1.,3.65500246526798));
#49992=CARTESIAN_POINT('Ctrl Pts',(-1.691877054817,-1.,3.64967689827393));
#49993=CARTESIAN_POINT('Ctrl Pts',(-1.691877054817,1.,3.64967689827393));
#49994=CARTESIAN_POINT('Ctrl Pts',(-1.68641690471455,-1.,3.64432638915199));
#49995=CARTESIAN_POINT('Ctrl Pts',(-1.68641690471455,1.,3.64432638915199));
#49996=CARTESIAN_POINT('Ctrl Pts',(-1.68099146651577,-1.,3.63895140887443));
#49997=CARTESIAN_POINT('Ctrl Pts',(-1.68099146651577,1.,3.63895140887443));
#49998=CARTESIAN_POINT('Ctrl Pts',(-1.67560193613145,-1.,3.63355343201211));
#49999=CARTESIAN_POINT('Ctrl Pts',(-1.67560193613145,1.,3.63355343201211));
#50000=CARTESIAN_POINT('Ctrl Pts',(-1.67024966008037,-1.,3.62813422105257));
#50001=CARTESIAN_POINT('Ctrl Pts',(-1.67024966008037,1.,3.62813422105257));
#50002=CARTESIAN_POINT('Ctrl Pts',(-1.66493585923853,-1.,3.62269517989104));
#50003=CARTESIAN_POINT('Ctrl Pts',(-1.66493585923853,1.,3.62269517989104));
#50004=CARTESIAN_POINT('Ctrl Pts',(-1.65966133399186,-1.,3.61723666482457));
#50005=CARTESIAN_POINT('Ctrl Pts',(-1.65966133399186,1.,3.61723666482457));
#50006=CARTESIAN_POINT('Ctrl Pts',(-1.65442619244327,-1.,3.61175734965129));
#50007=CARTESIAN_POINT('Ctrl Pts',(-1.65442619244327,1.,3.61175734965129));
#50008=CARTESIAN_POINT('Ctrl Pts',(-1.64922952425833,-1.,3.60625346556992));
#50009=CARTESIAN_POINT('Ctrl Pts',(-1.64922952425833,1.,3.60625346556992));
#50010=CARTESIAN_POINT('Ctrl Pts',(-1.6440700438558,-1.,3.6007202851384));
#50011=CARTESIAN_POINT('Ctrl Pts',(-1.6440700438558,1.,3.6007202851384));
#50012=CARTESIAN_POINT('Ctrl Pts',(-1.63894676675349,-1.,3.59515368334887));
#50013=CARTESIAN_POINT('Ctrl Pts',(-1.63894676675349,1.,3.59515368334887));
#50014=CARTESIAN_POINT('Ctrl Pts',(-1.63385971451259,-1.,3.58955176627876));
#50015=CARTESIAN_POINT('Ctrl Pts',(-1.63385971451259,1.,3.58955176627876));
#50016=CARTESIAN_POINT('Ctrl Pts',(-1.62881051550748,-1.,3.5839162577435));
#50017=CARTESIAN_POINT('Ctrl Pts',(-1.62881051550748,1.,3.5839162577435));
#50018=CARTESIAN_POINT('Ctrl Pts',(-1.62380329464851,-1.,3.57825455954405));
#50019=CARTESIAN_POINT('Ctrl Pts',(-1.62380329464851,1.,3.57825455954405));
#50020=CARTESIAN_POINT('Ctrl Pts',(-1.61884340915412,-1.,3.57257679609826));
#50021=CARTESIAN_POINT('Ctrl Pts',(-1.61884340915412,1.,3.57257679609826));
#50022=CARTESIAN_POINT('Ctrl Pts',(-1.61393581747522,-1.,3.56689200468404));
#50023=CARTESIAN_POINT('Ctrl Pts',(-1.61393581747522,1.,3.56689200468404));
#50024=CARTESIAN_POINT('Ctrl Pts',(-1.60908344685459,-1.,3.56120432482986));
#50025=CARTESIAN_POINT('Ctrl Pts',(-1.60908344685459,1.,3.56120432482986));
#50026=CARTESIAN_POINT('Ctrl Pts',(-1.60428584699848,-1.,3.55550985096117));
#50027=CARTESIAN_POINT('Ctrl Pts',(-1.60428584699848,1.,3.55550985096117));
#50028=CARTESIAN_POINT('Ctrl Pts',(-1.59953698113444,-1.,3.54979148634426));
#50029=CARTESIAN_POINT('Ctrl Pts',(-1.59953698113444,1.,3.54979148634426));
#50030=CARTESIAN_POINT('Ctrl Pts',(-1.5948276694975,-1.,3.544024581823));
#50031=CARTESIAN_POINT('Ctrl Pts',(-1.5948276694975,1.,3.544024581823));
#50032=CARTESIAN_POINT('Ctrl Pts',(-1.59014958368725,-1.,3.53818616861045));
#50033=CARTESIAN_POINT('Ctrl Pts',(-1.59014958368725,1.,3.53818616861045));
#50034=CARTESIAN_POINT('Ctrl Pts',(-1.58549906268083,-1.,3.53226378147068));
#50035=CARTESIAN_POINT('Ctrl Pts',(-1.58549906268083,1.,3.53226378147068));
#50036=CARTESIAN_POINT('Ctrl Pts',(-1.58088027227856,-1.,3.52626275334899));
#50037=CARTESIAN_POINT('Ctrl Pts',(-1.58088027227856,1.,3.52626275334899));
#50038=CARTESIAN_POINT('Ctrl Pts',(-1.5763104998818,-1.,3.52021847865961));
#50039=CARTESIAN_POINT('Ctrl Pts',(-1.5763104998818,1.,3.52021847865961));
#50040=CARTESIAN_POINT('Ctrl Pts',(-1.57181569799774,-1.,3.51418598431733));
#50041=CARTESIAN_POINT('Ctrl Pts',(-1.57181569799774,1.,3.51418598431733));
#50042=CARTESIAN_POINT('Ctrl Pts',(-1.56742097575041,-1.,3.50821771695427));
#50043=CARTESIAN_POINT('Ctrl Pts',(-1.56742097575041,1.,3.50821771695427));
#50044=CARTESIAN_POINT('Ctrl Pts',(-1.56314187758689,-1.,3.50234321621607));
#50045=CARTESIAN_POINT('Ctrl Pts',(-1.56314187758689,1.,3.50234321621607));
#50046=CARTESIAN_POINT('Ctrl Pts',(-1.55897703097859,-1.,3.49655185179623));
#50047=CARTESIAN_POINT('Ctrl Pts',(-1.55897703097859,1.,3.49655185179623));
#50048=CARTESIAN_POINT('Ctrl Pts',(-1.5548959590107,-1.,3.49076460877317));
#50049=CARTESIAN_POINT('Ctrl Pts',(-1.5548959590107,1.,3.49076460877317));
#50050=CARTESIAN_POINT('Ctrl Pts',(-1.55084702970382,-1.,3.48485155928414));
#50051=CARTESIAN_POINT('Ctrl Pts',(-1.55084702970382,1.,3.48485155928414));
#50052=CARTESIAN_POINT('Ctrl Pts',(-1.54678009290207,-1.,3.47868272898599));
#50053=CARTESIAN_POINT('Ctrl Pts',(-1.54678009290207,1.,3.47868272898599));
#50054=CARTESIAN_POINT('Ctrl Pts',(-1.54266605398152,-1.,3.47217189224576));
#50055=CARTESIAN_POINT('Ctrl Pts',(-1.54266605398152,1.,3.47217189224576));
#50056=CARTESIAN_POINT('Ctrl Pts',(-1.53851507915533,-1.,3.46531752207222));
#50057=CARTESIAN_POINT('Ctrl Pts',(-1.53851507915533,1.,3.46531752207222));
#50058=CARTESIAN_POINT('Ctrl Pts',(-1.53440195378902,-1.,3.45825932955273));
#50059=CARTESIAN_POINT('Ctrl Pts',(-1.53440195378902,1.,3.45825932955273));
#50060=CARTESIAN_POINT('Ctrl Pts',(-1.530462444618,-1.,3.45127136828667));
#50061=CARTESIAN_POINT('Ctrl Pts',(-1.530462444618,1.,3.45127136828667));
#50062=CARTESIAN_POINT('Ctrl Pts',(-1.52686242875717,-1.,3.44469547527));
#50063=CARTESIAN_POINT('Ctrl Pts',(-1.52686242875717,1.,3.44469547527));
#50064=CARTESIAN_POINT('Ctrl Pts',(-1.52377348950429,-1.,3.43888895974182));
#50065=CARTESIAN_POINT('Ctrl Pts',(-1.52377348950429,1.,3.43888895974182));
#50066=CARTESIAN_POINT('Ctrl Pts',(-1.52134826724227,-1.,3.43417156977749));
#50067=CARTESIAN_POINT('Ctrl Pts',(-1.52134826724227,1.,3.43417156977749));
#50068=CARTESIAN_POINT('Ctrl Pts',(-1.51969006980792,-1.,3.43076036253384));
#50069=CARTESIAN_POINT('Ctrl Pts',(-1.51969006980792,1.,3.43076036253384));
#50070=CARTESIAN_POINT('Ctrl Pts',(-1.51901585838879,-1.,3.42915787669388));
#50071=CARTESIAN_POINT('Ctrl Pts',(-1.51901585838879,1.,3.42915787669388));
#50072=CARTESIAN_POINT('Ctrl Pts',(-1.51888450659497,-1.,3.42860527148835));
#50073=CARTESIAN_POINT('Ctrl Pts',(-1.51888450659497,1.,3.42860527148835));
#50074=CARTESIAN_POINT('Ctrl Pts',(-1.51896318668306,-1.,3.42852521763648));
#50075=CARTESIAN_POINT('Ctrl Pts',(-1.51896318668306,1.,3.42852521763648));
#50076=CARTESIAN_POINT('Ctrl Pts',(-1.519044091397,-1.,3.42855728381368));
#50077=CARTESIAN_POINT('Ctrl Pts',(-1.519044091397,1.,3.42855728381368));
#50078=CARTESIAN_POINT('',(-1.83867539237861,1.,3.77614523045147));
#50079=CARTESIAN_POINT('Ctrl Pts',(-1.83867539237861,1.,3.77614523045147));
#50080=CARTESIAN_POINT('Ctrl Pts',(-1.83742834010821,1.,3.77518714458232));
#50081=CARTESIAN_POINT('Ctrl Pts',(-1.83493697935064,1.,3.77326886065484));
#50082=CARTESIAN_POINT('Ctrl Pts',(-1.83120816956515,1.,3.77038509819777));
#50083=CARTESIAN_POINT('Ctrl Pts',(-1.82625289221933,1.,3.76652740355856));
#50084=CARTESIAN_POINT('Ctrl Pts',(-1.82008629694924,1.,3.76168412709652));
#50085=CARTESIAN_POINT('Ctrl Pts',(-1.81394729834032,1.,3.75681965683995));
#50086=CARTESIAN_POINT('Ctrl Pts',(-1.80783603939662,1.,3.75193395888069));
#50087=CARTESIAN_POINT('Ctrl Pts',(-1.80175271485519,1.,3.74702700874954));
#50088=CARTESIAN_POINT('Ctrl Pts',(-1.79569757859041,1.,3.74209880351667));
#50089=CARTESIAN_POINT('Ctrl Pts',(-1.78967092823139,1.,3.73714934729962));
#50090=CARTESIAN_POINT('Ctrl Pts',(-1.78367308442682,1.,3.73217863095022));
#50091=CARTESIAN_POINT('Ctrl Pts',(-1.77770437039606,1.,3.72718661205504));
#50092=CARTESIAN_POINT('Ctrl Pts',(-1.77176509401846,1.,3.72217319911429));
#50093=CARTESIAN_POINT('Ctrl Pts',(-1.76585552124549,1.,3.71713822377675));
#50094=CARTESIAN_POINT('Ctrl Pts',(-1.75997588499021,1.,3.71208146346454));
#50095=CARTESIAN_POINT('Ctrl Pts',(-1.75412641804148,1.,3.70700269736876));
#50096=CARTESIAN_POINT('Ctrl Pts',(-1.74830738046092,1.,3.70190175673422));
#50097=CARTESIAN_POINT('Ctrl Pts',(-1.74251908492589,1.,3.6967785691046));
#50098=CARTESIAN_POINT('Ctrl Pts',(-1.73676193254493,1.,3.69163322647906));
#50099=CARTESIAN_POINT('Ctrl Pts',(-1.73103640956647,1.,3.68646597019188));
#50100=CARTESIAN_POINT('Ctrl Pts',(-1.72534302437003,1.,3.68127704936472));
#50101=CARTESIAN_POINT('Ctrl Pts',(-1.71968225581787,1.,3.67606660374665));
#50102=CARTESIAN_POINT('Ctrl Pts',(-1.71405450210392,1.,3.67083454901629));
#50103=CARTESIAN_POINT('Ctrl Pts',(-1.70846001610983,1.,3.6655804319893));
#50104=CARTESIAN_POINT('Ctrl Pts',(-1.70289888566904,1.,3.6603033877491));
#50105=CARTESIAN_POINT('Ctrl Pts',(-1.69737117722559,1.,3.65500246526798));
#50106=CARTESIAN_POINT('Ctrl Pts',(-1.691877054817,1.,3.64967689827393));
#50107=CARTESIAN_POINT('Ctrl Pts',(-1.68641690471455,1.,3.64432638915199));
#50108=CARTESIAN_POINT('Ctrl Pts',(-1.68099146651577,1.,3.63895140887443));
#50109=CARTESIAN_POINT('Ctrl Pts',(-1.67560193613145,1.,3.63355343201211));
#50110=CARTESIAN_POINT('Ctrl Pts',(-1.67024966008037,1.,3.62813422105257));
#50111=CARTESIAN_POINT('Ctrl Pts',(-1.66493585923853,1.,3.62269517989104));
#50112=CARTESIAN_POINT('Ctrl Pts',(-1.65966133399186,1.,3.61723666482457));
#50113=CARTESIAN_POINT('Ctrl Pts',(-1.65442619244327,1.,3.61175734965129));
#50114=CARTESIAN_POINT('Ctrl Pts',(-1.64922952425833,1.,3.60625346556992));
#50115=CARTESIAN_POINT('Ctrl Pts',(-1.6440700438558,1.,3.6007202851384));
#50116=CARTESIAN_POINT('Ctrl Pts',(-1.63894676675349,1.,3.59515368334887));
#50117=CARTESIAN_POINT('Ctrl Pts',(-1.63385971451259,1.,3.58955176627876));
#50118=CARTESIAN_POINT('Ctrl Pts',(-1.62881051550748,1.,3.5839162577435));
#50119=CARTESIAN_POINT('Ctrl Pts',(-1.62380329464851,1.,3.57825455954405));
#50120=CARTESIAN_POINT('Ctrl Pts',(-1.61884340915412,1.,3.57257679609826));
#50121=CARTESIAN_POINT('Ctrl Pts',(-1.61393581747522,1.,3.56689200468404));
#50122=CARTESIAN_POINT('Ctrl Pts',(-1.60908344685459,1.,3.56120432482986));
#50123=CARTESIAN_POINT('Ctrl Pts',(-1.60428584699848,1.,3.55550985096117));
#50124=CARTESIAN_POINT('Ctrl Pts',(-1.59953698113444,1.,3.54979148634426));
#50125=CARTESIAN_POINT('Ctrl Pts',(-1.5948276694975,1.,3.544024581823));
#50126=CARTESIAN_POINT('Ctrl Pts',(-1.59014958368725,1.,3.53818616861045));
#50127=CARTESIAN_POINT('Ctrl Pts',(-1.58549906268083,1.,3.53226378147068));
#50128=CARTESIAN_POINT('Ctrl Pts',(-1.58088027227856,1.,3.52626275334899));
#50129=CARTESIAN_POINT('Ctrl Pts',(-1.5763104998818,1.,3.52021847865961));
#50130=CARTESIAN_POINT('Ctrl Pts',(-1.57181569799774,1.,3.51418598431733));
#50131=CARTESIAN_POINT('Ctrl Pts',(-1.56742097575041,1.,3.50821771695427));
#50132=CARTESIAN_POINT('Ctrl Pts',(-1.56314187758689,1.,3.50234321621607));
#50133=CARTESIAN_POINT('Ctrl Pts',(-1.55897703097859,1.,3.49655185179623));
#50134=CARTESIAN_POINT('Ctrl Pts',(-1.5548959590107,1.,3.49076460877317));
#50135=CARTESIAN_POINT('Ctrl Pts',(-1.55084702970382,1.,3.48485155928414));
#50136=CARTESIAN_POINT('Ctrl Pts',(-1.54678009290207,1.,3.47868272898599));
#50137=CARTESIAN_POINT('Ctrl Pts',(-1.54266605398152,1.,3.47217189224576));
#50138=CARTESIAN_POINT('Ctrl Pts',(-1.53851507915533,1.,3.46531752207222));
#50139=CARTESIAN_POINT('Ctrl Pts',(-1.53440195378902,1.,3.45825932955273));
#50140=CARTESIAN_POINT('Ctrl Pts',(-1.530462444618,1.,3.45127136828667));
#50141=CARTESIAN_POINT('Ctrl Pts',(-1.52686242875717,1.,3.44469547527));
#50142=CARTESIAN_POINT('Ctrl Pts',(-1.52377348950429,1.,3.43888895974182));
#50143=CARTESIAN_POINT('Ctrl Pts',(-1.52134826724227,1.,3.43417156977749));
#50144=CARTESIAN_POINT('Ctrl Pts',(-1.5198144909343,1.,3.4310163189349));
#50145=CARTESIAN_POINT('Ctrl Pts',(-1.51914806898539,1.,3.42946838852728));
#50146=CARTESIAN_POINT('Ctrl Pts',(-1.51895133295017,1.,3.42884302333978));
#50147=CARTESIAN_POINT('Ctrl Pts',(-1.51893924967231,1.,3.42864616361967));
#50148=CARTESIAN_POINT('Ctrl Pts',(-1.51895082866166,1.,3.42859860294378));
#50149=CARTESIAN_POINT('',(-1.83867539237861,0.,3.77614523045147));
#50150=CARTESIAN_POINT('Ctrl Pts',(-1.88088939428811,-1.,3.24418789321065));
#50151=CARTESIAN_POINT('Ctrl Pts',(-1.88088939428811,1.,3.24418789321065));
#50152=CARTESIAN_POINT('Ctrl Pts',(-1.8809110068042,-1.,3.24410359189733));
#50153=CARTESIAN_POINT('Ctrl Pts',(-1.8809110068042,1.,3.24410359189733));
#50154=CARTESIAN_POINT('Ctrl Pts',(-1.8810220187274,-1.,3.24408699284449));
#50155=CARTESIAN_POINT('Ctrl Pts',(-1.8810220187274,1.,3.24408699284449));
#50156=CARTESIAN_POINT('Ctrl Pts',(-1.88139187908347,-1.,3.24451807186964));
#50157=CARTESIAN_POINT('Ctrl Pts',(-1.88139187908347,1.,3.24451807186964));
#50158=CARTESIAN_POINT('Ctrl Pts',(-1.88229202583187,-1.,3.24600543790876));
#50159=CARTESIAN_POINT('Ctrl Pts',(-1.88229202583187,1.,3.24600543790876));
#50160=CARTESIAN_POINT('Ctrl Pts',(-1.88407708646435,-1.,3.24935200512055));
#50161=CARTESIAN_POINT('Ctrl Pts',(-1.88407708646435,1.,3.24935200512055));
#50162=CARTESIAN_POINT('Ctrl Pts',(-1.88646802523372,-1.,3.25408686339298));
#50163=CARTESIAN_POINT('Ctrl Pts',(-1.88646802523372,1.,3.25408686339298));
#50164=CARTESIAN_POINT('Ctrl Pts',(-1.88934996203508,-1.,3.2599988519361));
#50165=CARTESIAN_POINT('Ctrl Pts',(-1.88934996203508,1.,3.2599988519361));
#50166=CARTESIAN_POINT('Ctrl Pts',(-1.89255393500769,-1.,3.2667765388833));
#50167=CARTESIAN_POINT('Ctrl Pts',(-1.89255393500769,1.,3.2667765388833));
#50168=CARTESIAN_POINT('Ctrl Pts',(-1.89589172903662,-1.,3.27407108932908));
#50169=CARTESIAN_POINT('Ctrl Pts',(-1.89589172903662,1.,3.27407108932908));
#50170=CARTESIAN_POINT('Ctrl Pts',(-1.89918429230425,-1.,3.28154737912287));
#50171=CARTESIAN_POINT('Ctrl Pts',(-1.89918429230425,1.,3.28154737912287));
#50172=CARTESIAN_POINT('Ctrl Pts',(-1.9022897124757,-1.,3.28893448600364));
#50173=CARTESIAN_POINT('Ctrl Pts',(-1.9022897124757,1.,3.28893448600364));
#50174=CARTESIAN_POINT('Ctrl Pts',(-1.9051389186417,-1.,3.29608978722258));
#50175=CARTESIAN_POINT('Ctrl Pts',(-1.9051389186417,1.,3.29608978722258));
#50176=CARTESIAN_POINT('Ctrl Pts',(-1.90773912171424,-1.,3.30300595568341));
#50177=CARTESIAN_POINT('Ctrl Pts',(-1.90773912171424,1.,3.30300595568341));
#50178=CARTESIAN_POINT('Ctrl Pts',(-1.91014297830502,-1.,3.30975721158694));
#50179=CARTESIAN_POINT('Ctrl Pts',(-1.91014297830502,1.,3.30975721158694));
#50180=CARTESIAN_POINT('Ctrl Pts',(-1.91242616234459,-1.,3.31646052426395));
#50181=CARTESIAN_POINT('Ctrl Pts',(-1.91242616234459,1.,3.31646052426395));
#50182=CARTESIAN_POINT('Ctrl Pts',(-1.91466343916612,-1.,3.32323403454507));
#50183=CARTESIAN_POINT('Ctrl Pts',(-1.91466343916612,1.,3.32323403454507));
#50184=CARTESIAN_POINT('Ctrl Pts',(-1.91690081930297,-1.,3.33014884257812));
#50185=CARTESIAN_POINT('Ctrl Pts',(-1.91690081930297,1.,3.33014884257812));
#50186=CARTESIAN_POINT('Ctrl Pts',(-1.91914609610173,-1.,3.33721230709948));
#50187=CARTESIAN_POINT('Ctrl Pts',(-1.91914609610173,1.,3.33721230709948));
#50188=CARTESIAN_POINT('Ctrl Pts',(-1.92138450828378,-1.,3.34439448941915));
#50189=CARTESIAN_POINT('Ctrl Pts',(-1.92138450828378,1.,3.34439448941915));
#50190=CARTESIAN_POINT('Ctrl Pts',(-1.92358838440518,-1.,3.35164424847206));
#50191=CARTESIAN_POINT('Ctrl Pts',(-1.92358838440518,1.,3.35164424847206));
#50192=CARTESIAN_POINT('Ctrl Pts',(-1.92572846125763,-1.,3.35890824422976));
#50193=CARTESIAN_POINT('Ctrl Pts',(-1.92572846125763,1.,3.35890824422976));
#50194=CARTESIAN_POINT('Ctrl Pts',(-1.92778626543803,-1.,3.36615168657597));
#50195=CARTESIAN_POINT('Ctrl Pts',(-1.92778626543803,1.,3.36615168657597));
#50196=CARTESIAN_POINT('Ctrl Pts',(-1.92975993109897,-1.,3.37336807068078));
#50197=CARTESIAN_POINT('Ctrl Pts',(-1.92975993109897,1.,3.37336807068078));
#50198=CARTESIAN_POINT('Ctrl Pts',(-1.93165739093292,-1.,3.38056768525577));
#50199=CARTESIAN_POINT('Ctrl Pts',(-1.93165739093292,1.,3.38056768525577));
#50200=CARTESIAN_POINT('Ctrl Pts',(-1.93349233176794,-1.,3.38777076883267));
#50201=CARTESIAN_POINT('Ctrl Pts',(-1.93349233176794,1.,3.38777076883267));
#50202=CARTESIAN_POINT('Ctrl Pts',(-1.93527929945982,-1.,3.39499923640789));
#50203=CARTESIAN_POINT('Ctrl Pts',(-1.93527929945982,1.,3.39499923640789));
#50204=CARTESIAN_POINT('Ctrl Pts',(-1.93702857723089,-1.,3.40226802104093));
#50205=CARTESIAN_POINT('Ctrl Pts',(-1.93702857723089,1.,3.40226802104093));
#50206=CARTESIAN_POINT('Ctrl Pts',(-1.93874306008132,-1.,3.40957978266622));
#50207=CARTESIAN_POINT('Ctrl Pts',(-1.93874306008132,1.,3.40957978266622));
#50208=CARTESIAN_POINT('Ctrl Pts',(-1.94042111965237,-1.,3.41692971994082));
#50209=CARTESIAN_POINT('Ctrl Pts',(-1.94042111965237,1.,3.41692971994082));
#50210=CARTESIAN_POINT('Ctrl Pts',(-1.94205835913692,-1.,3.42430850941497));
#50211=CARTESIAN_POINT('Ctrl Pts',(-1.94205835913692,1.,3.42430850941497));
#50212=CARTESIAN_POINT('Ctrl Pts',(-1.94364973660285,-1.,3.43170586602436));
#50213=CARTESIAN_POINT('Ctrl Pts',(-1.94364973660285,1.,3.43170586602436));
#50214=CARTESIAN_POINT('Ctrl Pts',(-1.94519168842883,-1.,3.43911410197693));
#50215=CARTESIAN_POINT('Ctrl Pts',(-1.94519168842883,1.,3.43911410197693));
#50216=CARTESIAN_POINT('Ctrl Pts',(-1.94668377715332,-1.,3.44653088665685));
#50217=CARTESIAN_POINT('Ctrl Pts',(-1.94668377715332,1.,3.44653088665685));
#50218=CARTESIAN_POINT('Ctrl Pts',(-1.94812754766524,-1.,3.45395731584051));
#50219=CARTESIAN_POINT('Ctrl Pts',(-1.94812754766524,1.,3.45395731584051));
#50220=CARTESIAN_POINT('Ctrl Pts',(-1.94952575850196,-1.,3.46139661060959));
#50221=CARTESIAN_POINT('Ctrl Pts',(-1.94952575850196,1.,3.46139661060959));
#50222=CARTESIAN_POINT('Ctrl Pts',(-1.95088147859876,-1.,3.4688525897419));
#50223=CARTESIAN_POINT('Ctrl Pts',(-1.95088147859876,1.,3.4688525897419));
#50224=CARTESIAN_POINT('Ctrl Pts',(-1.95219722189878,-1.,3.47632820495926));
#50225=CARTESIAN_POINT('Ctrl Pts',(-1.95219722189878,1.,3.47632820495926));
#50226=CARTESIAN_POINT('Ctrl Pts',(-1.95347412486316,-1.,3.48382414832648));
#50227=CARTESIAN_POINT('Ctrl Pts',(-1.95347412486316,1.,3.48382414832648));
#50228=CARTESIAN_POINT('Ctrl Pts',(-1.95471236969653,-1.,3.49133956289154));
#50229=CARTESIAN_POINT('Ctrl Pts',(-1.95471236969653,1.,3.49133956289154));
#50230=CARTESIAN_POINT('Ctrl Pts',(-1.9559115382367,-1.,3.49887263575602));
#50231=CARTESIAN_POINT('Ctrl Pts',(-1.9559115382367,1.,3.49887263575602));
#50232=CARTESIAN_POINT('Ctrl Pts',(-1.95707099606514,-1.,3.50642124159913));
#50233=CARTESIAN_POINT('Ctrl Pts',(-1.95707099606514,1.,3.50642124159913));
#50234=CARTESIAN_POINT('Ctrl Pts',(-1.95819025316768,-1.,3.51398354617772));
#50235=CARTESIAN_POINT('Ctrl Pts',(-1.95819025316768,1.,3.51398354617772));
#50236=CARTESIAN_POINT('Ctrl Pts',(-1.95926936324436,-1.,3.52155867431438));
#50237=CARTESIAN_POINT('Ctrl Pts',(-1.95926936324436,1.,3.52155867431438));
#50238=CARTESIAN_POINT('Ctrl Pts',(-1.96030879411534,-1.,3.52914648844289));
#50239=CARTESIAN_POINT('Ctrl Pts',(-1.96030879411534,1.,3.52914648844289));
#50240=CARTESIAN_POINT('Ctrl Pts',(-1.96130926212661,-1.,3.53674730625759));
#50241=CARTESIAN_POINT('Ctrl Pts',(-1.96130926212661,1.,3.53674730625759));
#50242=CARTESIAN_POINT('Ctrl Pts',(-1.96227157573058,-1.,3.54436163300425));
#50243=CARTESIAN_POINT('Ctrl Pts',(-1.96227157573058,1.,3.54436163300425));
#50244=CARTESIAN_POINT('Ctrl Pts',(-1.96319648628667,-1.,3.55198990600929));
#50245=CARTESIAN_POINT('Ctrl Pts',(-1.96319648628667,1.,3.55198990600929));
#50246=CARTESIAN_POINT('Ctrl Pts',(-1.96408450906868,-1.,3.55963218706201));
#50247=CARTESIAN_POINT('Ctrl Pts',(-1.96408450906868,1.,3.55963218706201));
#50248=CARTESIAN_POINT('Ctrl Pts',(-1.96493594634643,-1.,3.56728820357933));
#50249=CARTESIAN_POINT('Ctrl Pts',(-1.96493594634643,1.,3.56728820357933));
#50250=CARTESIAN_POINT('Ctrl Pts',(-1.96575096652857,-1.,3.57495748601088));
#50251=CARTESIAN_POINT('Ctrl Pts',(-1.96575096652857,1.,3.57495748601088));
#50252=CARTESIAN_POINT('Ctrl Pts',(-1.9665296668894,-1.,3.58263947663884));
#50253=CARTESIAN_POINT('Ctrl Pts',(-1.9665296668894,1.,3.58263947663884));
#50254=CARTESIAN_POINT('Ctrl Pts',(-1.96727213799507,-1.,3.5903336402273));
#50255=CARTESIAN_POINT('Ctrl Pts',(-1.96727213799507,1.,3.5903336402273));
#50256=CARTESIAN_POINT('Ctrl Pts',(-1.96797854118257,-1.,3.59803959819725));
#50257=CARTESIAN_POINT('Ctrl Pts',(-1.96797854118257,1.,3.59803959819725));
#50258=CARTESIAN_POINT('Ctrl Pts',(-1.96864911885775,-1.,3.60575714017676));
#50259=CARTESIAN_POINT('Ctrl Pts',(-1.96864911885775,1.,3.60575714017676));
#50260=CARTESIAN_POINT('Ctrl Pts',(-1.96928416040712,-1.,3.61348615496393));
#50261=CARTESIAN_POINT('Ctrl Pts',(-1.96928416040712,1.,3.61348615496393));
#50262=CARTESIAN_POINT('Ctrl Pts',(-1.96988398129888,-1.,3.62122658401722));
#50263=CARTESIAN_POINT('Ctrl Pts',(-1.96988398129888,1.,3.62122658401722));
#50264=CARTESIAN_POINT('Ctrl Pts',(-1.97044889850518,-1.,3.62897836973397));
#50265=CARTESIAN_POINT('Ctrl Pts',(-1.97044889850518,1.,3.62897836973397));
#50266=CARTESIAN_POINT('Ctrl Pts',(-1.97097920454698,-1.,3.63674139590853));
#50267=CARTESIAN_POINT('Ctrl Pts',(-1.97097920454698,1.,3.63674139590853));
#50268=CARTESIAN_POINT('Ctrl Pts',(-1.97147515441539,-1.,3.64451546724221));
#50269=CARTESIAN_POINT('Ctrl Pts',(-1.97147515441539,1.,3.64451546724221));
#50270=CARTESIAN_POINT('Ctrl Pts',(-1.97193697240645,-1.,3.65230034717364));
#50271=CARTESIAN_POINT('Ctrl Pts',(-1.97193697240645,1.,3.65230034717364));
#50272=CARTESIAN_POINT('Ctrl Pts',(-1.97236485439317,-1.,3.66009578166865));
#50273=CARTESIAN_POINT('Ctrl Pts',(-1.97236485439317,1.,3.66009578166865));
#50274=CARTESIAN_POINT('Ctrl Pts',(-1.9727589719863,-1.,3.66790152751984));
#50275=CARTESIAN_POINT('Ctrl Pts',(-1.9727589719863,1.,3.66790152751984));
#50276=CARTESIAN_POINT('Ctrl Pts',(-1.97311947678035,-1.,3.67571738106175));
#50277=CARTESIAN_POINT('Ctrl Pts',(-1.97311947678035,1.,3.67571738106175));
#50278=CARTESIAN_POINT('Ctrl Pts',(-1.97344650303631,-1.,3.68354319913416));
#50279=CARTESIAN_POINT('Ctrl Pts',(-1.97344650303631,1.,3.68354319913416));
#50280=CARTESIAN_POINT('Ctrl Pts',(-1.97374016224397,-1.,3.69137888597855));
#50281=CARTESIAN_POINT('Ctrl Pts',(-1.97374016224397,1.,3.69137888597855));
#50282=CARTESIAN_POINT('Ctrl Pts',(-1.97394846382289,-1.,3.69765528558292));
#50283=CARTESIAN_POINT('Ctrl Pts',(-1.97394846382289,1.,3.69765528558292));
#50284=CARTESIAN_POINT('Ctrl Pts',(-1.97408973726149,-1.,3.70236698911837));
#50285=CARTESIAN_POINT('Ctrl Pts',(-1.97408973726149,1.,3.70236698911837));
#50286=CARTESIAN_POINT('Ctrl Pts',(-1.974177276451,-1.,3.7055100813194));
#50287=CARTESIAN_POINT('Ctrl Pts',(-1.974177276451,1.,3.7055100813194));
#50288=CARTESIAN_POINT('Ctrl Pts',(-1.97421938526992,-1.,3.70708211654725));
#50289=CARTESIAN_POINT('Ctrl Pts',(-1.97421938526992,1.,3.70708211654725));
#50290=CARTESIAN_POINT('',(-1.88097764062542,1.,3.24413672884902));
#50291=CARTESIAN_POINT('Ctrl Pts',(-1.88097764062542,-1.,3.24413672884902));
#50292=CARTESIAN_POINT('Ctrl Pts',(-1.88097764062542,-0.666666666666667,
3.24413672884902));
#50293=CARTESIAN_POINT('Ctrl Pts',(-1.88097764062542,-0.333333333333333,
3.24413672884902));
#50294=CARTESIAN_POINT('Ctrl Pts',(-1.88097764062542,0.333333333333333,
3.24413672884902));
#50295=CARTESIAN_POINT('Ctrl Pts',(-1.88097764062542,0.666666666666667,
3.24413672884902));
#50296=CARTESIAN_POINT('Ctrl Pts',(-1.88097764062542,1.,3.24413672884902));
#50297=CARTESIAN_POINT('',(-1.97421938526992,1.,3.70708211654725));
#50298=CARTESIAN_POINT('',(-1.97421938526992,0.,3.70708211654725));
#50299=CARTESIAN_POINT('Ctrl Pts',(-1.88097764062542,1.,3.24413672884902));
#50300=CARTESIAN_POINT('Ctrl Pts',(-1.88102292397987,1.,3.24415531671311));
#50301=CARTESIAN_POINT('Ctrl Pts',(-1.88117508446657,1.,3.24428080352952));
#50302=CARTESIAN_POINT('Ctrl Pts',(-1.88156537699118,1.,3.24480754675942));
#50303=CARTESIAN_POINT('Ctrl Pts',(-1.88242596600422,1.,3.24625654410705));
#50304=CARTESIAN_POINT('Ctrl Pts',(-1.88407708646435,1.,3.24935200512055));
#50305=CARTESIAN_POINT('Ctrl Pts',(-1.88646802523372,1.,3.25408686339298));
#50306=CARTESIAN_POINT('Ctrl Pts',(-1.88934996203508,1.,3.2599988519361));
#50307=CARTESIAN_POINT('Ctrl Pts',(-1.89255393500769,1.,3.2667765388833));
#50308=CARTESIAN_POINT('Ctrl Pts',(-1.89589172903662,1.,3.27407108932908));
#50309=CARTESIAN_POINT('Ctrl Pts',(-1.89918429230425,1.,3.28154737912287));
#50310=CARTESIAN_POINT('Ctrl Pts',(-1.9022897124757,1.,3.28893448600364));
#50311=CARTESIAN_POINT('Ctrl Pts',(-1.9051389186417,1.,3.29608978722258));
#50312=CARTESIAN_POINT('Ctrl Pts',(-1.90773912171424,1.,3.30300595568341));
#50313=CARTESIAN_POINT('Ctrl Pts',(-1.91014297830502,1.,3.30975721158694));
#50314=CARTESIAN_POINT('Ctrl Pts',(-1.91242616234459,1.,3.31646052426395));
#50315=CARTESIAN_POINT('Ctrl Pts',(-1.91466343916612,1.,3.32323403454507));
#50316=CARTESIAN_POINT('Ctrl Pts',(-1.91690081930297,1.,3.33014884257812));
#50317=CARTESIAN_POINT('Ctrl Pts',(-1.91914609610173,1.,3.33721230709948));
#50318=CARTESIAN_POINT('Ctrl Pts',(-1.92138450828378,1.,3.34439448941915));
#50319=CARTESIAN_POINT('Ctrl Pts',(-1.92358838440518,1.,3.35164424847206));
#50320=CARTESIAN_POINT('Ctrl Pts',(-1.92572846125763,1.,3.35890824422976));
#50321=CARTESIAN_POINT('Ctrl Pts',(-1.92778626543803,1.,3.36615168657597));
#50322=CARTESIAN_POINT('Ctrl Pts',(-1.92975993109897,1.,3.37336807068078));
#50323=CARTESIAN_POINT('Ctrl Pts',(-1.93165739093292,1.,3.38056768525577));
#50324=CARTESIAN_POINT('Ctrl Pts',(-1.93349233176794,1.,3.38777076883267));
#50325=CARTESIAN_POINT('Ctrl Pts',(-1.93527929945982,1.,3.39499923640789));
#50326=CARTESIAN_POINT('Ctrl Pts',(-1.93702857723089,1.,3.40226802104093));
#50327=CARTESIAN_POINT('Ctrl Pts',(-1.93874306008132,1.,3.40957978266622));
#50328=CARTESIAN_POINT('Ctrl Pts',(-1.94042111965237,1.,3.41692971994082));
#50329=CARTESIAN_POINT('Ctrl Pts',(-1.94205835913692,1.,3.42430850941497));
#50330=CARTESIAN_POINT('Ctrl Pts',(-1.94364973660285,1.,3.43170586602436));
#50331=CARTESIAN_POINT('Ctrl Pts',(-1.94519168842883,1.,3.43911410197693));
#50332=CARTESIAN_POINT('Ctrl Pts',(-1.94668377715332,1.,3.44653088665685));
#50333=CARTESIAN_POINT('Ctrl Pts',(-1.94812754766524,1.,3.45395731584051));
#50334=CARTESIAN_POINT('Ctrl Pts',(-1.94952575850196,1.,3.46139661060959));
#50335=CARTESIAN_POINT('Ctrl Pts',(-1.95088147859876,1.,3.4688525897419));
#50336=CARTESIAN_POINT('Ctrl Pts',(-1.95219722189878,1.,3.47632820495926));
#50337=CARTESIAN_POINT('Ctrl Pts',(-1.95347412486316,1.,3.48382414832648));
#50338=CARTESIAN_POINT('Ctrl Pts',(-1.95471236969653,1.,3.49133956289154));
#50339=CARTESIAN_POINT('Ctrl Pts',(-1.9559115382367,1.,3.49887263575602));
#50340=CARTESIAN_POINT('Ctrl Pts',(-1.95707099606514,1.,3.50642124159913));
#50341=CARTESIAN_POINT('Ctrl Pts',(-1.95819025316768,1.,3.51398354617772));
#50342=CARTESIAN_POINT('Ctrl Pts',(-1.95926936324436,1.,3.52155867431438));
#50343=CARTESIAN_POINT('Ctrl Pts',(-1.96030879411534,1.,3.52914648844289));
#50344=CARTESIAN_POINT('Ctrl Pts',(-1.96130926212661,1.,3.53674730625759));
#50345=CARTESIAN_POINT('Ctrl Pts',(-1.96227157573058,1.,3.54436163300425));
#50346=CARTESIAN_POINT('Ctrl Pts',(-1.96319648628667,1.,3.55198990600929));
#50347=CARTESIAN_POINT('Ctrl Pts',(-1.96408450906868,1.,3.55963218706201));
#50348=CARTESIAN_POINT('Ctrl Pts',(-1.96493594634643,1.,3.56728820357933));
#50349=CARTESIAN_POINT('Ctrl Pts',(-1.96575096652857,1.,3.57495748601088));
#50350=CARTESIAN_POINT('Ctrl Pts',(-1.9665296668894,1.,3.58263947663884));
#50351=CARTESIAN_POINT('Ctrl Pts',(-1.96727213799507,1.,3.5903336402273));
#50352=CARTESIAN_POINT('Ctrl Pts',(-1.96797854118257,1.,3.59803959819725));
#50353=CARTESIAN_POINT('Ctrl Pts',(-1.96864911885775,1.,3.60575714017676));
#50354=CARTESIAN_POINT('Ctrl Pts',(-1.96928416040712,1.,3.61348615496393));
#50355=CARTESIAN_POINT('Ctrl Pts',(-1.96988398129888,1.,3.62122658401722));
#50356=CARTESIAN_POINT('Ctrl Pts',(-1.97044889850518,1.,3.62897836973397));
#50357=CARTESIAN_POINT('Ctrl Pts',(-1.97097920454698,1.,3.63674139590853));
#50358=CARTESIAN_POINT('Ctrl Pts',(-1.97147515441539,1.,3.64451546724221));
#50359=CARTESIAN_POINT('Ctrl Pts',(-1.97193697240645,1.,3.65230034717364));
#50360=CARTESIAN_POINT('Ctrl Pts',(-1.97236485439317,1.,3.66009578166865));
#50361=CARTESIAN_POINT('Ctrl Pts',(-1.9727589719863,1.,3.66790152751984));
#50362=CARTESIAN_POINT('Ctrl Pts',(-1.97311947678035,1.,3.67571738106175));
#50363=CARTESIAN_POINT('Ctrl Pts',(-1.97344650303631,1.,3.68354319913416));
#50364=CARTESIAN_POINT('Ctrl Pts',(-1.97374016224397,1.,3.69137888597855));
#50365=CARTESIAN_POINT('Ctrl Pts',(-1.97394846382289,1.,3.69765528558292));
#50366=CARTESIAN_POINT('Ctrl Pts',(-1.97408973726149,1.,3.70236698911837));
#50367=CARTESIAN_POINT('Ctrl Pts',(-1.974177276451,1.,3.7055100813194));
#50368=CARTESIAN_POINT('Ctrl Pts',(-1.97421938526992,1.,3.70708211654725));
#50369=CARTESIAN_POINT('Origin',(-1.97421938526992,0.,3.70708211654725));
#50370=CARTESIAN_POINT('',(-1.83867539237861,1.,3.77614523045147));
#50371=CARTESIAN_POINT('Origin',(0.,0.,0.));
#50372=CARTESIAN_POINT('',(-2.03660101169564,1.,3.14877060440425));
#50373=CARTESIAN_POINT('Origin',(0.,1.,0.));
#50374=CARTESIAN_POINT('Ctrl Pts',(-2.03660101169564,1.,3.14877060440425));
#50375=CARTESIAN_POINT('Ctrl Pts',(-2.03660101169564,0.666666666666667,
3.14877060440425));
#50376=CARTESIAN_POINT('Ctrl Pts',(-2.03660101169564,0.333333333333333,
3.14877060440425));
#50377=CARTESIAN_POINT('Ctrl Pts',(-2.03660101169564,-0.333333333333333,
3.14877060440425));
#50378=CARTESIAN_POINT('Ctrl Pts',(-2.03660101169564,-0.666666666666667,
3.14877060440425));
#50379=CARTESIAN_POINT('Ctrl Pts',(-2.03660101169564,-1.,3.14877060440425));
#50380=CARTESIAN_POINT('Ctrl Pts',(-2.40675750623143,-1.,3.44202241512147));
#50381=CARTESIAN_POINT('Ctrl Pts',(-2.40675750623143,1.,3.44202241512147));
#50382=CARTESIAN_POINT('Ctrl Pts',(-2.40537592959345,-1.,3.44127120683402));
#50383=CARTESIAN_POINT('Ctrl Pts',(-2.40537592959345,1.,3.44127120683402));
#50384=CARTESIAN_POINT('Ctrl Pts',(-2.40261515590099,-1.,3.43976627485223));
#50385=CARTESIAN_POINT('Ctrl Pts',(-2.40261515590099,1.,3.43976627485223));
#50386=CARTESIAN_POINT('Ctrl Pts',(-2.39848113411429,-1.,3.43750133066036));
#50387=CARTESIAN_POINT('Ctrl Pts',(-2.39848113411429,1.,3.43750133066036));
#50388=CARTESIAN_POINT('Ctrl Pts',(-2.39298338805823,-1.,3.43446630680436));
#50389=CARTESIAN_POINT('Ctrl Pts',(-2.39298338805823,1.,3.43446630680436));
#50390=CARTESIAN_POINT('Ctrl Pts',(-2.38613505844641,-1.,3.43064732714472));
#50391=CARTESIAN_POINT('Ctrl Pts',(-2.38613505844641,1.,3.43064732714472));
#50392=CARTESIAN_POINT('Ctrl Pts',(-2.37931067029517,-1.,3.42680309755241));
#50393=CARTESIAN_POINT('Ctrl Pts',(-2.37931067029517,1.,3.42680309755241));
#50394=CARTESIAN_POINT('Ctrl Pts',(-2.37251035954351,-1.,3.42293356216595));
#50395=CARTESIAN_POINT('Ctrl Pts',(-2.37251035954351,1.,3.42293356216595));
#50396=CARTESIAN_POINT('Ctrl Pts',(-2.36573431470314,-1.,3.41903866635384));
#50397=CARTESIAN_POINT('Ctrl Pts',(-2.36573431470314,1.,3.41903866635384));
#50398=CARTESIAN_POINT('Ctrl Pts',(-2.35898278606449,-1.,3.4151183675076));
#50399=CARTESIAN_POINT('Ctrl Pts',(-2.35898278606449,1.,3.4151183675076));
#50400=CARTESIAN_POINT('Ctrl Pts',(-2.35225606823649,-1.,3.41117262313464));
#50401=CARTESIAN_POINT('Ctrl Pts',(-2.35225606823649,1.,3.41117262313464));
#50402=CARTESIAN_POINT('Ctrl Pts',(-2.34555447648901,-1.,3.40720137403888));
#50403=CARTESIAN_POINT('Ctrl Pts',(-2.34555447648901,1.,3.40720137403888));
#50404=CARTESIAN_POINT('Ctrl Pts',(-2.33887832342715,-1.,3.40320452776646));
#50405=CARTESIAN_POINT('Ctrl Pts',(-2.33887832342715,1.,3.40320452776646));
#50406=CARTESIAN_POINT('Ctrl Pts',(-2.33222789882601,-1.,3.39918194578115));
#50407=CARTESIAN_POINT('Ctrl Pts',(-2.33222789882601,1.,3.39918194578115));
#50408=CARTESIAN_POINT('Ctrl Pts',(-2.32560343902683,-1.,3.39513342020045));
#50409=CARTESIAN_POINT('Ctrl Pts',(-2.32560343902683,1.,3.39513342020045));
#50410=CARTESIAN_POINT('Ctrl Pts',(-2.31900513925627,-1.,3.39105869475112));
#50411=CARTESIAN_POINT('Ctrl Pts',(-2.31900513925627,1.,3.39105869475112));
#50412=CARTESIAN_POINT('Ctrl Pts',(-2.31243319489505,-1.,3.38695751492659));
#50413=CARTESIAN_POINT('Ctrl Pts',(-2.31243319489505,1.,3.38695751492659));
#50414=CARTESIAN_POINT('Ctrl Pts',(-2.30588783640389,-1.,3.38282967336676));
#50415=CARTESIAN_POINT('Ctrl Pts',(-2.30588783640389,1.,3.38282967336676));
#50416=CARTESIAN_POINT('Ctrl Pts',(-2.29936936127588,-1.,3.37867504959382));
#50417=CARTESIAN_POINT('Ctrl Pts',(-2.29936936127588,1.,3.37867504959382));
#50418=CARTESIAN_POINT('Ctrl Pts',(-2.2928781800731,-1.,3.37449367172707));
#50419=CARTESIAN_POINT('Ctrl Pts',(-2.2928781800731,1.,3.37449367172707));
#50420=CARTESIAN_POINT('Ctrl Pts',(-2.28641481081045,-1.,3.37028570206357));
#50421=CARTESIAN_POINT('Ctrl Pts',(-2.28641481081045,1.,3.37028570206357));
#50422=CARTESIAN_POINT('Ctrl Pts',(-2.27997979457968,-1.,3.36605130712978));
#50423=CARTESIAN_POINT('Ctrl Pts',(-2.27997979457968,1.,3.36605130712978));
#50424=CARTESIAN_POINT('Ctrl Pts',(-2.27357362620902,-1.,3.36179055004369));
#50425=CARTESIAN_POINT('Ctrl Pts',(-2.27357362620902,1.,3.36179055004369));
#50426=CARTESIAN_POINT('Ctrl Pts',(-2.26719668579921,-1.,3.35750328523077));
#50427=CARTESIAN_POINT('Ctrl Pts',(-2.26719668579921,1.,3.35750328523077));
#50428=CARTESIAN_POINT('Ctrl Pts',(-2.26084915222484,-1.,3.35318902552676));
#50429=CARTESIAN_POINT('Ctrl Pts',(-2.26084915222484,1.,3.35318902552676));
#50430=CARTESIAN_POINT('Ctrl Pts',(-2.25453097693524,-1.,3.34884690292342));
#50431=CARTESIAN_POINT('Ctrl Pts',(-2.25453097693524,1.,3.34884690292342));
#50432=CARTESIAN_POINT('Ctrl Pts',(-2.24824207678288,-1.,3.34447596770768));
#50433=CARTESIAN_POINT('Ctrl Pts',(-2.24824207678288,1.,3.34447596770768));
#50434=CARTESIAN_POINT('Ctrl Pts',(-2.24198249391437,-1.,3.34007543738044));
#50435=CARTESIAN_POINT('Ctrl Pts',(-2.24198249391437,1.,3.34007543738044));
#50436=CARTESIAN_POINT('Ctrl Pts',(-2.2357525632881,-1.,3.33564495756478));
#50437=CARTESIAN_POINT('Ctrl Pts',(-2.2357525632881,1.,3.33564495756478));
#50438=CARTESIAN_POINT('Ctrl Pts',(-2.22955308907221,-1.,3.33118487773593));
#50439=CARTESIAN_POINT('Ctrl Pts',(-2.22955308907221,1.,3.33118487773593));
#50440=CARTESIAN_POINT('Ctrl Pts',(-2.22338548312758,-1.,3.32669646722871));
#50441=CARTESIAN_POINT('Ctrl Pts',(-2.22338548312758,1.,3.32669646722871));
#50442=CARTESIAN_POINT('Ctrl Pts',(-2.21725135110889,-1.,3.32218125618955));
#50443=CARTESIAN_POINT('Ctrl Pts',(-2.21725135110889,1.,3.32218125618955));
#50444=CARTESIAN_POINT('Ctrl Pts',(-2.21115211847872,-1.,3.31764044024231));
#50445=CARTESIAN_POINT('Ctrl Pts',(-2.21115211847872,1.,3.31764044024231));
#50446=CARTESIAN_POINT('Ctrl Pts',(-2.20508863150608,-1.,3.3130742460895));
#50447=CARTESIAN_POINT('Ctrl Pts',(-2.20508863150608,1.,3.3130742460895));
#50448=CARTESIAN_POINT('Ctrl Pts',(-2.19906078949924,-1.,3.30848134694596));
#50449=CARTESIAN_POINT('Ctrl Pts',(-2.19906078949924,1.,3.30848134694596));
#50450=CARTESIAN_POINT('Ctrl Pts',(-2.19306710376112,-1.,3.30385816281831));
#50451=CARTESIAN_POINT('Ctrl Pts',(-2.19306710376112,1.,3.30385816281831));
#50452=CARTESIAN_POINT('Ctrl Pts',(-2.18710556500325,-1.,3.29920022557635));
#50453=CARTESIAN_POINT('Ctrl Pts',(-2.18710556500325,1.,3.29920022557635));
#50454=CARTESIAN_POINT('Ctrl Pts',(-2.18117455557062,-1.,3.29450361500484));
#50455=CARTESIAN_POINT('Ctrl Pts',(-2.18117455557062,1.,3.29450361500484));
#50456=CARTESIAN_POINT('Ctrl Pts',(-2.17527380048422,-1.,3.28976645712566));
#50457=CARTESIAN_POINT('Ctrl Pts',(-2.17527380048422,1.,3.28976645712566));
#50458=CARTESIAN_POINT('Ctrl Pts',(-2.16940517773459,-1.,3.2849901997973));
#50459=CARTESIAN_POINT('Ctrl Pts',(-2.16940517773459,1.,3.2849901997973));
#50460=CARTESIAN_POINT('Ctrl Pts',(-2.16357391934434,-1.,3.28018150841414));
#50461=CARTESIAN_POINT('Ctrl Pts',(-2.16357391934434,1.,3.28018150841414));
#50462=CARTESIAN_POINT('Ctrl Pts',(-2.15778690038359,-1.,3.27534954469206));
#50463=CARTESIAN_POINT('Ctrl Pts',(-2.15778690038359,1.,3.27534954469206));
#50464=CARTESIAN_POINT('Ctrl Pts',(-2.15205043199818,-1.,3.27050245897244));
#50465=CARTESIAN_POINT('Ctrl Pts',(-2.15205043199818,1.,3.27050245897244));
#50466=CARTESIAN_POINT('Ctrl Pts',(-2.14636805295663,-1.,3.26564388189764));
#50467=CARTESIAN_POINT('Ctrl Pts',(-2.14636805295663,1.,3.26564388189764));
#50468=CARTESIAN_POINT('Ctrl Pts',(-2.14073870754257,-1.,3.26077002641868));
#50469=CARTESIAN_POINT('Ctrl Pts',(-2.14073870754257,1.,3.26077002641868));
#50470=CARTESIAN_POINT('Ctrl Pts',(-2.13515375878786,-1.,3.25586495065027));
#50471=CARTESIAN_POINT('Ctrl Pts',(-2.13515375878786,1.,3.25586495065027));
#50472=CARTESIAN_POINT('Ctrl Pts',(-2.1296002839681,-1.,3.25090574493994));
#50473=CARTESIAN_POINT('Ctrl Pts',(-2.1296002839681,1.,3.25090574493994));
#50474=CARTESIAN_POINT('Ctrl Pts',(-2.12406646410943,-1.,3.24587102613347));
#50475=CARTESIAN_POINT('Ctrl Pts',(-2.12406646410943,1.,3.24587102613347));
#50476=CARTESIAN_POINT('Ctrl Pts',(-2.11854673326972,-1.,3.24074905517282));
#50477=CARTESIAN_POINT('Ctrl Pts',(-2.11854673326972,1.,3.24074905517282));
#50478=CARTESIAN_POINT('Ctrl Pts',(-2.11304604021784,-1.,3.23554444767115));
#50479=CARTESIAN_POINT('Ctrl Pts',(-2.11304604021784,1.,3.23554444767115));
#50480=CARTESIAN_POINT('Ctrl Pts',(-2.1075869964248,-1.,3.23028945793334));
#50481=CARTESIAN_POINT('Ctrl Pts',(-2.1075869964248,1.,3.23028945793334));
#50482=CARTESIAN_POINT('Ctrl Pts',(-2.10220384298533,-1.,3.22503437553496));
#50483=CARTESIAN_POINT('Ctrl Pts',(-2.10220384298533,1.,3.22503437553496));
#50484=CARTESIAN_POINT('Ctrl Pts',(-2.09692958434933,-1.,3.21982707347067));
#50485=CARTESIAN_POINT('Ctrl Pts',(-2.09692958434933,1.,3.21982707347067));
#50486=CARTESIAN_POINT('Ctrl Pts',(-2.0917841946046,-1.,3.2146942960168));
#50487=CARTESIAN_POINT('Ctrl Pts',(-2.0917841946046,1.,3.2146942960168));
#50488=CARTESIAN_POINT('Ctrl Pts',(-2.08676465517435,-1.,3.20962575845433));
#50489=CARTESIAN_POINT('Ctrl Pts',(-2.08676465517435,1.,3.20962575845433));
#50490=CARTESIAN_POINT('Ctrl Pts',(-2.08182850370816,-1.,3.20454818630635));
#50491=CARTESIAN_POINT('Ctrl Pts',(-2.08182850370816,1.,3.20454818630635));
#50492=CARTESIAN_POINT('Ctrl Pts',(-2.0769044187063,-1.,3.19934132835879));
#50493=CARTESIAN_POINT('Ctrl Pts',(-2.0769044187063,1.,3.19934132835879));
#50494=CARTESIAN_POINT('Ctrl Pts',(-2.07192253497765,-1.,3.19388465568113));
#50495=CARTESIAN_POINT('Ctrl Pts',(-2.07192253497765,1.,3.19388465568113));
#50496=CARTESIAN_POINT('Ctrl Pts',(-2.06684062744065,-1.,3.18809755562297));
#50497=CARTESIAN_POINT('Ctrl Pts',(-2.06684062744065,1.,3.18809755562297));
#50498=CARTESIAN_POINT('Ctrl Pts',(-2.06166849827143,-1.,3.18197692964677));
#50499=CARTESIAN_POINT('Ctrl Pts',(-2.06166849827143,1.,3.18197692964677));
#50500=CARTESIAN_POINT('Ctrl Pts',(-2.05650186773279,-1.,3.17564906975592));
#50501=CARTESIAN_POINT('Ctrl Pts',(-2.05650186773279,1.,3.17564906975592));
#50502=CARTESIAN_POINT('Ctrl Pts',(-2.05151770247452,-1.,3.16936341689859));
#50503=CARTESIAN_POINT('Ctrl Pts',(-2.05151770247452,1.,3.16936341689859));
#50504=CARTESIAN_POINT('Ctrl Pts',(-2.0469333124766,-1.,3.16343165059235));
#50505=CARTESIAN_POINT('Ctrl Pts',(-2.0469333124766,1.,3.16343165059235));
#50506=CARTESIAN_POINT('Ctrl Pts',(-2.04297406404132,-1.,3.15817983946525));
#50507=CARTESIAN_POINT('Ctrl Pts',(-2.04297406404132,1.,3.15817983946525));
#50508=CARTESIAN_POINT('Ctrl Pts',(-2.03984073791432,-1.,3.1538999167466));
#50509=CARTESIAN_POINT('Ctrl Pts',(-2.03984073791432,1.,3.1538999167466));
#50510=CARTESIAN_POINT('Ctrl Pts',(-2.03766932526171,-1.,3.15079010635326));
#50511=CARTESIAN_POINT('Ctrl Pts',(-2.03766932526171,1.,3.15079010635326));
#50512=CARTESIAN_POINT('Ctrl Pts',(-2.03675273048882,-1.,3.14931281967585));
#50513=CARTESIAN_POINT('Ctrl Pts',(-2.03675273048882,1.,3.14931281967585));
#50514=CARTESIAN_POINT('Ctrl Pts',(-2.03653654935384,-1.,3.14878756590499));
#50515=CARTESIAN_POINT('Ctrl Pts',(-2.03653654935384,1.,3.14878756590499));
#50516=CARTESIAN_POINT('Ctrl Pts',(-2.036601737578,-1.,3.14869618937138));
#50517=CARTESIAN_POINT('Ctrl Pts',(-2.036601737578,1.,3.14869618937138));
#50518=CARTESIAN_POINT('Ctrl Pts',(-2.03668666247593,-1.,3.1487152044751));
#50519=CARTESIAN_POINT('Ctrl Pts',(-2.03668666247593,1.,3.1487152044751));
#50520=CARTESIAN_POINT('',(-2.40675750623143,1.,3.44202241512147));
#50521=CARTESIAN_POINT('Ctrl Pts',(-2.40675750623143,1.,3.44202241512147));
#50522=CARTESIAN_POINT('Ctrl Pts',(-2.40537592959345,1.,3.44127120683402));
#50523=CARTESIAN_POINT('Ctrl Pts',(-2.40261515590099,1.,3.43976627485223));
#50524=CARTESIAN_POINT('Ctrl Pts',(-2.39848113411429,1.,3.43750133066036));
#50525=CARTESIAN_POINT('Ctrl Pts',(-2.39298338805823,1.,3.43446630680436));
#50526=CARTESIAN_POINT('Ctrl Pts',(-2.38613505844641,1.,3.43064732714472));
#50527=CARTESIAN_POINT('Ctrl Pts',(-2.37931067029517,1.,3.42680309755241));
#50528=CARTESIAN_POINT('Ctrl Pts',(-2.37251035954351,1.,3.42293356216595));
#50529=CARTESIAN_POINT('Ctrl Pts',(-2.36573431470314,1.,3.41903866635384));
#50530=CARTESIAN_POINT('Ctrl Pts',(-2.35898278606449,1.,3.4151183675076));
#50531=CARTESIAN_POINT('Ctrl Pts',(-2.35225606823649,1.,3.41117262313464));
#50532=CARTESIAN_POINT('Ctrl Pts',(-2.34555447648901,1.,3.40720137403888));
#50533=CARTESIAN_POINT('Ctrl Pts',(-2.33887832342715,1.,3.40320452776646));
#50534=CARTESIAN_POINT('Ctrl Pts',(-2.33222789882601,1.,3.39918194578115));
#50535=CARTESIAN_POINT('Ctrl Pts',(-2.32560343902683,1.,3.39513342020045));
#50536=CARTESIAN_POINT('Ctrl Pts',(-2.31900513925627,1.,3.39105869475112));
#50537=CARTESIAN_POINT('Ctrl Pts',(-2.31243319489505,1.,3.38695751492659));
#50538=CARTESIAN_POINT('Ctrl Pts',(-2.30588783640389,1.,3.38282967336676));
#50539=CARTESIAN_POINT('Ctrl Pts',(-2.29936936127588,1.,3.37867504959382));
#50540=CARTESIAN_POINT('Ctrl Pts',(-2.2928781800731,1.,3.37449367172707));
#50541=CARTESIAN_POINT('Ctrl Pts',(-2.28641481081045,1.,3.37028570206357));
#50542=CARTESIAN_POINT('Ctrl Pts',(-2.27997979457968,1.,3.36605130712978));
#50543=CARTESIAN_POINT('Ctrl Pts',(-2.27357362620902,1.,3.36179055004369));
#50544=CARTESIAN_POINT('Ctrl Pts',(-2.26719668579921,1.,3.35750328523077));
#50545=CARTESIAN_POINT('Ctrl Pts',(-2.26084915222484,1.,3.35318902552676));
#50546=CARTESIAN_POINT('Ctrl Pts',(-2.25453097693524,1.,3.34884690292342));
#50547=CARTESIAN_POINT('Ctrl Pts',(-2.24824207678288,1.,3.34447596770768));
#50548=CARTESIAN_POINT('Ctrl Pts',(-2.24198249391437,1.,3.34007543738044));
#50549=CARTESIAN_POINT('Ctrl Pts',(-2.2357525632881,1.,3.33564495756478));
#50550=CARTESIAN_POINT('Ctrl Pts',(-2.22955308907221,1.,3.33118487773593));
#50551=CARTESIAN_POINT('Ctrl Pts',(-2.22338548312758,1.,3.32669646722871));
#50552=CARTESIAN_POINT('Ctrl Pts',(-2.21725135110889,1.,3.32218125618955));
#50553=CARTESIAN_POINT('Ctrl Pts',(-2.21115211847872,1.,3.31764044024231));
#50554=CARTESIAN_POINT('Ctrl Pts',(-2.20508863150608,1.,3.3130742460895));
#50555=CARTESIAN_POINT('Ctrl Pts',(-2.19906078949924,1.,3.30848134694596));
#50556=CARTESIAN_POINT('Ctrl Pts',(-2.19306710376112,1.,3.30385816281831));
#50557=CARTESIAN_POINT('Ctrl Pts',(-2.18710556500325,1.,3.29920022557635));
#50558=CARTESIAN_POINT('Ctrl Pts',(-2.18117455557062,1.,3.29450361500484));
#50559=CARTESIAN_POINT('Ctrl Pts',(-2.17527380048422,1.,3.28976645712566));
#50560=CARTESIAN_POINT('Ctrl Pts',(-2.16940517773459,1.,3.2849901997973));
#50561=CARTESIAN_POINT('Ctrl Pts',(-2.16357391934434,1.,3.28018150841414));
#50562=CARTESIAN_POINT('Ctrl Pts',(-2.15778690038359,1.,3.27534954469206));
#50563=CARTESIAN_POINT('Ctrl Pts',(-2.15205043199818,1.,3.27050245897244));
#50564=CARTESIAN_POINT('Ctrl Pts',(-2.14636805295663,1.,3.26564388189764));
#50565=CARTESIAN_POINT('Ctrl Pts',(-2.14073870754257,1.,3.26077002641868));
#50566=CARTESIAN_POINT('Ctrl Pts',(-2.13515375878786,1.,3.25586495065027));
#50567=CARTESIAN_POINT('Ctrl Pts',(-2.1296002839681,1.,3.25090574493994));
#50568=CARTESIAN_POINT('Ctrl Pts',(-2.12406646410943,1.,3.24587102613347));
#50569=CARTESIAN_POINT('Ctrl Pts',(-2.11854673326972,1.,3.24074905517282));
#50570=CARTESIAN_POINT('Ctrl Pts',(-2.11304604021784,1.,3.23554444767115));
#50571=CARTESIAN_POINT('Ctrl Pts',(-2.1075869964248,1.,3.23028945793334));
#50572=CARTESIAN_POINT('Ctrl Pts',(-2.10220384298533,1.,3.22503437553496));
#50573=CARTESIAN_POINT('Ctrl Pts',(-2.09692958434933,1.,3.21982707347067));
#50574=CARTESIAN_POINT('Ctrl Pts',(-2.0917841946046,1.,3.2146942960168));
#50575=CARTESIAN_POINT('Ctrl Pts',(-2.08676465517435,1.,3.20962575845433));
#50576=CARTESIAN_POINT('Ctrl Pts',(-2.08182850370816,1.,3.20454818630635));
#50577=CARTESIAN_POINT('Ctrl Pts',(-2.0769044187063,1.,3.19934132835879));
#50578=CARTESIAN_POINT('Ctrl Pts',(-2.07192253497765,1.,3.19388465568113));
#50579=CARTESIAN_POINT('Ctrl Pts',(-2.06684062744065,1.,3.18809755562297));
#50580=CARTESIAN_POINT('Ctrl Pts',(-2.06166849827143,1.,3.18197692964677));
#50581=CARTESIAN_POINT('Ctrl Pts',(-2.05650186773279,1.,3.17564906975592));
#50582=CARTESIAN_POINT('Ctrl Pts',(-2.05151770247452,1.,3.16936341689859));
#50583=CARTESIAN_POINT('Ctrl Pts',(-2.0469333124766,1.,3.16343165059235));
#50584=CARTESIAN_POINT('Ctrl Pts',(-2.04297406404132,1.,3.15817983946525));
#50585=CARTESIAN_POINT('Ctrl Pts',(-2.03984073791432,1.,3.1538999167466));
#50586=CARTESIAN_POINT('Ctrl Pts',(-2.03783225496023,1.,3.15102344775396));
#50587=CARTESIAN_POINT('Ctrl Pts',(-2.03693188810614,1.,3.14959882629936));
#50588=CARTESIAN_POINT('Ctrl Pts',(-2.03663974554941,1.,3.14901193669147));
#50589=CARTESIAN_POINT('Ctrl Pts',(-2.03659701539175,1.,3.1488193908823));
#50590=CARTESIAN_POINT('Ctrl Pts',(-2.03660101169564,1.,3.14877060440425));
#50591=CARTESIAN_POINT('',(-2.40675750623143,0.,3.44202241512147));
#50592=CARTESIAN_POINT('Ctrl Pts',(-2.36523532225181,-1.,2.91001063062876));
#50593=CARTESIAN_POINT('Ctrl Pts',(-2.36523532225181,1.,2.91001063062876));
#50594=CARTESIAN_POINT('Ctrl Pts',(-2.36524348105112,-1.,2.90992398626211));
#50595=CARTESIAN_POINT('Ctrl Pts',(-2.36524348105112,1.,2.90992398626211));
#50596=CARTESIAN_POINT('Ctrl Pts',(-2.36535052956938,-1.,2.90989022548032));
#50597=CARTESIAN_POINT('Ctrl Pts',(-2.36535052956938,1.,2.90989022548032));
#50598=CARTESIAN_POINT('Ctrl Pts',(-2.36578327194741,-1.,2.91025813830041));
#50599=CARTESIAN_POINT('Ctrl Pts',(-2.36578327194741,1.,2.91025813830041));
#50600=CARTESIAN_POINT('Ctrl Pts',(-2.36690501170627,-1.,2.9115863784204));
#50601=CARTESIAN_POINT('Ctrl Pts',(-2.36690501170627,1.,2.9115863784204));
#50602=CARTESIAN_POINT('Ctrl Pts',(-2.36919161373173,-1.,2.9146124988314));
#50603=CARTESIAN_POINT('Ctrl Pts',(-2.36919161373173,1.,2.9146124988314));
#50604=CARTESIAN_POINT('Ctrl Pts',(-2.37229381109821,-1.,2.91891503791411));
#50605=CARTESIAN_POINT('Ctrl Pts',(-2.37229381109821,1.,2.91891503791411));
#50606=CARTESIAN_POINT('Ctrl Pts',(-2.3760651052403,-1.,2.92430340582608));
#50607=CARTESIAN_POINT('Ctrl Pts',(-2.3760651052403,1.,2.92430340582608));
#50608=CARTESIAN_POINT('Ctrl Pts',(-2.38028989582073,-1.,2.93049643640206));
#50609=CARTESIAN_POINT('Ctrl Pts',(-2.38028989582073,1.,2.93049643640206));
#50610=CARTESIAN_POINT('Ctrl Pts',(-2.38472771516311,-1.,2.93717903280391));
#50611=CARTESIAN_POINT('Ctrl Pts',(-2.38472771516311,1.,2.93717903280391));
#50612=CARTESIAN_POINT('Ctrl Pts',(-2.38914929090759,-1.,2.94404820669076));
#50613=CARTESIAN_POINT('Ctrl Pts',(-2.38914929090759,1.,2.94404820669076));
#50614=CARTESIAN_POINT('Ctrl Pts',(-2.39337207631667,-1.,2.95085857128439));
#50615=CARTESIAN_POINT('Ctrl Pts',(-2.39337207631667,1.,2.95085857128439));
#50616=CARTESIAN_POINT('Ctrl Pts',(-2.39730553974517,-1.,2.95748006482942));
#50617=CARTESIAN_POINT('Ctrl Pts',(-2.39730553974517,1.,2.95748006482942));
#50618=CARTESIAN_POINT('Ctrl Pts',(-2.4009556571164,-1.,2.96390432240312));
#50619=CARTESIAN_POINT('Ctrl Pts',(-2.4009556571164,1.,2.96390432240312));
#50620=CARTESIAN_POINT('Ctrl Pts',(-2.40438604734919,-1.,2.9701964131236));
#50621=CARTESIAN_POINT('Ctrl Pts',(-2.40438604734919,1.,2.9701964131236));
#50622=CARTESIAN_POINT('Ctrl Pts',(-2.40768975073713,-1.,2.97646002822422));
#50623=CARTESIAN_POINT('Ctrl Pts',(-2.40768975073713,1.,2.97646002822422));
#50624=CARTESIAN_POINT('Ctrl Pts',(-2.41095909342571,-1.,2.98280015815107));
#50625=CARTESIAN_POINT('Ctrl Pts',(-2.41095909342571,1.,2.98280015815107));
#50626=CARTESIAN_POINT('Ctrl Pts',(-2.41425064199586,-1.,2.98927983005796));
#50627=CARTESIAN_POINT('Ctrl Pts',(-2.41425064199586,1.,2.98927983005796));
#50628=CARTESIAN_POINT('Ctrl Pts',(-2.41757324500514,-1.,2.99590509293503));
#50629=CARTESIAN_POINT('Ctrl Pts',(-2.41757324500514,1.,2.99590509293503));
#50630=CARTESIAN_POINT('Ctrl Pts',(-2.42090763946779,-1.,3.00264868585996));
#50631=CARTESIAN_POINT('Ctrl Pts',(-2.42090763946779,1.,3.00264868585996));
#50632=CARTESIAN_POINT('Ctrl Pts',(-2.42421849439613,-1.,3.00946442616658));
#50633=CARTESIAN_POINT('Ctrl Pts',(-2.42421849439613,1.,3.00946442616658));
#50634=CARTESIAN_POINT('Ctrl Pts',(-2.42746856264168,-1.,3.01630420830504));
#50635=CARTESIAN_POINT('Ctrl Pts',(-2.42746856264168,1.,3.01630420830504));
#50636=CARTESIAN_POINT('Ctrl Pts',(-2.43063415586637,-1.,3.02313656036004));
#50637=CARTESIAN_POINT('Ctrl Pts',(-2.43063415586637,1.,3.02313656036004));
#50638=CARTESIAN_POINT('Ctrl Pts',(-2.43371241361488,-1.,3.02995534946978));
#50639=CARTESIAN_POINT('Ctrl Pts',(-2.43371241361488,1.,3.02995534946978));
#50640=CARTESIAN_POINT('Ctrl Pts',(-2.43671278042414,-1.,3.03676949672821));
#50641=CARTESIAN_POINT('Ctrl Pts',(-2.43671278042414,1.,3.03676949672821));
#50642=CARTESIAN_POINT('Ctrl Pts',(-2.43965194061857,-1.,3.04359685040555));
#50643=CARTESIAN_POINT('Ctrl Pts',(-2.43965194061857,1.,3.04359685040555));
#50644=CARTESIAN_POINT('Ctrl Pts',(-2.44254768923105,-1.,3.05045678021504));
#50645=CARTESIAN_POINT('Ctrl Pts',(-2.44254768923105,1.,3.05045678021504));
#50646=CARTESIAN_POINT('Ctrl Pts',(-2.44541251892556,-1.,3.05736242671506));
#50647=CARTESIAN_POINT('Ctrl Pts',(-2.44541251892556,1.,3.05736242671506));
#50648=CARTESIAN_POINT('Ctrl Pts',(-2.44824970516544,-1.,3.06431596421405));
#50649=CARTESIAN_POINT('Ctrl Pts',(-2.44824970516544,1.,3.06431596421405));
#50650=CARTESIAN_POINT('Ctrl Pts',(-2.45105688854422,-1.,3.07131290521297));
#50651=CARTESIAN_POINT('Ctrl Pts',(-2.45105688854422,1.,3.07131290521297));
#50652=CARTESIAN_POINT('Ctrl Pts',(-2.4538282678779,-1.,3.07834472886139));
#50653=CARTESIAN_POINT('Ctrl Pts',(-2.4538282678779,1.,3.07834472886139));
#50654=CARTESIAN_POINT('Ctrl Pts',(-2.45655725437039,-1.,3.08540206545315));
#50655=CARTESIAN_POINT('Ctrl Pts',(-2.45655725437039,1.,3.08540206545315));
#50656=CARTESIAN_POINT('Ctrl Pts',(-2.4592391256388,-1.,3.09247787931887));
#50657=CARTESIAN_POINT('Ctrl Pts',(-2.4592391256388,1.,3.09247787931887));
#50658=CARTESIAN_POINT('Ctrl Pts',(-2.46187308501884,-1.,3.09956993697052));
#50659=CARTESIAN_POINT('Ctrl Pts',(-2.46187308501884,1.,3.09956993697052));
#50660=CARTESIAN_POINT('Ctrl Pts',(-2.46446082979646,-1.,3.1066790790198));
#50661=CARTESIAN_POINT('Ctrl Pts',(-2.46446082979646,1.,3.1066790790198));
#50662=CARTESIAN_POINT('Ctrl Pts',(-2.46700558843506,-1.,3.11380805536122));
#50663=CARTESIAN_POINT('Ctrl Pts',(-2.46700558843506,1.,3.11380805536122));
#50664=CARTESIAN_POINT('Ctrl Pts',(-2.46951098947469,-1.,3.12096015766983));
#50665=CARTESIAN_POINT('Ctrl Pts',(-2.46951098947469,1.,3.12096015766983));
#50666=CARTESIAN_POINT('Ctrl Pts',(-2.47197997765871,-1.,3.12813790805952));
#50667=CARTESIAN_POINT('Ctrl Pts',(-2.47197997765871,1.,3.12813790805952));
#50668=CARTESIAN_POINT('Ctrl Pts',(-2.47441378371932,-1.,3.13534181229295));
#50669=CARTESIAN_POINT('Ctrl Pts',(-2.47441378371932,1.,3.13534181229295));
#50670=CARTESIAN_POINT('Ctrl Pts',(-2.47681245356109,-1.,3.1425709954655));
#50671=CARTESIAN_POINT('Ctrl Pts',(-2.47681245356109,1.,3.1425709954655));
#50672=CARTESIAN_POINT('Ctrl Pts',(-2.47917529057029,-1.,3.14982373241352));
#50673=CARTESIAN_POINT('Ctrl Pts',(-2.47917529057029,1.,3.14982373241352));
#50674=CARTESIAN_POINT('Ctrl Pts',(-2.48150133566571,-1.,3.15709802322739));
#50675=CARTESIAN_POINT('Ctrl Pts',(-2.48150133566571,1.,3.15709802322739));
#50676=CARTESIAN_POINT('Ctrl Pts',(-2.48378981792725,-1.,3.16439213290161));
#50677=CARTESIAN_POINT('Ctrl Pts',(-2.48378981792725,1.,3.16439213290161));
#50678=CARTESIAN_POINT('Ctrl Pts',(-2.48604065348587,-1.,3.17170518863313));
#50679=CARTESIAN_POINT('Ctrl Pts',(-2.48604065348587,1.,3.17170518863313));
#50680=CARTESIAN_POINT('Ctrl Pts',(-2.48825428288201,-1.,3.17903698136622));
#50681=CARTESIAN_POINT('Ctrl Pts',(-2.48825428288201,1.,3.17903698136622));
#50682=CARTESIAN_POINT('Ctrl Pts',(-2.49043146334059,-1.,3.18638771282266));
#50683=CARTESIAN_POINT('Ctrl Pts',(-2.49043146334059,1.,3.18638771282266));
#50684=CARTESIAN_POINT('Ctrl Pts',(-2.49257307239848,-1.,3.19375775555798));
#50685=CARTESIAN_POINT('Ctrl Pts',(-2.49257307239848,1.,3.19375775555798));
#50686=CARTESIAN_POINT('Ctrl Pts',(-2.49467992057755,-1.,3.20114742397588));
#50687=CARTESIAN_POINT('Ctrl Pts',(-2.49467992057755,1.,3.20114742397588));
#50688=CARTESIAN_POINT('Ctrl Pts',(-2.4967525264737,-1.,3.20855669849836));
#50689=CARTESIAN_POINT('Ctrl Pts',(-2.4967525264737,1.,3.20855669849836));
#50690=CARTESIAN_POINT('Ctrl Pts',(-2.4987911459939,-1.,3.21598526261286));
#50691=CARTESIAN_POINT('Ctrl Pts',(-2.4987911459939,1.,3.21598526261286));
#50692=CARTESIAN_POINT('Ctrl Pts',(-2.50079587201957,-1.,3.22343262620503));
#50693=CARTESIAN_POINT('Ctrl Pts',(-2.50079587201957,1.,3.22343262620503));
#50694=CARTESIAN_POINT('Ctrl Pts',(-2.50276671338111,-1.,3.23089822320646));
#50695=CARTESIAN_POINT('Ctrl Pts',(-2.50276671338111,1.,3.23089822320646));
#50696=CARTESIAN_POINT('Ctrl Pts',(-2.5047036758003,-1.,3.23838151080319));
#50697=CARTESIAN_POINT('Ctrl Pts',(-2.5047036758003,1.,3.23838151080319));
#50698=CARTESIAN_POINT('Ctrl Pts',(-2.506606859405,-1.,3.24588208983849));
#50699=CARTESIAN_POINT('Ctrl Pts',(-2.506606859405,1.,3.24588208983849));
#50700=CARTESIAN_POINT('Ctrl Pts',(-2.50847647070723,-1.,3.25339971460982));
#50701=CARTESIAN_POINT('Ctrl Pts',(-2.50847647070723,1.,3.25339971460982));
#50702=CARTESIAN_POINT('Ctrl Pts',(-2.51031277813486,-1.,3.26093423001434));
#50703=CARTESIAN_POINT('Ctrl Pts',(-2.51031277813486,1.,3.26093423001434));
#50704=CARTESIAN_POINT('Ctrl Pts',(-2.51211608411423,-1.,3.26848552888115));
#50705=CARTESIAN_POINT('Ctrl Pts',(-2.51211608411423,1.,3.26848552888115));
#50706=CARTESIAN_POINT('Ctrl Pts',(-2.513886692704,-1.,3.27605350473142));
#50707=CARTESIAN_POINT('Ctrl Pts',(-2.513886692704,1.,3.27605350473142));
#50708=CARTESIAN_POINT('Ctrl Pts',(-2.51562487464514,-1.,3.28363799702982));
#50709=CARTESIAN_POINT('Ctrl Pts',(-2.51562487464514,1.,3.28363799702982));
#50710=CARTESIAN_POINT('Ctrl Pts',(-2.51733085123797,-1.,3.2912387729927));
#50711=CARTESIAN_POINT('Ctrl Pts',(-2.51733085123797,1.,3.2912387729927));
#50712=CARTESIAN_POINT('Ctrl Pts',(-2.51900480701069,-1.,3.29885556388352));
#50713=CARTESIAN_POINT('Ctrl Pts',(-2.51900480701069,1.,3.29885556388352));
#50714=CARTESIAN_POINT('Ctrl Pts',(-2.52064689568511,-1.,3.30648808815442));
#50715=CARTESIAN_POINT('Ctrl Pts',(-2.52064689568511,1.,3.30648808815442));
#50716=CARTESIAN_POINT('Ctrl Pts',(-2.52225724871313,-1.,3.31413607874645));
#50717=CARTESIAN_POINT('Ctrl Pts',(-2.52225724871313,1.,3.31413607874645));
#50718=CARTESIAN_POINT('Ctrl Pts',(-2.5238359839626,-1.,3.32179931078699));
#50719=CARTESIAN_POINT('Ctrl Pts',(-2.5238359839626,1.,3.32179931078699));
#50720=CARTESIAN_POINT('Ctrl Pts',(-2.52538321164634,-1.,3.32947762187533));
#50721=CARTESIAN_POINT('Ctrl Pts',(-2.52538321164634,1.,3.32947762187533));
#50722=CARTESIAN_POINT('Ctrl Pts',(-2.52689902690158,-1.,3.33717089999103));
#50723=CARTESIAN_POINT('Ctrl Pts',(-2.52689902690158,1.,3.33717089999103));
#50724=CARTESIAN_POINT('Ctrl Pts',(-2.52808660915689,-1.,3.34333744115511));
#50725=CARTESIAN_POINT('Ctrl Pts',(-2.52808660915689,1.,3.34333744115511));
#50726=CARTESIAN_POINT('Ctrl Pts',(-2.52896321610703,-1.,3.34796903576663));
#50727=CARTESIAN_POINT('Ctrl Pts',(-2.52896321610703,1.,3.34796903576663));
#50728=CARTESIAN_POINT('Ctrl Pts',(-2.5295413654909,-1.,3.35105973714071));
#50729=CARTESIAN_POINT('Ctrl Pts',(-2.5295413654909,1.,3.35105973714071));
#50730=CARTESIAN_POINT('Ctrl Pts',(-2.52982887637028,-1.,3.35260583073571));
#50731=CARTESIAN_POINT('Ctrl Pts',(-2.52982887637028,1.,3.35260583073571));
#50732=CARTESIAN_POINT('',(-2.36531447826073,1.,2.90994629141676));
#50733=CARTESIAN_POINT('Ctrl Pts',(-2.36531447826073,-1.,2.90994629141676));
#50734=CARTESIAN_POINT('Ctrl Pts',(-2.36531447826073,-0.666666666666667,
2.90994629141676));
#50735=CARTESIAN_POINT('Ctrl Pts',(-2.36531447826073,-0.333333333333333,
2.90994629141676));
#50736=CARTESIAN_POINT('Ctrl Pts',(-2.36531447826073,0.333333333333333,
2.90994629141676));
#50737=CARTESIAN_POINT('Ctrl Pts',(-2.36531447826073,0.666666666666667,
2.90994629141676));
#50738=CARTESIAN_POINT('Ctrl Pts',(-2.36531447826073,1.,2.90994629141676));
#50739=CARTESIAN_POINT('',(-2.52982887637028,1.,3.35260583073571));
#50740=CARTESIAN_POINT('',(-2.52982887637028,0.,3.35260583073571));
#50741=CARTESIAN_POINT('Ctrl Pts',(-2.36531447826073,1.,2.90994629141676));
#50742=CARTESIAN_POINT('Ctrl Pts',(-2.36536211188453,1.,2.90995756655606));
#50743=CARTESIAN_POINT('Ctrl Pts',(-2.36553202948613,1.,2.91005770527719));
#50744=CARTESIAN_POINT('Ctrl Pts',(-2.36599991765749,1.,2.91051690822156));
#50745=CARTESIAN_POINT('Ctrl Pts',(-2.36707658451664,1.,2.91181344022549));
#50746=CARTESIAN_POINT('Ctrl Pts',(-2.36919161373173,1.,2.9146124988314));
#50747=CARTESIAN_POINT('Ctrl Pts',(-2.37229381109821,1.,2.91891503791411));
#50748=CARTESIAN_POINT('Ctrl Pts',(-2.3760651052403,1.,2.92430340582608));
#50749=CARTESIAN_POINT('Ctrl Pts',(-2.38028989582073,1.,2.93049643640206));
#50750=CARTESIAN_POINT('Ctrl Pts',(-2.38472771516311,1.,2.93717903280391));
#50751=CARTESIAN_POINT('Ctrl Pts',(-2.38914929090759,1.,2.94404820669076));
#50752=CARTESIAN_POINT('Ctrl Pts',(-2.39337207631667,1.,2.95085857128439));
#50753=CARTESIAN_POINT('Ctrl Pts',(-2.39730553974517,1.,2.95748006482942));
#50754=CARTESIAN_POINT('Ctrl Pts',(-2.4009556571164,1.,2.96390432240312));
#50755=CARTESIAN_POINT('Ctrl Pts',(-2.40438604734919,1.,2.9701964131236));
#50756=CARTESIAN_POINT('Ctrl Pts',(-2.40768975073713,1.,2.97646002822422));
#50757=CARTESIAN_POINT('Ctrl Pts',(-2.41095909342571,1.,2.98280015815107));
#50758=CARTESIAN_POINT('Ctrl Pts',(-2.41425064199586,1.,2.98927983005796));
#50759=CARTESIAN_POINT('Ctrl Pts',(-2.41757324500514,1.,2.99590509293503));
#50760=CARTESIAN_POINT('Ctrl Pts',(-2.42090763946779,1.,3.00264868585996));
#50761=CARTESIAN_POINT('Ctrl Pts',(-2.42421849439613,1.,3.00946442616658));
#50762=CARTESIAN_POINT('Ctrl Pts',(-2.42746856264168,1.,3.01630420830504));
#50763=CARTESIAN_POINT('Ctrl Pts',(-2.43063415586637,1.,3.02313656036004));
#50764=CARTESIAN_POINT('Ctrl Pts',(-2.43371241361488,1.,3.02995534946978));
#50765=CARTESIAN_POINT('Ctrl Pts',(-2.43671278042414,1.,3.03676949672821));
#50766=CARTESIAN_POINT('Ctrl Pts',(-2.43965194061857,1.,3.04359685040555));
#50767=CARTESIAN_POINT('Ctrl Pts',(-2.44254768923105,1.,3.05045678021504));
#50768=CARTESIAN_POINT('Ctrl Pts',(-2.44541251892556,1.,3.05736242671506));
#50769=CARTESIAN_POINT('Ctrl Pts',(-2.44824970516544,1.,3.06431596421405));
#50770=CARTESIAN_POINT('Ctrl Pts',(-2.45105688854422,1.,3.07131290521297));
#50771=CARTESIAN_POINT('Ctrl Pts',(-2.4538282678779,1.,3.07834472886139));
#50772=CARTESIAN_POINT('Ctrl Pts',(-2.45655725437039,1.,3.08540206545315));
#50773=CARTESIAN_POINT('Ctrl Pts',(-2.4592391256388,1.,3.09247787931887));
#50774=CARTESIAN_POINT('Ctrl Pts',(-2.46187308501884,1.,3.09956993697052));
#50775=CARTESIAN_POINT('Ctrl Pts',(-2.46446082979646,1.,3.1066790790198));
#50776=CARTESIAN_POINT('Ctrl Pts',(-2.46700558843506,1.,3.11380805536122));
#50777=CARTESIAN_POINT('Ctrl Pts',(-2.46951098947469,1.,3.12096015766983));
#50778=CARTESIAN_POINT('Ctrl Pts',(-2.47197997765871,1.,3.12813790805952));
#50779=CARTESIAN_POINT('Ctrl Pts',(-2.47441378371932,1.,3.13534181229295));
#50780=CARTESIAN_POINT('Ctrl Pts',(-2.47681245356109,1.,3.1425709954655));
#50781=CARTESIAN_POINT('Ctrl Pts',(-2.47917529057029,1.,3.14982373241352));
#50782=CARTESIAN_POINT('Ctrl Pts',(-2.48150133566571,1.,3.15709802322739));
#50783=CARTESIAN_POINT('Ctrl Pts',(-2.48378981792725,1.,3.16439213290161));
#50784=CARTESIAN_POINT('Ctrl Pts',(-2.48604065348587,1.,3.17170518863313));
#50785=CARTESIAN_POINT('Ctrl Pts',(-2.48825428288201,1.,3.17903698136622));
#50786=CARTESIAN_POINT('Ctrl Pts',(-2.49043146334059,1.,3.18638771282266));
#50787=CARTESIAN_POINT('Ctrl Pts',(-2.49257307239848,1.,3.19375775555798));
#50788=CARTESIAN_POINT('Ctrl Pts',(-2.49467992057755,1.,3.20114742397588));
#50789=CARTESIAN_POINT('Ctrl Pts',(-2.4967525264737,1.,3.20855669849836));
#50790=CARTESIAN_POINT('Ctrl Pts',(-2.4987911459939,1.,3.21598526261286));
#50791=CARTESIAN_POINT('Ctrl Pts',(-2.50079587201957,1.,3.22343262620503));
#50792=CARTESIAN_POINT('Ctrl Pts',(-2.50276671338111,1.,3.23089822320646));
#50793=CARTESIAN_POINT('Ctrl Pts',(-2.5047036758003,1.,3.23838151080319));
#50794=CARTESIAN_POINT('Ctrl Pts',(-2.506606859405,1.,3.24588208983849));
#50795=CARTESIAN_POINT('Ctrl Pts',(-2.50847647070723,1.,3.25339971460982));
#50796=CARTESIAN_POINT('Ctrl Pts',(-2.51031277813486,1.,3.26093423001434));
#50797=CARTESIAN_POINT('Ctrl Pts',(-2.51211608411423,1.,3.26848552888115));
#50798=CARTESIAN_POINT('Ctrl Pts',(-2.513886692704,1.,3.27605350473142));
#50799=CARTESIAN_POINT('Ctrl Pts',(-2.51562487464514,1.,3.28363799702982));
#50800=CARTESIAN_POINT('Ctrl Pts',(-2.51733085123797,1.,3.2912387729927));
#50801=CARTESIAN_POINT('Ctrl Pts',(-2.51900480701069,1.,3.29885556388352));
#50802=CARTESIAN_POINT('Ctrl Pts',(-2.52064689568511,1.,3.30648808815442));
#50803=CARTESIAN_POINT('Ctrl Pts',(-2.52225724871313,1.,3.31413607874645));
#50804=CARTESIAN_POINT('Ctrl Pts',(-2.5238359839626,1.,3.32179931078699));
#50805=CARTESIAN_POINT('Ctrl Pts',(-2.52538321164634,1.,3.32947762187533));
#50806=CARTESIAN_POINT('Ctrl Pts',(-2.52689902690158,1.,3.33717089999103));
#50807=CARTESIAN_POINT('Ctrl Pts',(-2.52808660915689,1.,3.34333744115511));
#50808=CARTESIAN_POINT('Ctrl Pts',(-2.52896321610703,1.,3.34796903576663));
#50809=CARTESIAN_POINT('Ctrl Pts',(-2.5295413654909,1.,3.35105973714071));
#50810=CARTESIAN_POINT('Ctrl Pts',(-2.52982887637028,1.,3.35260583073571));
#50811=CARTESIAN_POINT('Origin',(-2.52982887637028,0.,3.35260583073571));
#50812=CARTESIAN_POINT('',(-2.40675750623143,1.,3.44202241512147));
#50813=CARTESIAN_POINT('Origin',(0.,0.,0.));
#50814=CARTESIAN_POINT('',(-2.50410331873042,1.,2.79140942341378));
#50815=CARTESIAN_POINT('Origin',(0.,1.,0.));
#50816=CARTESIAN_POINT('Ctrl Pts',(-2.50410331873042,1.,2.79140942341378));
#50817=CARTESIAN_POINT('Ctrl Pts',(-2.50410331873042,0.666666666666667,
2.79140942341378));
#50818=CARTESIAN_POINT('Ctrl Pts',(-2.50410331873043,0.333333333333333,
2.79140942341378));
#50819=CARTESIAN_POINT('Ctrl Pts',(-2.50410331873043,-0.333333333333333,
2.79140942341378));
#50820=CARTESIAN_POINT('Ctrl Pts',(-2.50410331873043,-0.666666666666667,
2.79140942341378));
#50821=CARTESIAN_POINT('Ctrl Pts',(-2.50410331873043,-1.,2.79140942341378));
#50822=CARTESIAN_POINT('Ctrl Pts',(-2.91557726271063,-1.,3.02314558451372));
#50823=CARTESIAN_POINT('Ctrl Pts',(-2.91557726271063,1.,3.02314558451372));
#50824=CARTESIAN_POINT('Ctrl Pts',(-2.91409518070707,-1.,3.02261975104912));
#50825=CARTESIAN_POINT('Ctrl Pts',(-2.91409518070707,1.,3.02261975104912));
#50826=CARTESIAN_POINT('Ctrl Pts',(-2.91113297349052,-1.,3.02156522743299));
#50827=CARTESIAN_POINT('Ctrl Pts',(-2.91113297349052,1.,3.02156522743299));
#50828=CARTESIAN_POINT('Ctrl Pts',(-2.90669553303902,-1.,3.01997487194926));
#50829=CARTESIAN_POINT('Ctrl Pts',(-2.90669553303902,1.,3.01997487194926));
#50830=CARTESIAN_POINT('Ctrl Pts',(-2.90079069102661,-1.,3.01783725123646));
#50831=CARTESIAN_POINT('Ctrl Pts',(-2.90079069102661,1.,3.01783725123646));
#50832=CARTESIAN_POINT('Ctrl Pts',(-2.8934292556764,-1.,3.01513660433291));
#50833=CARTESIAN_POINT('Ctrl Pts',(-2.8934292556764,1.,3.01513660433291));
#50834=CARTESIAN_POINT('Ctrl Pts',(-2.88608751706796,-1.,3.01240727309568));
#50835=CARTESIAN_POINT('Ctrl Pts',(-2.88608751706796,1.,3.01240727309568));
#50836=CARTESIAN_POINT('Ctrl Pts',(-2.87876560072799,-1.,3.0096491810855));
#50837=CARTESIAN_POINT('Ctrl Pts',(-2.87876560072799,1.,3.0096491810855));
#50838=CARTESIAN_POINT('Ctrl Pts',(-2.87146368430104,-1.,3.00686224485374));
#50839=CARTESIAN_POINT('Ctrl Pts',(-2.87146368430104,1.,3.00686224485374));
#50840=CARTESIAN_POINT('Ctrl Pts',(-2.86418200833065,-1.,3.00404638316245));
#50841=CARTESIAN_POINT('Ctrl Pts',(-2.86418200833065,1.,3.00404638316245));
#50842=CARTESIAN_POINT('Ctrl Pts',(-2.85692085715129,-1.,3.0012015079552));
#50843=CARTESIAN_POINT('Ctrl Pts',(-2.85692085715129,1.,3.0012015079552));
#50844=CARTESIAN_POINT('Ctrl Pts',(-2.84968053289104,-1.,2.99832751144566));
#50845=CARTESIAN_POINT('Ctrl Pts',(-2.84968053289104,1.,2.99832751144566));
#50846=CARTESIAN_POINT('Ctrl Pts',(-2.84246132984334,-1.,2.995424253416));
#50847=CARTESIAN_POINT('Ctrl Pts',(-2.84246132984334,1.,2.995424253416));
#50848=CARTESIAN_POINT('Ctrl Pts',(-2.83526351254383,-1.,2.99249155170479));
#50849=CARTESIAN_POINT('Ctrl Pts',(-2.83526351254383,1.,2.99249155170479));
#50850=CARTESIAN_POINT('Ctrl Pts',(-2.82808728190402,-1.,2.98952916401699));
#50851=CARTESIAN_POINT('Ctrl Pts',(-2.82808728190402,1.,2.98952916401699));
#50852=CARTESIAN_POINT('Ctrl Pts',(-2.82093279065704,-1.,2.98653680669434));
#50853=CARTESIAN_POINT('Ctrl Pts',(-2.82093279065704,1.,2.98653680669434));
#50854=CARTESIAN_POINT('Ctrl Pts',(-2.81380019196454,-1.,2.9835141977994));
#50855=CARTESIAN_POINT('Ctrl Pts',(-2.81380019196454,1.,2.9835141977994));
#50856=CARTESIAN_POINT('Ctrl Pts',(-2.80668968101162,-1.,2.98046109647299));
#50857=CARTESIAN_POINT('Ctrl Pts',(-2.80668968101162,1.,2.98046109647299));
#50858=CARTESIAN_POINT('Ctrl Pts',(-2.79960153278186,-1.,2.97737733718242));
#50859=CARTESIAN_POINT('Ctrl Pts',(-2.79960153278186,1.,2.97737733718242));
#50860=CARTESIAN_POINT('Ctrl Pts',(-2.79253615718147,-1.,2.97426288347475));
#50861=CARTESIAN_POINT('Ctrl Pts',(-2.79253615718147,1.,2.97426288347475));
#50862=CARTESIAN_POINT('Ctrl Pts',(-2.78549409123657,-1.,2.97111781461349));
#50863=CARTESIAN_POINT('Ctrl Pts',(-2.78549409123657,1.,2.97111781461349));
#50864=CARTESIAN_POINT('Ctrl Pts',(-2.77847589542767,-1.,2.9679422104295));
#50865=CARTESIAN_POINT('Ctrl Pts',(-2.77847589542767,1.,2.9679422104295));
#50866=CARTESIAN_POINT('Ctrl Pts',(-2.77148206836464,-1.,2.96473605585548));
#50867=CARTESIAN_POINT('Ctrl Pts',(-2.77148206836464,1.,2.96473605585548));
#50868=CARTESIAN_POINT('Ctrl Pts',(-2.76451296269571,-1.,2.96149914764832));
#50869=CARTESIAN_POINT('Ctrl Pts',(-2.76451296269571,1.,2.96149914764832));
#50870=CARTESIAN_POINT('Ctrl Pts',(-2.75756867888393,-1.,2.9582309766594));
#50871=CARTESIAN_POINT('Ctrl Pts',(-2.75756867888393,1.,2.9582309766594));
#50872=CARTESIAN_POINT('Ctrl Pts',(-2.75064903318996,-1.,2.95493069316211));
#50873=CARTESIAN_POINT('Ctrl Pts',(-2.75064903318996,1.,2.95493069316211));
#50874=CARTESIAN_POINT('Ctrl Pts',(-2.7437537949221,-1.,2.95159737214305));
#50875=CARTESIAN_POINT('Ctrl Pts',(-2.7437537949221,1.,2.95159737214305));
#50876=CARTESIAN_POINT('Ctrl Pts',(-2.73688288329825,-1.,2.94823023414381));
#50877=CARTESIAN_POINT('Ctrl Pts',(-2.73688288329825,1.,2.94823023414381));
#50878=CARTESIAN_POINT('Ctrl Pts',(-2.73003657371613,-1.,2.94482887675139));
#50879=CARTESIAN_POINT('Ctrl Pts',(-2.73003657371613,1.,2.94482887675139));
#50880=CARTESIAN_POINT('Ctrl Pts',(-2.72321571511322,-1.,2.94139351933882));
#50881=CARTESIAN_POINT('Ctrl Pts',(-2.72321571511322,1.,2.94139351933882));
#50882=CARTESIAN_POINT('Ctrl Pts',(-2.71642190053575,-1.,2.93792519474955));
#50883=CARTESIAN_POINT('Ctrl Pts',(-2.71642190053575,1.,2.93792519474955));
#50884=CARTESIAN_POINT('Ctrl Pts',(-2.70965695523776,-1.,2.93442516311168));
#50885=CARTESIAN_POINT('Ctrl Pts',(-2.70965695523776,1.,2.93442516311168));
#50886=CARTESIAN_POINT('Ctrl Pts',(-2.70292247416881,-1.,2.93089438233746));
#50887=CARTESIAN_POINT('Ctrl Pts',(-2.70292247416881,1.,2.93089438233746));
#50888=CARTESIAN_POINT('Ctrl Pts',(-2.69621932864302,-1.,2.92733294395268));
#50889=CARTESIAN_POINT('Ctrl Pts',(-2.69621932864302,1.,2.92733294395268));
#50890=CARTESIAN_POINT('Ctrl Pts',(-2.68954721165342,-1.,2.92373955325876));
#50891=CARTESIAN_POINT('Ctrl Pts',(-2.68954721165342,1.,2.92373955325876));
#50892=CARTESIAN_POINT('Ctrl Pts',(-2.68290409279689,-1.,2.92011090722152));
#50893=CARTESIAN_POINT('Ctrl Pts',(-2.68290409279689,1.,2.92011090722152));
#50894=CARTESIAN_POINT('Ctrl Pts',(-2.67628728855309,-1.,2.91644290704281));
#50895=CARTESIAN_POINT('Ctrl Pts',(-2.67628728855309,1.,2.91644290704281));
#50896=CARTESIAN_POINT('Ctrl Pts',(-2.66969458792627,-1.,2.91273193382876));
#50897=CARTESIAN_POINT('Ctrl Pts',(-2.66969458792627,1.,2.91273193382876));
#50898=CARTESIAN_POINT('Ctrl Pts',(-2.66312542616809,-1.,2.90897617968921));
#50899=CARTESIAN_POINT('Ctrl Pts',(-2.66312542616809,1.,2.90897617968921));
#50900=CARTESIAN_POINT('Ctrl Pts',(-2.65658188464287,-1.,2.90517678087467));
#50901=CARTESIAN_POINT('Ctrl Pts',(-2.65658188464287,1.,2.90517678087467));
#50902=CARTESIAN_POINT('Ctrl Pts',(-2.65007017365576,-1.,2.90133950224879));
#50903=CARTESIAN_POINT('Ctrl Pts',(-2.65007017365576,1.,2.90133950224879));
#50904=CARTESIAN_POINT('Ctrl Pts',(-2.64359851684146,-1.,2.89747231723361));
#50905=CARTESIAN_POINT('Ctrl Pts',(-2.64359851684146,1.,2.89747231723361));
#50906=CARTESIAN_POINT('Ctrl Pts',(-2.63717442263944,-1.,2.89358228854557));
#50907=CARTESIAN_POINT('Ctrl Pts',(-2.63717442263944,1.,2.89358228854557));
#50908=CARTESIAN_POINT('Ctrl Pts',(-2.63080195420771,-1.,2.88967244854243));
#50909=CARTESIAN_POINT('Ctrl Pts',(-2.63080195420771,1.,2.88967244854243));
#50910=CARTESIAN_POINT('Ctrl Pts',(-2.62447947640253,-1.,2.88573922195049));
#50911=CARTESIAN_POINT('Ctrl Pts',(-2.62447947640253,1.,2.88573922195049));
#50912=CARTESIAN_POINT('Ctrl Pts',(-2.61819596473087,-1.,2.88176821427502));
#50913=CARTESIAN_POINT('Ctrl Pts',(-2.61819596473087,1.,2.88176821427502));
#50914=CARTESIAN_POINT('Ctrl Pts',(-2.61193507170928,-1.,2.87773881947885));
#50915=CARTESIAN_POINT('Ctrl Pts',(-2.61193507170928,1.,2.87773881947885));
#50916=CARTESIAN_POINT('Ctrl Pts',(-2.6056817788128,-1.,2.87363176656475));
#50917=CARTESIAN_POINT('Ctrl Pts',(-2.6056817788128,1.,2.87363176656475));
#50918=CARTESIAN_POINT('Ctrl Pts',(-2.59942875223202,-1.,2.86943633170712));
#50919=CARTESIAN_POINT('Ctrl Pts',(-2.59942875223202,1.,2.86943633170712));
#50920=CARTESIAN_POINT('Ctrl Pts',(-2.59318160184921,-1.,2.86515629953528));
#50921=CARTESIAN_POINT('Ctrl Pts',(-2.59318160184921,1.,2.86515629953528));
#50922=CARTESIAN_POINT('Ctrl Pts',(-2.5869677064356,-1.,2.86081999003668));
#50923=CARTESIAN_POINT('Ctrl Pts',(-2.5869677064356,1.,2.86081999003668));
#50924=CARTESIAN_POINT('Ctrl Pts',(-2.58082875254407,-1.,2.85647171715147));
#50925=CARTESIAN_POINT('Ctrl Pts',(-2.58082875254407,1.,2.85647171715147));
#50926=CARTESIAN_POINT('Ctrl Pts',(-2.57480482727128,-1.,2.85215360144483));
#50927=CARTESIAN_POINT('Ctrl Pts',(-2.57480482727128,1.,2.85215360144483));
#50928=CARTESIAN_POINT('Ctrl Pts',(-2.56891984251743,-1.,2.84788893329091));
#50929=CARTESIAN_POINT('Ctrl Pts',(-2.56891984251743,1.,2.84788893329091));
#50930=CARTESIAN_POINT('Ctrl Pts',(-2.56316920798489,-1.,2.84366802680211));
#50931=CARTESIAN_POINT('Ctrl Pts',(-2.56316920798489,1.,2.84366802680211));
#50932=CARTESIAN_POINT('Ctrl Pts',(-2.55749952145165,-1.,2.83942515220699));
#50933=CARTESIAN_POINT('Ctrl Pts',(-2.55749952145165,1.,2.83942515220699));
#50934=CARTESIAN_POINT('Ctrl Pts',(-2.55182152806964,-1.,2.83505269592412));
#50935=CARTESIAN_POINT('Ctrl Pts',(-2.55182152806964,1.,2.83505269592412));
#50936=CARTESIAN_POINT('Ctrl Pts',(-2.54604736792542,-1.,2.83044254225794));
#50937=CARTESIAN_POINT('Ctrl Pts',(-2.54604736792542,1.,2.83044254225794));
#50938=CARTESIAN_POINT('Ctrl Pts',(-2.54012272520141,-1.,2.82552167649157));
#50939=CARTESIAN_POINT('Ctrl Pts',(-2.54012272520141,1.,2.82552167649157));
#50940=CARTESIAN_POINT('Ctrl Pts',(-2.53405679667463,-1.,2.82028550483744));
#50941=CARTESIAN_POINT('Ctrl Pts',(-2.53405679667463,1.,2.82028550483744));
#50942=CARTESIAN_POINT('Ctrl Pts',(-2.52796388055457,-1.,2.8148437904867));
#50943=CARTESIAN_POINT('Ctrl Pts',(-2.52796388055457,1.,2.8148437904867));
#50944=CARTESIAN_POINT('Ctrl Pts',(-2.52205778589922,-1.,2.80941521967234));
#50945=CARTESIAN_POINT('Ctrl Pts',(-2.52205778589922,1.,2.80941521967234));
#50946=CARTESIAN_POINT('Ctrl Pts',(-2.51660190466067,-1.,2.80427363984939));
#50947=CARTESIAN_POINT('Ctrl Pts',(-2.51660190466067,1.,2.80427363984939));
#50948=CARTESIAN_POINT('Ctrl Pts',(-2.51186983687947,-1.,2.79970585014308));
#50949=CARTESIAN_POINT('Ctrl Pts',(-2.51186983687947,1.,2.79970585014308));
#50950=CARTESIAN_POINT('Ctrl Pts',(-2.50810555977564,-1.,2.7959687805717));
#50951=CARTESIAN_POINT('Ctrl Pts',(-2.50810555977564,1.,2.7959687805717));
#50952=CARTESIAN_POINT('Ctrl Pts',(-2.50547439929077,-1.,2.79323694088143));
#50953=CARTESIAN_POINT('Ctrl Pts',(-2.50547439929077,1.,2.79323694088143));
#50954=CARTESIAN_POINT('Ctrl Pts',(-2.50433799076945,-1.,2.79192122906739));
#50955=CARTESIAN_POINT('Ctrl Pts',(-2.50433799076945,1.,2.79192122906739));
#50956=CARTESIAN_POINT('Ctrl Pts',(-2.50404230339032,-1.,2.79143626022225));
#50957=CARTESIAN_POINT('Ctrl Pts',(-2.50404230339032,1.,2.79143626022225));
#50958=CARTESIAN_POINT('Ctrl Pts',(-2.50409239460011,-1.,2.79133581100044));
#50959=CARTESIAN_POINT('Ctrl Pts',(-2.50409239460011,1.,2.79133581100044));
#50960=CARTESIAN_POINT('Ctrl Pts',(-2.50417924854921,-1.,2.79134130681569));
#50961=CARTESIAN_POINT('Ctrl Pts',(-2.50417924854921,1.,2.79134130681569));
#50962=CARTESIAN_POINT('',(-2.91557726271063,1.,3.02314558451372));
#50963=CARTESIAN_POINT('Ctrl Pts',(-2.91557726271063,1.,3.02314558451372));
#50964=CARTESIAN_POINT('Ctrl Pts',(-2.91409518070707,1.,3.02261975104912));
#50965=CARTESIAN_POINT('Ctrl Pts',(-2.91113297349052,1.,3.02156522743299));
#50966=CARTESIAN_POINT('Ctrl Pts',(-2.90669553303902,1.,3.01997487194926));
#50967=CARTESIAN_POINT('Ctrl Pts',(-2.90079069102661,1.,3.01783725123646));
#50968=CARTESIAN_POINT('Ctrl Pts',(-2.8934292556764,1.,3.01513660433291));
#50969=CARTESIAN_POINT('Ctrl Pts',(-2.88608751706796,1.,3.01240727309568));
#50970=CARTESIAN_POINT('Ctrl Pts',(-2.87876560072799,1.,3.0096491810855));
#50971=CARTESIAN_POINT('Ctrl Pts',(-2.87146368430104,1.,3.00686224485374));
#50972=CARTESIAN_POINT('Ctrl Pts',(-2.86418200833065,1.,3.00404638316245));
#50973=CARTESIAN_POINT('Ctrl Pts',(-2.85692085715129,1.,3.0012015079552));
#50974=CARTESIAN_POINT('Ctrl Pts',(-2.84968053289104,1.,2.99832751144566));
#50975=CARTESIAN_POINT('Ctrl Pts',(-2.84246132984334,1.,2.995424253416));
#50976=CARTESIAN_POINT('Ctrl Pts',(-2.83526351254383,1.,2.99249155170479));
#50977=CARTESIAN_POINT('Ctrl Pts',(-2.82808728190402,1.,2.98952916401699));
#50978=CARTESIAN_POINT('Ctrl Pts',(-2.82093279065704,1.,2.98653680669434));
#50979=CARTESIAN_POINT('Ctrl Pts',(-2.81380019196454,1.,2.9835141977994));
#50980=CARTESIAN_POINT('Ctrl Pts',(-2.80668968101162,1.,2.98046109647299));
#50981=CARTESIAN_POINT('Ctrl Pts',(-2.79960153278186,1.,2.97737733718242));
#50982=CARTESIAN_POINT('Ctrl Pts',(-2.79253615718147,1.,2.97426288347475));
#50983=CARTESIAN_POINT('Ctrl Pts',(-2.78549409123657,1.,2.97111781461349));
#50984=CARTESIAN_POINT('Ctrl Pts',(-2.77847589542767,1.,2.9679422104295));
#50985=CARTESIAN_POINT('Ctrl Pts',(-2.77148206836464,1.,2.96473605585548));
#50986=CARTESIAN_POINT('Ctrl Pts',(-2.76451296269571,1.,2.96149914764832));
#50987=CARTESIAN_POINT('Ctrl Pts',(-2.75756867888393,1.,2.9582309766594));
#50988=CARTESIAN_POINT('Ctrl Pts',(-2.75064903318996,1.,2.95493069316211));
#50989=CARTESIAN_POINT('Ctrl Pts',(-2.7437537949221,1.,2.95159737214305));
#50990=CARTESIAN_POINT('Ctrl Pts',(-2.73688288329825,1.,2.94823023414381));
#50991=CARTESIAN_POINT('Ctrl Pts',(-2.73003657371613,1.,2.94482887675139));
#50992=CARTESIAN_POINT('Ctrl Pts',(-2.72321571511322,1.,2.94139351933882));
#50993=CARTESIAN_POINT('Ctrl Pts',(-2.71642190053575,1.,2.93792519474955));
#50994=CARTESIAN_POINT('Ctrl Pts',(-2.70965695523776,1.,2.93442516311168));
#50995=CARTESIAN_POINT('Ctrl Pts',(-2.70292247416881,1.,2.93089438233746));
#50996=CARTESIAN_POINT('Ctrl Pts',(-2.69621932864302,1.,2.92733294395268));
#50997=CARTESIAN_POINT('Ctrl Pts',(-2.68954721165342,1.,2.92373955325876));
#50998=CARTESIAN_POINT('Ctrl Pts',(-2.68290409279689,1.,2.92011090722152));
#50999=CARTESIAN_POINT('Ctrl Pts',(-2.67628728855309,1.,2.91644290704281));
#51000=CARTESIAN_POINT('Ctrl Pts',(-2.66969458792627,1.,2.91273193382876));
#51001=CARTESIAN_POINT('Ctrl Pts',(-2.66312542616809,1.,2.90897617968921));
#51002=CARTESIAN_POINT('Ctrl Pts',(-2.65658188464287,1.,2.90517678087467));
#51003=CARTESIAN_POINT('Ctrl Pts',(-2.65007017365576,1.,2.90133950224879));
#51004=CARTESIAN_POINT('Ctrl Pts',(-2.64359851684146,1.,2.89747231723361));
#51005=CARTESIAN_POINT('Ctrl Pts',(-2.63717442263944,1.,2.89358228854557));
#51006=CARTESIAN_POINT('Ctrl Pts',(-2.63080195420771,1.,2.88967244854243));
#51007=CARTESIAN_POINT('Ctrl Pts',(-2.62447947640253,1.,2.88573922195049));
#51008=CARTESIAN_POINT('Ctrl Pts',(-2.61819596473087,1.,2.88176821427502));
#51009=CARTESIAN_POINT('Ctrl Pts',(-2.61193507170928,1.,2.87773881947885));
#51010=CARTESIAN_POINT('Ctrl Pts',(-2.6056817788128,1.,2.87363176656475));
#51011=CARTESIAN_POINT('Ctrl Pts',(-2.59942875223202,1.,2.86943633170712));
#51012=CARTESIAN_POINT('Ctrl Pts',(-2.59318160184921,1.,2.86515629953528));
#51013=CARTESIAN_POINT('Ctrl Pts',(-2.5869677064356,1.,2.86081999003668));
#51014=CARTESIAN_POINT('Ctrl Pts',(-2.58082875254407,1.,2.85647171715147));
#51015=CARTESIAN_POINT('Ctrl Pts',(-2.57480482727128,1.,2.85215360144483));
#51016=CARTESIAN_POINT('Ctrl Pts',(-2.56891984251743,1.,2.84788893329091));
#51017=CARTESIAN_POINT('Ctrl Pts',(-2.56316920798489,1.,2.84366802680211));
#51018=CARTESIAN_POINT('Ctrl Pts',(-2.55749952145165,1.,2.83942515220699));
#51019=CARTESIAN_POINT('Ctrl Pts',(-2.55182152806964,1.,2.83505269592412));
#51020=CARTESIAN_POINT('Ctrl Pts',(-2.54604736792542,1.,2.83044254225794));
#51021=CARTESIAN_POINT('Ctrl Pts',(-2.54012272520141,1.,2.82552167649157));
#51022=CARTESIAN_POINT('Ctrl Pts',(-2.53405679667463,1.,2.82028550483744));
#51023=CARTESIAN_POINT('Ctrl Pts',(-2.52796388055457,1.,2.8148437904867));
#51024=CARTESIAN_POINT('Ctrl Pts',(-2.52205778589922,1.,2.80941521967234));
#51025=CARTESIAN_POINT('Ctrl Pts',(-2.51660190466067,1.,2.80427363984939));
#51026=CARTESIAN_POINT('Ctrl Pts',(-2.51186983687947,1.,2.79970585014308));
#51027=CARTESIAN_POINT('Ctrl Pts',(-2.50810555977564,1.,2.7959687805717));
#51028=CARTESIAN_POINT('Ctrl Pts',(-2.50567182569153,1.,2.79344192164204));
#51029=CARTESIAN_POINT('Ctrl Pts',(-2.50455968395235,1.,2.79217568804874));
#51030=CARTESIAN_POINT('Ctrl Pts',(-2.50417932839343,1.,2.79164172519039));
#51031=CARTESIAN_POINT('Ctrl Pts',(-2.50410700351427,1.,2.79145823440899));
#51032=CARTESIAN_POINT('Ctrl Pts',(-2.50410331873043,1.,2.79140942341378));
#51033=CARTESIAN_POINT('',(-2.91557726271063,0.,3.02314558451372));
#51034=CARTESIAN_POINT('Ctrl Pts',(-2.79134130681569,-1.,2.50417924854921));
#51035=CARTESIAN_POINT('Ctrl Pts',(-2.79134130681569,1.,2.50417924854921));
#51036=CARTESIAN_POINT('Ctrl Pts',(-2.7913358110015,-1.,2.50409239460108));
#51037=CARTESIAN_POINT('Ctrl Pts',(-2.7913358110015,1.,2.50409239460108));
#51038=CARTESIAN_POINT('Ctrl Pts',(-2.79143626022503,-1.,2.50404230339286));
#51039=CARTESIAN_POINT('Ctrl Pts',(-2.79143626022503,1.,2.50404230339286));
#51040=CARTESIAN_POINT('Ctrl Pts',(-2.79192122907148,-1.,2.5043379907732));
#51041=CARTESIAN_POINT('Ctrl Pts',(-2.79192122907148,1.,2.5043379907732));
#51042=CARTESIAN_POINT('Ctrl Pts',(-2.7932369408851,-1.,2.50547439929414));
#51043=CARTESIAN_POINT('Ctrl Pts',(-2.7932369408851,1.,2.50547439929414));
#51044=CARTESIAN_POINT('Ctrl Pts',(-2.79596878057287,-1.,2.50810555977671));
#51045=CARTESIAN_POINT('Ctrl Pts',(-2.79596878057287,1.,2.50810555977671));
#51046=CARTESIAN_POINT('Ctrl Pts',(-2.79970585014168,-1.,2.51186983687818));
#51047=CARTESIAN_POINT('Ctrl Pts',(-2.79970585014168,1.,2.51186983687818));
#51048=CARTESIAN_POINT('Ctrl Pts',(-2.80427363984653,-1.,2.51660190465805));
#51049=CARTESIAN_POINT('Ctrl Pts',(-2.80427363984653,1.,2.51660190465805));
#51050=CARTESIAN_POINT('Ctrl Pts',(-2.80941521966941,-1.,2.52205778589653));
#51051=CARTESIAN_POINT('Ctrl Pts',(-2.80941521966941,1.,2.52205778589653));
#51052=CARTESIAN_POINT('Ctrl Pts',(-2.81484379048475,-1.,2.52796388055278));
#51053=CARTESIAN_POINT('Ctrl Pts',(-2.81484379048475,1.,2.52796388055278));
#51054=CARTESIAN_POINT('Ctrl Pts',(-2.82028550483689,-1.,2.53405679667412));
#51055=CARTESIAN_POINT('Ctrl Pts',(-2.82028550483689,1.,2.53405679667412));
#51056=CARTESIAN_POINT('Ctrl Pts',(-2.8255216764922,-1.,2.54012272520199));
#51057=CARTESIAN_POINT('Ctrl Pts',(-2.8255216764922,1.,2.54012272520199));
#51058=CARTESIAN_POINT('Ctrl Pts',(-2.83044254225917,-1.,2.54604736792655));
#51059=CARTESIAN_POINT('Ctrl Pts',(-2.83044254225917,1.,2.54604736792655));
#51060=CARTESIAN_POINT('Ctrl Pts',(-2.83505269592536,-1.,2.55182152807077));
#51061=CARTESIAN_POINT('Ctrl Pts',(-2.83505269592536,1.,2.55182152807077));
#51062=CARTESIAN_POINT('Ctrl Pts',(-2.83942515220782,-1.,2.55749952145241));
#51063=CARTESIAN_POINT('Ctrl Pts',(-2.83942515220782,1.,2.55749952145241));
#51064=CARTESIAN_POINT('Ctrl Pts',(-2.84366802680237,-1.,2.56316920798513));
#51065=CARTESIAN_POINT('Ctrl Pts',(-2.84366802680237,1.,2.56316920798513));
#51066=CARTESIAN_POINT('Ctrl Pts',(-2.84788893329067,-1.,2.56891984251721));
#51067=CARTESIAN_POINT('Ctrl Pts',(-2.84788893329067,1.,2.56891984251721));
#51068=CARTESIAN_POINT('Ctrl Pts',(-2.85215360144431,-1.,2.57480482727081));
#51069=CARTESIAN_POINT('Ctrl Pts',(-2.85215360144431,1.,2.57480482727081));
#51070=CARTESIAN_POINT('Ctrl Pts',(-2.85647171715092,-1.,2.58082875254357));
#51071=CARTESIAN_POINT('Ctrl Pts',(-2.85647171715092,1.,2.58082875254357));
#51072=CARTESIAN_POINT('Ctrl Pts',(-2.86081999003629,-1.,2.58696770643524));
#51073=CARTESIAN_POINT('Ctrl Pts',(-2.86081999003629,1.,2.58696770643524));
#51074=CARTESIAN_POINT('Ctrl Pts',(-2.86515629953513,-1.,2.59318160184908));
#51075=CARTESIAN_POINT('Ctrl Pts',(-2.86515629953513,1.,2.59318160184908));
#51076=CARTESIAN_POINT('Ctrl Pts',(-2.86943633170722,-1.,2.5994287522321));
#51077=CARTESIAN_POINT('Ctrl Pts',(-2.86943633170722,1.,2.5994287522321));
#51078=CARTESIAN_POINT('Ctrl Pts',(-2.87363176656501,-1.,2.60568177881303));
#51079=CARTESIAN_POINT('Ctrl Pts',(-2.87363176656501,1.,2.60568177881303));
#51080=CARTESIAN_POINT('Ctrl Pts',(-2.87773881947916,-1.,2.61193507170955));
#51081=CARTESIAN_POINT('Ctrl Pts',(-2.87773881947916,1.,2.61193507170955));
#51082=CARTESIAN_POINT('Ctrl Pts',(-2.88176821427525,-1.,2.61819596473108));
#51083=CARTESIAN_POINT('Ctrl Pts',(-2.88176821427525,1.,2.61819596473108));
#51084=CARTESIAN_POINT('Ctrl Pts',(-2.88573922195059,-1.,2.62447947640262));
#51085=CARTESIAN_POINT('Ctrl Pts',(-2.88573922195059,1.,2.62447947640262));
#51086=CARTESIAN_POINT('Ctrl Pts',(-2.88967244854239,-1.,2.63080195420767));
#51087=CARTESIAN_POINT('Ctrl Pts',(-2.88967244854239,1.,2.63080195420767));
#51088=CARTESIAN_POINT('Ctrl Pts',(-2.89358228854544,-1.,2.63717442263932));
#51089=CARTESIAN_POINT('Ctrl Pts',(-2.89358228854544,1.,2.63717442263932));
#51090=CARTESIAN_POINT('Ctrl Pts',(-2.89747231723345,-1.,2.64359851684131));
#51091=CARTESIAN_POINT('Ctrl Pts',(-2.89747231723345,1.,2.64359851684131));
#51092=CARTESIAN_POINT('Ctrl Pts',(-2.90133950224867,-1.,2.65007017365564));
#51093=CARTESIAN_POINT('Ctrl Pts',(-2.90133950224867,1.,2.65007017365564));
#51094=CARTESIAN_POINT('Ctrl Pts',(-2.90517678087461,-1.,2.65658188464282));
#51095=CARTESIAN_POINT('Ctrl Pts',(-2.90517678087461,1.,2.65658188464282));
#51096=CARTESIAN_POINT('Ctrl Pts',(-2.90897617968923,-1.,2.6631254261681));
#51097=CARTESIAN_POINT('Ctrl Pts',(-2.90897617968923,1.,2.6631254261681));
#51098=CARTESIAN_POINT('Ctrl Pts',(-2.91273193382882,-1.,2.66969458792631));
#51099=CARTESIAN_POINT('Ctrl Pts',(-2.91273193382882,1.,2.66969458792631));
#51100=CARTESIAN_POINT('Ctrl Pts',(-2.91644290704285,-1.,2.67628728855312));
#51101=CARTESIAN_POINT('Ctrl Pts',(-2.91644290704285,1.,2.67628728855312));
#51102=CARTESIAN_POINT('Ctrl Pts',(-2.92011090722152,-1.,2.68290409279688));
#51103=CARTESIAN_POINT('Ctrl Pts',(-2.92011090722152,1.,2.68290409279688));
#51104=CARTESIAN_POINT('Ctrl Pts',(-2.92373955325875,-1.,2.68954721165339));
#51105=CARTESIAN_POINT('Ctrl Pts',(-2.92373955325875,1.,2.68954721165339));
#51106=CARTESIAN_POINT('Ctrl Pts',(-2.92733294395267,-1.,2.69621932864301));
#51107=CARTESIAN_POINT('Ctrl Pts',(-2.92733294395267,1.,2.69621932864301));
#51108=CARTESIAN_POINT('Ctrl Pts',(-2.9308943823375,-1.,2.70292247416885));
#51109=CARTESIAN_POINT('Ctrl Pts',(-2.9308943823375,1.,2.70292247416885));
#51110=CARTESIAN_POINT('Ctrl Pts',(-2.93442516311179,-1.,2.70965695523787));
#51111=CARTESIAN_POINT('Ctrl Pts',(-2.93442516311179,1.,2.70965695523787));
#51112=CARTESIAN_POINT('Ctrl Pts',(-2.93792519474972,-1.,2.71642190053592));
#51113=CARTESIAN_POINT('Ctrl Pts',(-2.93792519474972,1.,2.71642190053592));
#51114=CARTESIAN_POINT('Ctrl Pts',(-2.94139351933897,-1.,2.72321571511337));
#51115=CARTESIAN_POINT('Ctrl Pts',(-2.94139351933897,1.,2.72321571511337));
#51116=CARTESIAN_POINT('Ctrl Pts',(-2.94482887675143,-1.,2.73003657371617));
#51117=CARTESIAN_POINT('Ctrl Pts',(-2.94482887675143,1.,2.73003657371617));
#51118=CARTESIAN_POINT('Ctrl Pts',(-2.94823023414364,-1.,2.73688288329808));
#51119=CARTESIAN_POINT('Ctrl Pts',(-2.94823023414364,1.,2.73688288329808));
#51120=CARTESIAN_POINT('Ctrl Pts',(-2.95159737214266,-1.,2.74375379492172));
#51121=CARTESIAN_POINT('Ctrl Pts',(-2.95159737214266,1.,2.74375379492172));
#51122=CARTESIAN_POINT('Ctrl Pts',(-2.95493069316161,-1.,2.75064903318947));
#51123=CARTESIAN_POINT('Ctrl Pts',(-2.95493069316161,1.,2.75064903318947));
#51124=CARTESIAN_POINT('Ctrl Pts',(-2.95823097665896,-1.,2.7575686788835));
#51125=CARTESIAN_POINT('Ctrl Pts',(-2.95823097665896,1.,2.7575686788835));
#51126=CARTESIAN_POINT('Ctrl Pts',(-2.96149914764818,-1.,2.76451296269557));
#51127=CARTESIAN_POINT('Ctrl Pts',(-2.96149914764818,1.,2.76451296269557));
#51128=CARTESIAN_POINT('Ctrl Pts',(-2.96473605585583,-1.,2.77148206836498));
#51129=CARTESIAN_POINT('Ctrl Pts',(-2.96473605585583,1.,2.77148206836498));
#51130=CARTESIAN_POINT('Ctrl Pts',(-2.96794221043036,-1.,2.7784758954285));
#51131=CARTESIAN_POINT('Ctrl Pts',(-2.96794221043036,1.,2.7784758954285));
#51132=CARTESIAN_POINT('Ctrl Pts',(-2.97111781461465,-1.,2.78549409123769));
#51133=CARTESIAN_POINT('Ctrl Pts',(-2.97111781461465,1.,2.78549409123769));
#51134=CARTESIAN_POINT('Ctrl Pts',(-2.9742628834758,-1.,2.79253615718248));
#51135=CARTESIAN_POINT('Ctrl Pts',(-2.9742628834758,1.,2.79253615718248));
#51136=CARTESIAN_POINT('Ctrl Pts',(-2.97737733718287,-1.,2.7996015327823));
#51137=CARTESIAN_POINT('Ctrl Pts',(-2.97737733718287,1.,2.7996015327823));
#51138=CARTESIAN_POINT('Ctrl Pts',(-2.98046109647241,-1.,2.80668968101106));
#51139=CARTESIAN_POINT('Ctrl Pts',(-2.98046109647241,1.,2.80668968101106));
#51140=CARTESIAN_POINT('Ctrl Pts',(-2.98351419779767,-1.,2.81380019196286));
#51141=CARTESIAN_POINT('Ctrl Pts',(-2.98351419779767,1.,2.81380019196286));
#51142=CARTESIAN_POINT('Ctrl Pts',(-2.9865368066918,-1.,2.82093279065457));
#51143=CARTESIAN_POINT('Ctrl Pts',(-2.9865368066918,1.,2.82093279065457));
#51144=CARTESIAN_POINT('Ctrl Pts',(-2.98952916401446,-1.,2.82808728190157));
#51145=CARTESIAN_POINT('Ctrl Pts',(-2.98952916401446,1.,2.82808728190157));
#51146=CARTESIAN_POINT('Ctrl Pts',(-2.9924915517034,-1.,2.83526351254248));
#51147=CARTESIAN_POINT('Ctrl Pts',(-2.9924915517034,1.,2.83526351254248));
#51148=CARTESIAN_POINT('Ctrl Pts',(-2.99542425341685,-1.,2.84246132984415));
#51149=CARTESIAN_POINT('Ctrl Pts',(-2.99542425341685,1.,2.84246132984415));
#51150=CARTESIAN_POINT('Ctrl Pts',(-2.99832751144925,-1.,2.84968053289451));
#51151=CARTESIAN_POINT('Ctrl Pts',(-2.99832751144925,1.,2.84968053289451));
#51152=CARTESIAN_POINT('Ctrl Pts',(-3.00120150796095,-1.,2.85692085715686));
#51153=CARTESIAN_POINT('Ctrl Pts',(-3.00120150796095,1.,2.85692085715686));
#51154=CARTESIAN_POINT('Ctrl Pts',(-3.00404638316867,-1.,2.86418200833667));
#51155=CARTESIAN_POINT('Ctrl Pts',(-3.00404638316867,1.,2.86418200833667));
#51156=CARTESIAN_POINT('Ctrl Pts',(-3.00686224485784,-1.,2.87146368430502));
#51157=CARTESIAN_POINT('Ctrl Pts',(-3.00686224485784,1.,2.87146368430502));
#51158=CARTESIAN_POINT('Ctrl Pts',(-3.00964918108476,-1.,2.87876560072727));
#51159=CARTESIAN_POINT('Ctrl Pts',(-3.00964918108476,1.,2.87876560072727));
#51160=CARTESIAN_POINT('Ctrl Pts',(-3.01240727308829,-1.,2.8860875170608));
#51161=CARTESIAN_POINT('Ctrl Pts',(-3.01240727308829,1.,2.8860875170608));
#51162=CARTESIAN_POINT('Ctrl Pts',(-3.01513660431928,-1.,2.89342925566321));
#51163=CARTESIAN_POINT('Ctrl Pts',(-3.01513660431928,1.,2.89342925566321));
#51164=CARTESIAN_POINT('Ctrl Pts',(-3.01783725121981,-1.,2.9007906910105));
#51165=CARTESIAN_POINT('Ctrl Pts',(-3.01783725121981,1.,2.9007906910105));
#51166=CARTESIAN_POINT('Ctrl Pts',(-3.01997487193503,-1.,2.90669553302526));
#51167=CARTESIAN_POINT('Ctrl Pts',(-3.01997487193503,1.,2.90669553302526));
#51168=CARTESIAN_POINT('Ctrl Pts',(-3.02156522742431,-1.,2.91113297348212));
#51169=CARTESIAN_POINT('Ctrl Pts',(-3.02156522742431,1.,2.91113297348212));
#51170=CARTESIAN_POINT('Ctrl Pts',(-3.02261975104593,-1.,2.91409518070399));
#51171=CARTESIAN_POINT('Ctrl Pts',(-3.02261975104593,1.,2.91409518070399));
#51172=CARTESIAN_POINT('Ctrl Pts',(-3.02314558451372,-1.,2.91557726271063));
#51173=CARTESIAN_POINT('Ctrl Pts',(-3.02314558451372,1.,2.91557726271063));
#51174=CARTESIAN_POINT('',(-2.79140942341258,1.,2.50410331873176));
#51175=CARTESIAN_POINT('Ctrl Pts',(-2.79140942341258,-1.,2.50410331873176));
#51176=CARTESIAN_POINT('Ctrl Pts',(-2.79140942341258,-0.666666666666667,
2.50410331873176));
#51177=CARTESIAN_POINT('Ctrl Pts',(-2.79140942341258,-0.333333333333333,
2.50410331873176));
#51178=CARTESIAN_POINT('Ctrl Pts',(-2.79140942341258,0.333333333333333,
2.50410331873176));
#51179=CARTESIAN_POINT('Ctrl Pts',(-2.79140942341258,0.666666666666667,
2.50410331873176));
#51180=CARTESIAN_POINT('Ctrl Pts',(-2.79140942341258,1.,2.50410331873176));
#51181=CARTESIAN_POINT('',(-3.02314558451372,1.,2.91557726271063));
#51182=CARTESIAN_POINT('',(-3.02314558451372,0.,2.91557726271063));
#51183=CARTESIAN_POINT('Ctrl Pts',(-2.79140942341258,1.,2.50410331873176));
#51184=CARTESIAN_POINT('Ctrl Pts',(-2.79145823440781,1.,2.50410700351493));
#51185=CARTESIAN_POINT('Ctrl Pts',(-2.79164172518905,1.,2.50417932839313));
#51186=CARTESIAN_POINT('Ctrl Pts',(-2.79217568804755,1.,2.50455968395146));
#51187=CARTESIAN_POINT('Ctrl Pts',(-2.79344192164147,1.,2.50567182569081));
#51188=CARTESIAN_POINT('Ctrl Pts',(-2.79596878057287,1.,2.50810555977671));
#51189=CARTESIAN_POINT('Ctrl Pts',(-2.79970585014168,1.,2.51186983687818));
#51190=CARTESIAN_POINT('Ctrl Pts',(-2.80427363984653,1.,2.51660190465805));
#51191=CARTESIAN_POINT('Ctrl Pts',(-2.80941521966941,1.,2.52205778589653));
#51192=CARTESIAN_POINT('Ctrl Pts',(-2.81484379048475,1.,2.52796388055278));
#51193=CARTESIAN_POINT('Ctrl Pts',(-2.82028550483689,1.,2.53405679667412));
#51194=CARTESIAN_POINT('Ctrl Pts',(-2.8255216764922,1.,2.54012272520199));
#51195=CARTESIAN_POINT('Ctrl Pts',(-2.83044254225917,1.,2.54604736792655));
#51196=CARTESIAN_POINT('Ctrl Pts',(-2.83505269592536,1.,2.55182152807077));
#51197=CARTESIAN_POINT('Ctrl Pts',(-2.83942515220782,1.,2.55749952145241));
#51198=CARTESIAN_POINT('Ctrl Pts',(-2.84366802680237,1.,2.56316920798513));
#51199=CARTESIAN_POINT('Ctrl Pts',(-2.84788893329067,1.,2.56891984251721));
#51200=CARTESIAN_POINT('Ctrl Pts',(-2.85215360144431,1.,2.57480482727081));
#51201=CARTESIAN_POINT('Ctrl Pts',(-2.85647171715092,1.,2.58082875254357));
#51202=CARTESIAN_POINT('Ctrl Pts',(-2.86081999003629,1.,2.58696770643524));
#51203=CARTESIAN_POINT('Ctrl Pts',(-2.86515629953513,1.,2.59318160184908));
#51204=CARTESIAN_POINT('Ctrl Pts',(-2.86943633170722,1.,2.5994287522321));
#51205=CARTESIAN_POINT('Ctrl Pts',(-2.87363176656501,1.,2.60568177881303));
#51206=CARTESIAN_POINT('Ctrl Pts',(-2.87773881947916,1.,2.61193507170955));
#51207=CARTESIAN_POINT('Ctrl Pts',(-2.88176821427525,1.,2.61819596473108));
#51208=CARTESIAN_POINT('Ctrl Pts',(-2.88573922195059,1.,2.62447947640262));
#51209=CARTESIAN_POINT('Ctrl Pts',(-2.88967244854239,1.,2.63080195420767));
#51210=CARTESIAN_POINT('Ctrl Pts',(-2.89358228854544,1.,2.63717442263932));
#51211=CARTESIAN_POINT('Ctrl Pts',(-2.89747231723345,1.,2.64359851684131));
#51212=CARTESIAN_POINT('Ctrl Pts',(-2.90133950224867,1.,2.65007017365564));
#51213=CARTESIAN_POINT('Ctrl Pts',(-2.90517678087461,1.,2.65658188464282));
#51214=CARTESIAN_POINT('Ctrl Pts',(-2.90897617968923,1.,2.6631254261681));
#51215=CARTESIAN_POINT('Ctrl Pts',(-2.91273193382882,1.,2.66969458792631));
#51216=CARTESIAN_POINT('Ctrl Pts',(-2.91644290704285,1.,2.67628728855312));
#51217=CARTESIAN_POINT('Ctrl Pts',(-2.92011090722152,1.,2.68290409279688));
#51218=CARTESIAN_POINT('Ctrl Pts',(-2.92373955325875,1.,2.68954721165339));
#51219=CARTESIAN_POINT('Ctrl Pts',(-2.92733294395267,1.,2.69621932864301));
#51220=CARTESIAN_POINT('Ctrl Pts',(-2.9308943823375,1.,2.70292247416885));
#51221=CARTESIAN_POINT('Ctrl Pts',(-2.93442516311179,1.,2.70965695523787));
#51222=CARTESIAN_POINT('Ctrl Pts',(-2.93792519474972,1.,2.71642190053592));
#51223=CARTESIAN_POINT('Ctrl Pts',(-2.94139351933897,1.,2.72321571511337));
#51224=CARTESIAN_POINT('Ctrl Pts',(-2.94482887675143,1.,2.73003657371617));
#51225=CARTESIAN_POINT('Ctrl Pts',(-2.94823023414364,1.,2.73688288329808));
#51226=CARTESIAN_POINT('Ctrl Pts',(-2.95159737214266,1.,2.74375379492172));
#51227=CARTESIAN_POINT('Ctrl Pts',(-2.95493069316161,1.,2.75064903318947));
#51228=CARTESIAN_POINT('Ctrl Pts',(-2.95823097665896,1.,2.7575686788835));
#51229=CARTESIAN_POINT('Ctrl Pts',(-2.96149914764818,1.,2.76451296269557));
#51230=CARTESIAN_POINT('Ctrl Pts',(-2.96473605585583,1.,2.77148206836498));
#51231=CARTESIAN_POINT('Ctrl Pts',(-2.96794221043036,1.,2.7784758954285));
#51232=CARTESIAN_POINT('Ctrl Pts',(-2.97111781461465,1.,2.78549409123769));
#51233=CARTESIAN_POINT('Ctrl Pts',(-2.9742628834758,1.,2.79253615718248));
#51234=CARTESIAN_POINT('Ctrl Pts',(-2.97737733718287,1.,2.7996015327823));
#51235=CARTESIAN_POINT('Ctrl Pts',(-2.98046109647241,1.,2.80668968101106));
#51236=CARTESIAN_POINT('Ctrl Pts',(-2.98351419779767,1.,2.81380019196286));
#51237=CARTESIAN_POINT('Ctrl Pts',(-2.9865368066918,1.,2.82093279065457));
#51238=CARTESIAN_POINT('Ctrl Pts',(-2.98952916401446,1.,2.82808728190157));
#51239=CARTESIAN_POINT('Ctrl Pts',(-2.9924915517034,1.,2.83526351254248));
#51240=CARTESIAN_POINT('Ctrl Pts',(-2.99542425341685,1.,2.84246132984415));
#51241=CARTESIAN_POINT('Ctrl Pts',(-2.99832751144925,1.,2.84968053289451));
#51242=CARTESIAN_POINT('Ctrl Pts',(-3.00120150796095,1.,2.85692085715686));
#51243=CARTESIAN_POINT('Ctrl Pts',(-3.00404638316867,1.,2.86418200833667));
#51244=CARTESIAN_POINT('Ctrl Pts',(-3.00686224485784,1.,2.87146368430502));
#51245=CARTESIAN_POINT('Ctrl Pts',(-3.00964918108476,1.,2.87876560072727));
#51246=CARTESIAN_POINT('Ctrl Pts',(-3.01240727308829,1.,2.8860875170608));
#51247=CARTESIAN_POINT('Ctrl Pts',(-3.01513660431928,1.,2.89342925566321));
#51248=CARTESIAN_POINT('Ctrl Pts',(-3.01783725121981,1.,2.9007906910105));
#51249=CARTESIAN_POINT('Ctrl Pts',(-3.01997487193503,1.,2.90669553302526));
#51250=CARTESIAN_POINT('Ctrl Pts',(-3.02156522742431,1.,2.91113297348212));
#51251=CARTESIAN_POINT('Ctrl Pts',(-3.02261975104593,1.,2.91409518070399));
#51252=CARTESIAN_POINT('Ctrl Pts',(-3.02314558451372,1.,2.91557726271063));
#51253=CARTESIAN_POINT('Origin',(-3.02314558451372,0.,2.91557726271063));
#51254=CARTESIAN_POINT('',(-2.91557726271063,1.,3.02314558451372));
#51255=CARTESIAN_POINT('Origin',(0.,0.,0.));
#51256=CARTESIAN_POINT('',(-2.90994629141562,1.,2.36531447826213));
#51257=CARTESIAN_POINT('Origin',(0.,1.,0.));
#51258=CARTESIAN_POINT('Ctrl Pts',(-2.90994629141562,1.,2.36531447826213));
#51259=CARTESIAN_POINT('Ctrl Pts',(-2.90994629141562,0.666666666666667,
2.36531447826213));
#51260=CARTESIAN_POINT('Ctrl Pts',(-2.90994629141562,0.333333333333333,
2.36531447826213));
#51261=CARTESIAN_POINT('Ctrl Pts',(-2.90994629141562,-0.333333333333333,
2.36531447826213));
#51262=CARTESIAN_POINT('Ctrl Pts',(-2.90994629141562,-0.666666666666667,
2.36531447826213));
#51263=CARTESIAN_POINT('Ctrl Pts',(-2.90994629141562,-1.,2.36531447826213));
#51264=CARTESIAN_POINT('Ctrl Pts',(-3.35260583073571,-1.,2.52982887637028));
#51265=CARTESIAN_POINT('Ctrl Pts',(-3.35260583073571,1.,2.52982887637028));
#51266=CARTESIAN_POINT('Ctrl Pts',(-3.35105973714426,-1.,2.52954136549357));
#51267=CARTESIAN_POINT('Ctrl Pts',(-3.35105973714426,1.,2.52954136549357));
#51268=CARTESIAN_POINT('Ctrl Pts',(-3.34796903577628,-1.,2.5289632161143));
#51269=CARTESIAN_POINT('Ctrl Pts',(-3.34796903577628,1.,2.5289632161143));
#51270=CARTESIAN_POINT('Ctrl Pts',(-3.34333744117093,-1.,2.52808660916879));
#51271=CARTESIAN_POINT('Ctrl Pts',(-3.34333744117093,1.,2.52808660916879));
#51272=CARTESIAN_POINT('Ctrl Pts',(-3.33717090000955,-1.,2.52689902691551));
#51273=CARTESIAN_POINT('Ctrl Pts',(-3.33717090000955,1.,2.52689902691551));
#51274=CARTESIAN_POINT('Ctrl Pts',(-3.32947762189049,-1.,2.52538321165774));
#51275=CARTESIAN_POINT('Ctrl Pts',(-3.32947762189049,1.,2.52538321165774));
#51276=CARTESIAN_POINT('Ctrl Pts',(-3.32179931079521,-1.,2.52383598396878));
#51277=CARTESIAN_POINT('Ctrl Pts',(-3.32179931079521,1.,2.52383598396878));
#51278=CARTESIAN_POINT('Ctrl Pts',(-3.31413607874727,-1.,2.52225724871375));
#51279=CARTESIAN_POINT('Ctrl Pts',(-3.31413607874727,1.,2.52225724871375));
#51280=CARTESIAN_POINT('Ctrl Pts',(-3.30648808814986,-1.,2.52064689568167));
#51281=CARTESIAN_POINT('Ctrl Pts',(-3.30648808814986,1.,2.52064689568167));
#51282=CARTESIAN_POINT('Ctrl Pts',(-3.29885556387661,-1.,2.51900480700548));
#51283=CARTESIAN_POINT('Ctrl Pts',(-3.29885556387661,1.,2.51900480700548));
#51284=CARTESIAN_POINT('Ctrl Pts',(-3.2912387729863,-1.,2.51733085123316));
#51285=CARTESIAN_POINT('Ctrl Pts',(-3.2912387729863,1.,2.51733085123316));
#51286=CARTESIAN_POINT('Ctrl Pts',(-3.28363799702583,-1.,2.51562487464215));
#51287=CARTESIAN_POINT('Ctrl Pts',(-3.28363799702583,1.,2.51562487464215));
#51288=CARTESIAN_POINT('Ctrl Pts',(-3.27605350473048,-1.,2.51388669270329));
#51289=CARTESIAN_POINT('Ctrl Pts',(-3.27605350473048,1.,2.51388669270329));
#51290=CARTESIAN_POINT('Ctrl Pts',(-3.26848552888271,-1.,2.51211608411539));
#51291=CARTESIAN_POINT('Ctrl Pts',(-3.26848552888271,1.,2.51211608411539));
#51292=CARTESIAN_POINT('Ctrl Pts',(-3.26093423001716,-1.,2.51031277813697));
#51293=CARTESIAN_POINT('Ctrl Pts',(-3.26093423001716,1.,2.51031277813697));
#51294=CARTESIAN_POINT('Ctrl Pts',(-3.25339971461265,-1.,2.50847647070936));
#51295=CARTESIAN_POINT('Ctrl Pts',(-3.25339971461265,1.,2.50847647070936));
#51296=CARTESIAN_POINT('Ctrl Pts',(-3.24588208984042,-1.,2.50660685940645));
#51297=CARTESIAN_POINT('Ctrl Pts',(-3.24588208984042,1.,2.50660685940645));
#51298=CARTESIAN_POINT('Ctrl Pts',(-3.23838151080383,-1.,2.50470367580078));
#51299=CARTESIAN_POINT('Ctrl Pts',(-3.23838151080383,1.,2.50470367580078));
#51300=CARTESIAN_POINT('Ctrl Pts',(-3.23089822320596,-1.,2.50276671338074));
#51301=CARTESIAN_POINT('Ctrl Pts',(-3.23089822320596,1.,2.50276671338074));
#51302=CARTESIAN_POINT('Ctrl Pts',(-3.22343262620387,-1.,2.5007958720187));
#51303=CARTESIAN_POINT('Ctrl Pts',(-3.22343262620387,1.,2.5007958720187));
#51304=CARTESIAN_POINT('Ctrl Pts',(-3.21598526261157,-1.,2.49879114599293));
#51305=CARTESIAN_POINT('Ctrl Pts',(-3.21598526261157,1.,2.49879114599293));
#51306=CARTESIAN_POINT('Ctrl Pts',(-3.2085566984974,-1.,2.49675252647298));
#51307=CARTESIAN_POINT('Ctrl Pts',(-3.2085566984974,1.,2.49675252647298));
#51308=CARTESIAN_POINT('Ctrl Pts',(-3.20114742397549,-1.,2.49467992057726));
#51309=CARTESIAN_POINT('Ctrl Pts',(-3.20114742397549,1.,2.49467992057726));
#51310=CARTESIAN_POINT('Ctrl Pts',(-3.19375775555814,-1.,2.4925730723986));
#51311=CARTESIAN_POINT('Ctrl Pts',(-3.19375775555814,1.,2.4925730723986));
#51312=CARTESIAN_POINT('Ctrl Pts',(-3.18638771282315,-1.,2.49043146334095));
#51313=CARTESIAN_POINT('Ctrl Pts',(-3.18638771282315,1.,2.49043146334095));
#51314=CARTESIAN_POINT('Ctrl Pts',(-3.17903698136679,-1.,2.48825428288243));
#51315=CARTESIAN_POINT('Ctrl Pts',(-3.17903698136679,1.,2.48825428288243));
#51316=CARTESIAN_POINT('Ctrl Pts',(-3.17170518863357,-1.,2.48604065348619));
#51317=CARTESIAN_POINT('Ctrl Pts',(-3.17170518863357,1.,2.48604065348619));
#51318=CARTESIAN_POINT('Ctrl Pts',(-3.16439213290181,-1.,2.48378981792739));
#51319=CARTESIAN_POINT('Ctrl Pts',(-3.16439213290181,1.,2.48378981792739));
#51320=CARTESIAN_POINT('Ctrl Pts',(-3.15709802322735,-1.,2.48150133566568));
#51321=CARTESIAN_POINT('Ctrl Pts',(-3.15709802322735,1.,2.48150133566568));
#51322=CARTESIAN_POINT('Ctrl Pts',(-3.14982373241335,-1.,2.47917529057016));
#51323=CARTESIAN_POINT('Ctrl Pts',(-3.14982373241335,1.,2.47917529057016));
#51324=CARTESIAN_POINT('Ctrl Pts',(-3.14257099546531,-1.,2.47681245356095));
#51325=CARTESIAN_POINT('Ctrl Pts',(-3.14257099546531,1.,2.47681245356095));
#51326=CARTESIAN_POINT('Ctrl Pts',(-3.13534181229282,-1.,2.47441378371923));
#51327=CARTESIAN_POINT('Ctrl Pts',(-3.13534181229282,1.,2.47441378371923));
#51328=CARTESIAN_POINT('Ctrl Pts',(-3.12813790805948,-1.,2.47197997765868));
#51329=CARTESIAN_POINT('Ctrl Pts',(-3.12813790805948,1.,2.47197997765868));
#51330=CARTESIAN_POINT('Ctrl Pts',(-3.12096015766984,-1.,2.4695109894747));
#51331=CARTESIAN_POINT('Ctrl Pts',(-3.12096015766984,1.,2.4695109894747));
#51332=CARTESIAN_POINT('Ctrl Pts',(-3.11380805536124,-1.,2.46700558843507));
#51333=CARTESIAN_POINT('Ctrl Pts',(-3.11380805536124,1.,2.46700558843507));
#51334=CARTESIAN_POINT('Ctrl Pts',(-3.10667907901981,-1.,2.46446082979645));
#51335=CARTESIAN_POINT('Ctrl Pts',(-3.10667907901981,1.,2.46446082979645));
#51336=CARTESIAN_POINT('Ctrl Pts',(-3.09956993697048,-1.,2.4618730850188));
#51337=CARTESIAN_POINT('Ctrl Pts',(-3.09956993697048,1.,2.4618730850188));
#51338=CARTESIAN_POINT('Ctrl Pts',(-3.09247787931881,-1.,2.45923912563875));
#51339=CARTESIAN_POINT('Ctrl Pts',(-3.09247787931881,1.,2.45923912563875));
#51340=CARTESIAN_POINT('Ctrl Pts',(-3.08540206545313,-1.,2.45655725437037));
#51341=CARTESIAN_POINT('Ctrl Pts',(-3.08540206545313,1.,2.45655725437037));
#51342=CARTESIAN_POINT('Ctrl Pts',(-3.07834472886145,-1.,2.45382826787795));
#51343=CARTESIAN_POINT('Ctrl Pts',(-3.07834472886145,1.,2.45382826787795));
#51344=CARTESIAN_POINT('Ctrl Pts',(-3.0713129052131,-1.,2.45105688854432));
#51345=CARTESIAN_POINT('Ctrl Pts',(-3.0713129052131,1.,2.45105688854432));
#51346=CARTESIAN_POINT('Ctrl Pts',(-3.06431596421422,-1.,2.44824970516558));
#51347=CARTESIAN_POINT('Ctrl Pts',(-3.06431596421422,1.,2.44824970516558));
#51348=CARTESIAN_POINT('Ctrl Pts',(-3.05736242671521,-1.,2.44541251892568));
#51349=CARTESIAN_POINT('Ctrl Pts',(-3.05736242671521,1.,2.44541251892568));
#51350=CARTESIAN_POINT('Ctrl Pts',(-3.05045678021509,-1.,2.44254768923109));
#51351=CARTESIAN_POINT('Ctrl Pts',(-3.05045678021509,1.,2.44254768923109));
#51352=CARTESIAN_POINT('Ctrl Pts',(-3.04359685040545,-1.,2.43965194061849));
#51353=CARTESIAN_POINT('Ctrl Pts',(-3.04359685040545,1.,2.43965194061849));
#51354=CARTESIAN_POINT('Ctrl Pts',(-3.03676949672797,-1.,2.43671278042394));
#51355=CARTESIAN_POINT('Ctrl Pts',(-3.03676949672797,1.,2.43671278042394));
#51356=CARTESIAN_POINT('Ctrl Pts',(-3.02995534946946,-1.,2.43371241361462));
#51357=CARTESIAN_POINT('Ctrl Pts',(-3.02995534946946,1.,2.43371241361462));
#51358=CARTESIAN_POINT('Ctrl Pts',(-3.02313656035977,-1.,2.43063415586615));
#51359=CARTESIAN_POINT('Ctrl Pts',(-3.02313656035977,1.,2.43063415586615));
#51360=CARTESIAN_POINT('Ctrl Pts',(-3.01630420830494,-1.,2.4274685626416));
#51361=CARTESIAN_POINT('Ctrl Pts',(-3.01630420830494,1.,2.4274685626416));
#51362=CARTESIAN_POINT('Ctrl Pts',(-3.00946442616674,-1.,2.42421849439625));
#51363=CARTESIAN_POINT('Ctrl Pts',(-3.00946442616674,1.,2.42421849439625));
#51364=CARTESIAN_POINT('Ctrl Pts',(-3.00264868586038,-1.,2.42090763946812));
#51365=CARTESIAN_POINT('Ctrl Pts',(-3.00264868586038,1.,2.42090763946812));
#51366=CARTESIAN_POINT('Ctrl Pts',(-2.99590509293561,-1.,2.4175732450056));
#51367=CARTESIAN_POINT('Ctrl Pts',(-2.99590509293561,1.,2.4175732450056));
#51368=CARTESIAN_POINT('Ctrl Pts',(-2.98927983005851,-1.,2.4142506419963));
#51369=CARTESIAN_POINT('Ctrl Pts',(-2.98927983005851,1.,2.4142506419963));
#51370=CARTESIAN_POINT('Ctrl Pts',(-2.98280015815132,-1.,2.41095909342591));
#51371=CARTESIAN_POINT('Ctrl Pts',(-2.98280015815132,1.,2.41095909342591));
#51372=CARTESIAN_POINT('Ctrl Pts',(-2.97646002822395,-1.,2.40768975073691));
#51373=CARTESIAN_POINT('Ctrl Pts',(-2.97646002822395,1.,2.40768975073691));
#51374=CARTESIAN_POINT('Ctrl Pts',(-2.97019641312272,-1.,2.40438604734848));
#51375=CARTESIAN_POINT('Ctrl Pts',(-2.97019641312272,1.,2.40438604734848));
#51376=CARTESIAN_POINT('Ctrl Pts',(-2.96390432240181,-1.,2.40095565711535));
#51377=CARTESIAN_POINT('Ctrl Pts',(-2.96390432240181,1.,2.40095565711535));
#51378=CARTESIAN_POINT('Ctrl Pts',(-2.95748006482811,-1.,2.39730553974412));
#51379=CARTESIAN_POINT('Ctrl Pts',(-2.95748006482811,1.,2.39730553974412));
#51380=CARTESIAN_POINT('Ctrl Pts',(-2.95085857128372,-1.,2.39337207631613));
#51381=CARTESIAN_POINT('Ctrl Pts',(-2.95085857128372,1.,2.39337207631613));
#51382=CARTESIAN_POINT('Ctrl Pts',(-2.94404820669135,-1.,2.38914929090806));
#51383=CARTESIAN_POINT('Ctrl Pts',(-2.94404820669135,1.,2.38914929090806));
#51384=CARTESIAN_POINT('Ctrl Pts',(-2.93717903280599,-1.,2.38472771516476));
#51385=CARTESIAN_POINT('Ctrl Pts',(-2.93717903280599,1.,2.38472771516476));
#51386=CARTESIAN_POINT('Ctrl Pts',(-2.93049643640517,-1.,2.3802898958232));
#51387=CARTESIAN_POINT('Ctrl Pts',(-2.93049643640517,1.,2.3802898958232));
#51388=CARTESIAN_POINT('Ctrl Pts',(-2.92430340582912,-1.,2.37606510524271));
#51389=CARTESIAN_POINT('Ctrl Pts',(-2.92430340582912,1.,2.37606510524271));
#51390=CARTESIAN_POINT('Ctrl Pts',(-2.9189150379156,-1.,2.37229381109939));
#51391=CARTESIAN_POINT('Ctrl Pts',(-2.9189150379156,1.,2.37229381109939));
#51392=CARTESIAN_POINT('Ctrl Pts',(-2.91461249883016,-1.,2.36919161373074));
#51393=CARTESIAN_POINT('Ctrl Pts',(-2.91461249883016,1.,2.36919161373074));
#51394=CARTESIAN_POINT('Ctrl Pts',(-2.9115863784165,-1.,2.36690501170317));
#51395=CARTESIAN_POINT('Ctrl Pts',(-2.9115863784165,1.,2.36690501170317));
#51396=CARTESIAN_POINT('Ctrl Pts',(-2.91025813829606,-1.,2.36578327194396));
#51397=CARTESIAN_POINT('Ctrl Pts',(-2.91025813829606,1.,2.36578327194396));
#51398=CARTESIAN_POINT('Ctrl Pts',(-2.90989022547738,-1.,2.36535052956704));
#51399=CARTESIAN_POINT('Ctrl Pts',(-2.90989022547738,1.,2.36535052956704));
#51400=CARTESIAN_POINT('Ctrl Pts',(-2.90992398626098,-1.,2.36524348105023));
#51401=CARTESIAN_POINT('Ctrl Pts',(-2.90992398626098,1.,2.36524348105023));
#51402=CARTESIAN_POINT('Ctrl Pts',(-2.91001063062876,-1.,2.36523532225181));
#51403=CARTESIAN_POINT('Ctrl Pts',(-2.91001063062876,1.,2.36523532225181));
#51404=CARTESIAN_POINT('',(-3.35260583073571,1.,2.52982887637028));
#51405=CARTESIAN_POINT('Ctrl Pts',(-3.35260583073571,1.,2.52982887637028));
#51406=CARTESIAN_POINT('Ctrl Pts',(-3.35105973714426,1.,2.52954136549357));
#51407=CARTESIAN_POINT('Ctrl Pts',(-3.34796903577628,1.,2.5289632161143));
#51408=CARTESIAN_POINT('Ctrl Pts',(-3.34333744117093,1.,2.52808660916879));
#51409=CARTESIAN_POINT('Ctrl Pts',(-3.33717090000955,1.,2.52689902691551));
#51410=CARTESIAN_POINT('Ctrl Pts',(-3.32947762189049,1.,2.52538321165774));
#51411=CARTESIAN_POINT('Ctrl Pts',(-3.32179931079521,1.,2.52383598396878));
#51412=CARTESIAN_POINT('Ctrl Pts',(-3.31413607874727,1.,2.52225724871375));
#51413=CARTESIAN_POINT('Ctrl Pts',(-3.30648808814986,1.,2.52064689568167));
#51414=CARTESIAN_POINT('Ctrl Pts',(-3.29885556387661,1.,2.51900480700548));
#51415=CARTESIAN_POINT('Ctrl Pts',(-3.2912387729863,1.,2.51733085123316));
#51416=CARTESIAN_POINT('Ctrl Pts',(-3.28363799702583,1.,2.51562487464215));
#51417=CARTESIAN_POINT('Ctrl Pts',(-3.27605350473048,1.,2.51388669270329));
#51418=CARTESIAN_POINT('Ctrl Pts',(-3.26848552888271,1.,2.51211608411539));
#51419=CARTESIAN_POINT('Ctrl Pts',(-3.26093423001716,1.,2.51031277813697));
#51420=CARTESIAN_POINT('Ctrl Pts',(-3.25339971461265,1.,2.50847647070936));
#51421=CARTESIAN_POINT('Ctrl Pts',(-3.24588208984042,1.,2.50660685940645));
#51422=CARTESIAN_POINT('Ctrl Pts',(-3.23838151080383,1.,2.50470367580078));
#51423=CARTESIAN_POINT('Ctrl Pts',(-3.23089822320596,1.,2.50276671338074));
#51424=CARTESIAN_POINT('Ctrl Pts',(-3.22343262620387,1.,2.5007958720187));
#51425=CARTESIAN_POINT('Ctrl Pts',(-3.21598526261157,1.,2.49879114599293));
#51426=CARTESIAN_POINT('Ctrl Pts',(-3.2085566984974,1.,2.49675252647298));
#51427=CARTESIAN_POINT('Ctrl Pts',(-3.20114742397549,1.,2.49467992057726));
#51428=CARTESIAN_POINT('Ctrl Pts',(-3.19375775555814,1.,2.4925730723986));
#51429=CARTESIAN_POINT('Ctrl Pts',(-3.18638771282315,1.,2.49043146334095));
#51430=CARTESIAN_POINT('Ctrl Pts',(-3.17903698136679,1.,2.48825428288243));
#51431=CARTESIAN_POINT('Ctrl Pts',(-3.17170518863357,1.,2.48604065348619));
#51432=CARTESIAN_POINT('Ctrl Pts',(-3.16439213290181,1.,2.48378981792739));
#51433=CARTESIAN_POINT('Ctrl Pts',(-3.15709802322735,1.,2.48150133566568));
#51434=CARTESIAN_POINT('Ctrl Pts',(-3.14982373241335,1.,2.47917529057016));
#51435=CARTESIAN_POINT('Ctrl Pts',(-3.14257099546531,1.,2.47681245356095));
#51436=CARTESIAN_POINT('Ctrl Pts',(-3.13534181229282,1.,2.47441378371923));
#51437=CARTESIAN_POINT('Ctrl Pts',(-3.12813790805948,1.,2.47197997765868));
#51438=CARTESIAN_POINT('Ctrl Pts',(-3.12096015766984,1.,2.4695109894747));
#51439=CARTESIAN_POINT('Ctrl Pts',(-3.11380805536124,1.,2.46700558843507));
#51440=CARTESIAN_POINT('Ctrl Pts',(-3.10667907901981,1.,2.46446082979645));
#51441=CARTESIAN_POINT('Ctrl Pts',(-3.09956993697048,1.,2.4618730850188));
#51442=CARTESIAN_POINT('Ctrl Pts',(-3.09247787931881,1.,2.45923912563875));
#51443=CARTESIAN_POINT('Ctrl Pts',(-3.08540206545313,1.,2.45655725437037));
#51444=CARTESIAN_POINT('Ctrl Pts',(-3.07834472886145,1.,2.45382826787795));
#51445=CARTESIAN_POINT('Ctrl Pts',(-3.0713129052131,1.,2.45105688854432));
#51446=CARTESIAN_POINT('Ctrl Pts',(-3.06431596421422,1.,2.44824970516558));
#51447=CARTESIAN_POINT('Ctrl Pts',(-3.05736242671521,1.,2.44541251892568));
#51448=CARTESIAN_POINT('Ctrl Pts',(-3.05045678021509,1.,2.44254768923109));
#51449=CARTESIAN_POINT('Ctrl Pts',(-3.04359685040545,1.,2.43965194061849));
#51450=CARTESIAN_POINT('Ctrl Pts',(-3.03676949672797,1.,2.43671278042394));
#51451=CARTESIAN_POINT('Ctrl Pts',(-3.02995534946946,1.,2.43371241361462));
#51452=CARTESIAN_POINT('Ctrl Pts',(-3.02313656035977,1.,2.43063415586615));
#51453=CARTESIAN_POINT('Ctrl Pts',(-3.01630420830494,1.,2.4274685626416));
#51454=CARTESIAN_POINT('Ctrl Pts',(-3.00946442616674,1.,2.42421849439625));
#51455=CARTESIAN_POINT('Ctrl Pts',(-3.00264868586038,1.,2.42090763946812));
#51456=CARTESIAN_POINT('Ctrl Pts',(-2.99590509293561,1.,2.4175732450056));
#51457=CARTESIAN_POINT('Ctrl Pts',(-2.98927983005851,1.,2.4142506419963));
#51458=CARTESIAN_POINT('Ctrl Pts',(-2.98280015815132,1.,2.41095909342591));
#51459=CARTESIAN_POINT('Ctrl Pts',(-2.97646002822395,1.,2.40768975073691));
#51460=CARTESIAN_POINT('Ctrl Pts',(-2.97019641312272,1.,2.40438604734848));
#51461=CARTESIAN_POINT('Ctrl Pts',(-2.96390432240181,1.,2.40095565711535));
#51462=CARTESIAN_POINT('Ctrl Pts',(-2.95748006482811,1.,2.39730553974412));
#51463=CARTESIAN_POINT('Ctrl Pts',(-2.95085857128372,1.,2.39337207631613));
#51464=CARTESIAN_POINT('Ctrl Pts',(-2.94404820669135,1.,2.38914929090806));
#51465=CARTESIAN_POINT('Ctrl Pts',(-2.93717903280599,1.,2.38472771516476));
#51466=CARTESIAN_POINT('Ctrl Pts',(-2.93049643640517,1.,2.3802898958232));
#51467=CARTESIAN_POINT('Ctrl Pts',(-2.92430340582912,1.,2.37606510524271));
#51468=CARTESIAN_POINT('Ctrl Pts',(-2.9189150379156,1.,2.37229381109939));
#51469=CARTESIAN_POINT('Ctrl Pts',(-2.91461249883016,1.,2.36919161373074));
#51470=CARTESIAN_POINT('Ctrl Pts',(-2.91181344022628,1.,2.36707658451709));
#51471=CARTESIAN_POINT('Ctrl Pts',(-2.91051690822262,1.,2.36599991765853));
#51472=CARTESIAN_POINT('Ctrl Pts',(-2.9100577052777,1.,2.36553202948741));
#51473=CARTESIAN_POINT('Ctrl Pts',(-2.90995756655559,1.,2.3653621118858));
#51474=CARTESIAN_POINT('Ctrl Pts',(-2.90994629141563,1.,2.36531447826213));
#51475=CARTESIAN_POINT('',(-3.35260583073571,0.,2.52982887637028));
#51476=CARTESIAN_POINT('Ctrl Pts',(-3.1487152044751,-1.,2.03668666247593));
#51477=CARTESIAN_POINT('Ctrl Pts',(-3.1487152044751,1.,2.03668666247593));
#51478=CARTESIAN_POINT('Ctrl Pts',(-3.14869618937258,-1.,2.03660173757879));
#51479=CARTESIAN_POINT('Ctrl Pts',(-3.14869618937258,1.,2.03660173757879));
#51480=CARTESIAN_POINT('Ctrl Pts',(-3.14878756590812,-1.,2.03653654935592));
#51481=CARTESIAN_POINT('Ctrl Pts',(-3.14878756590812,1.,2.03653654935592));
#51482=CARTESIAN_POINT('Ctrl Pts',(-3.14931281968048,-1.,2.03675273049189));
#51483=CARTESIAN_POINT('Ctrl Pts',(-3.14931281968048,1.,2.03675273049189));
#51484=CARTESIAN_POINT('Ctrl Pts',(-3.15079010635742,-1.,2.03766932526445));
#51485=CARTESIAN_POINT('Ctrl Pts',(-3.15079010635742,1.,2.03766932526445));
#51486=CARTESIAN_POINT('Ctrl Pts',(-3.15389991674792,-1.,2.03984073791519));
#51487=CARTESIAN_POINT('Ctrl Pts',(-3.15389991674792,1.,2.03984073791519));
#51488=CARTESIAN_POINT('Ctrl Pts',(-3.15817983946367,-1.,2.04297406404027));
#51489=CARTESIAN_POINT('Ctrl Pts',(-3.15817983946367,1.,2.04297406404027));
#51490=CARTESIAN_POINT('Ctrl Pts',(-3.16343165058912,-1.,2.04693331247446));
#51491=CARTESIAN_POINT('Ctrl Pts',(-3.16343165058912,1.,2.04693331247446));
#51492=CARTESIAN_POINT('Ctrl Pts',(-3.16936341689527,-1.,2.05151770247233));
#51493=CARTESIAN_POINT('Ctrl Pts',(-3.16936341689527,1.,2.05151770247233));
#51494=CARTESIAN_POINT('Ctrl Pts',(-3.17564906975371,-1.,2.05650186773132));
#51495=CARTESIAN_POINT('Ctrl Pts',(-3.17564906975371,1.,2.05650186773132));
#51496=CARTESIAN_POINT('Ctrl Pts',(-3.18197692964614,-1.,2.06166849827101));
#51497=CARTESIAN_POINT('Ctrl Pts',(-3.18197692964614,1.,2.06166849827101));
#51498=CARTESIAN_POINT('Ctrl Pts',(-3.18809755562368,-1.,2.06684062744112));
#51499=CARTESIAN_POINT('Ctrl Pts',(-3.18809755562368,1.,2.06684062744112));
#51500=CARTESIAN_POINT('Ctrl Pts',(-3.19388465568252,-1.,2.07192253497857));
#51501=CARTESIAN_POINT('Ctrl Pts',(-3.19388465568252,1.,2.07192253497857));
#51502=CARTESIAN_POINT('Ctrl Pts',(-3.19934132836019,-1.,2.07690441870722));
#51503=CARTESIAN_POINT('Ctrl Pts',(-3.19934132836019,1.,2.07690441870722));
#51504=CARTESIAN_POINT('Ctrl Pts',(-3.2045481863073,-1.,2.08182850370878));
#51505=CARTESIAN_POINT('Ctrl Pts',(-3.2045481863073,1.,2.08182850370878));
#51506=CARTESIAN_POINT('Ctrl Pts',(-3.20962575845463,-1.,2.08676465517455));
#51507=CARTESIAN_POINT('Ctrl Pts',(-3.20962575845463,1.,2.08676465517455));
#51508=CARTESIAN_POINT('Ctrl Pts',(-3.21469429601654,-1.,2.09178419460443));
#51509=CARTESIAN_POINT('Ctrl Pts',(-3.21469429601654,1.,2.09178419460443));
#51510=CARTESIAN_POINT('Ctrl Pts',(-3.21982707347009,-1.,2.09692958434895));
#51511=CARTESIAN_POINT('Ctrl Pts',(-3.21982707347009,1.,2.09692958434895));
#51512=CARTESIAN_POINT('Ctrl Pts',(-3.22503437553434,-1.,2.10220384298492));
#51513=CARTESIAN_POINT('Ctrl Pts',(-3.22503437553434,1.,2.10220384298492));
#51514=CARTESIAN_POINT('Ctrl Pts',(-3.23028945793289,-1.,2.10758699642451));
#51515=CARTESIAN_POINT('Ctrl Pts',(-3.23028945793289,1.,2.10758699642451));
#51516=CARTESIAN_POINT('Ctrl Pts',(-3.23554444767099,-1.,2.11304604021773));
#51517=CARTESIAN_POINT('Ctrl Pts',(-3.23554444767099,1.,2.11304604021773));
#51518=CARTESIAN_POINT('Ctrl Pts',(-3.24074905517293,-1.,2.11854673326979));
#51519=CARTESIAN_POINT('Ctrl Pts',(-3.24074905517293,1.,2.11854673326979));
#51520=CARTESIAN_POINT('Ctrl Pts',(-3.24587102613376,-1.,2.12406646410962));
#51521=CARTESIAN_POINT('Ctrl Pts',(-3.24587102613376,1.,2.12406646410962));
#51522=CARTESIAN_POINT('Ctrl Pts',(-3.25090574494028,-1.,2.12960028396832));
#51523=CARTESIAN_POINT('Ctrl Pts',(-3.25090574494028,1.,2.12960028396832));
#51524=CARTESIAN_POINT('Ctrl Pts',(-3.25586495065054,-1.,2.13515375878803));
#51525=CARTESIAN_POINT('Ctrl Pts',(-3.25586495065054,1.,2.13515375878803));
#51526=CARTESIAN_POINT('Ctrl Pts',(-3.26077002641879,-1.,2.14073870754264));
#51527=CARTESIAN_POINT('Ctrl Pts',(-3.26077002641879,1.,2.14073870754264));
#51528=CARTESIAN_POINT('Ctrl Pts',(-3.26564388189759,-1.,2.1463680529566));
#51529=CARTESIAN_POINT('Ctrl Pts',(-3.26564388189759,1.,2.1463680529566));
#51530=CARTESIAN_POINT('Ctrl Pts',(-3.27050245897228,-1.,2.15205043199808));
#51531=CARTESIAN_POINT('Ctrl Pts',(-3.27050245897228,1.,2.15205043199808));
#51532=CARTESIAN_POINT('Ctrl Pts',(-3.27534954469187,-1.,2.15778690038347));
#51533=CARTESIAN_POINT('Ctrl Pts',(-3.27534954469187,1.,2.15778690038347));
#51534=CARTESIAN_POINT('Ctrl Pts',(-3.280181508414,-1.,2.16357391934425));
#51535=CARTESIAN_POINT('Ctrl Pts',(-3.280181508414,1.,2.16357391934425));
#51536=CARTESIAN_POINT('Ctrl Pts',(-3.28499019979724,-1.,2.16940517773455));
#51537=CARTESIAN_POINT('Ctrl Pts',(-3.28499019979724,1.,2.16940517773455));
#51538=CARTESIAN_POINT('Ctrl Pts',(-3.28976645712568,-1.,2.17527380048423));
#51539=CARTESIAN_POINT('Ctrl Pts',(-3.28976645712568,1.,2.17527380048423));
#51540=CARTESIAN_POINT('Ctrl Pts',(-3.2945036150049,-1.,2.18117455557065));
#51541=CARTESIAN_POINT('Ctrl Pts',(-3.2945036150049,1.,2.18117455557065));
#51542=CARTESIAN_POINT('Ctrl Pts',(-3.29920022557639,-1.,2.18710556500327));
#51543=CARTESIAN_POINT('Ctrl Pts',(-3.29920022557639,1.,2.18710556500327));
#51544=CARTESIAN_POINT('Ctrl Pts',(-3.30385816281831,-1.,2.19306710376111));
#51545=CARTESIAN_POINT('Ctrl Pts',(-3.30385816281831,1.,2.19306710376111));
#51546=CARTESIAN_POINT('Ctrl Pts',(-3.30848134694595,-1.,2.19906078949923));
#51547=CARTESIAN_POINT('Ctrl Pts',(-3.30848134694595,1.,2.19906078949923));
#51548=CARTESIAN_POINT('Ctrl Pts',(-3.31307424608949,-1.,2.20508863150607));
#51549=CARTESIAN_POINT('Ctrl Pts',(-3.31307424608949,1.,2.20508863150607));
#51550=CARTESIAN_POINT('Ctrl Pts',(-3.31764044024235,-1.,2.21115211847875));
#51551=CARTESIAN_POINT('Ctrl Pts',(-3.31764044024235,1.,2.21115211847875));
#51552=CARTESIAN_POINT('Ctrl Pts',(-3.32218125618968,-1.,2.21725135110898));
#51553=CARTESIAN_POINT('Ctrl Pts',(-3.32218125618968,1.,2.21725135110898));
#51554=CARTESIAN_POINT('Ctrl Pts',(-3.3266964672289,-1.,2.22338548312772));
#51555=CARTESIAN_POINT('Ctrl Pts',(-3.3266964672289,1.,2.22338548312772));
#51556=CARTESIAN_POINT('Ctrl Pts',(-3.33118487773611,-1.,2.22955308907233));
#51557=CARTESIAN_POINT('Ctrl Pts',(-3.33118487773611,1.,2.22955308907233));
#51558=CARTESIAN_POINT('Ctrl Pts',(-3.33564495756482,-1.,2.23575256328812));
#51559=CARTESIAN_POINT('Ctrl Pts',(-3.33564495756482,1.,2.23575256328812));
#51560=CARTESIAN_POINT('Ctrl Pts',(-3.34007543738025,-1.,2.24198249391422));
#51561=CARTESIAN_POINT('Ctrl Pts',(-3.34007543738025,1.,2.24198249391422));
#51562=CARTESIAN_POINT('Ctrl Pts',(-3.34447596770723,-1.,2.24824207678256));
#51563=CARTESIAN_POINT('Ctrl Pts',(-3.34447596770723,1.,2.24824207678256));
#51564=CARTESIAN_POINT('Ctrl Pts',(-3.34884690292285,-1.,2.25453097693483));
#51565=CARTESIAN_POINT('Ctrl Pts',(-3.34884690292285,1.,2.25453097693483));
#51566=CARTESIAN_POINT('Ctrl Pts',(-3.35318902552626,-1.,2.26084915222449));
#51567=CARTESIAN_POINT('Ctrl Pts',(-3.35318902552626,1.,2.26084915222449));
#51568=CARTESIAN_POINT('Ctrl Pts',(-3.35750328523061,-1.,2.2671966857991));
#51569=CARTESIAN_POINT('Ctrl Pts',(-3.35750328523061,1.,2.2671966857991));
#51570=CARTESIAN_POINT('Ctrl Pts',(-3.36179055004409,-1.,2.2735736262093));
#51571=CARTESIAN_POINT('Ctrl Pts',(-3.36179055004409,1.,2.2735736262093));
#51572=CARTESIAN_POINT('Ctrl Pts',(-3.36605130713076,-1.,2.27997979458037));
#51573=CARTESIAN_POINT('Ctrl Pts',(-3.36605130713076,1.,2.27997979458037));
#51574=CARTESIAN_POINT('Ctrl Pts',(-3.37028570206488,-1.,2.28641481081137));
#51575=CARTESIAN_POINT('Ctrl Pts',(-3.37028570206488,1.,2.28641481081137));
#51576=CARTESIAN_POINT('Ctrl Pts',(-3.37449367172826,-1.,2.29287818007393));
#51577=CARTESIAN_POINT('Ctrl Pts',(-3.37449367172826,1.,2.29287818007393));
#51578=CARTESIAN_POINT('Ctrl Pts',(-3.37867504959433,-1.,2.29936936127624));
#51579=CARTESIAN_POINT('Ctrl Pts',(-3.37867504959433,1.,2.29936936127624));
#51580=CARTESIAN_POINT('Ctrl Pts',(-3.3828296733661,-1.,2.30588783640343));
#51581=CARTESIAN_POINT('Ctrl Pts',(-3.3828296733661,1.,2.30588783640343));
#51582=CARTESIAN_POINT('Ctrl Pts',(-3.38695751492462,-1.,2.31243319489367));
#51583=CARTESIAN_POINT('Ctrl Pts',(-3.38695751492462,1.,2.31243319489367));
#51584=CARTESIAN_POINT('Ctrl Pts',(-3.39105869474822,-1.,2.31900513925424));
#51585=CARTESIAN_POINT('Ctrl Pts',(-3.39105869474822,1.,2.31900513925424));
#51586=CARTESIAN_POINT('Ctrl Pts',(-3.39513342019756,-1.,2.3256034390248));
#51587=CARTESIAN_POINT('Ctrl Pts',(-3.39513342019756,1.,2.3256034390248));
#51588=CARTESIAN_POINT('Ctrl Pts',(-3.39918194577956,-1.,2.33222789882489));
#51589=CARTESIAN_POINT('Ctrl Pts',(-3.39918194577956,1.,2.33222789882489));
#51590=CARTESIAN_POINT('Ctrl Pts',(-3.40320452776743,-1.,2.33887832342782));
#51591=CARTESIAN_POINT('Ctrl Pts',(-3.40320452776743,1.,2.33887832342782));
#51592=CARTESIAN_POINT('Ctrl Pts',(-3.40720137404297,-1.,2.34555447649188));
#51593=CARTESIAN_POINT('Ctrl Pts',(-3.40720137404297,1.,2.34555447649188));
#51594=CARTESIAN_POINT('Ctrl Pts',(-3.41117262314119,-1.,2.35225606824109));
#51595=CARTESIAN_POINT('Ctrl Pts',(-3.41117262314119,1.,2.35225606824109));
#51596=CARTESIAN_POINT('Ctrl Pts',(-3.41511836751469,-1.,2.35898278606946));
#51597=CARTESIAN_POINT('Ctrl Pts',(-3.41511836751469,1.,2.35898278606946));
#51598=CARTESIAN_POINT('Ctrl Pts',(-3.41903866635852,-1.,2.36573431470642));
#51599=CARTESIAN_POINT('Ctrl Pts',(-3.41903866635852,1.,2.36573431470642));
#51600=CARTESIAN_POINT('Ctrl Pts',(-3.42293356216511,-1.,2.37251035954292));
#51601=CARTESIAN_POINT('Ctrl Pts',(-3.42293356216511,1.,2.37251035954292));
#51602=CARTESIAN_POINT('Ctrl Pts',(-3.42680309754399,-1.,2.37931067028926));
#51603=CARTESIAN_POINT('Ctrl Pts',(-3.42680309754399,1.,2.37931067028926));
#51604=CARTESIAN_POINT('Ctrl Pts',(-3.4306473271292,-1.,2.38613505843552));
#51605=CARTESIAN_POINT('Ctrl Pts',(-3.4306473271292,1.,2.38613505843552));
#51606=CARTESIAN_POINT('Ctrl Pts',(-3.4344663067854,-1.,2.39298338804493));
#51607=CARTESIAN_POINT('Ctrl Pts',(-3.4344663067854,1.,2.39298338804493));
#51608=CARTESIAN_POINT('Ctrl Pts',(-3.43750133064416,-1.,2.39848113410292));
#51609=CARTESIAN_POINT('Ctrl Pts',(-3.43750133064416,1.,2.39848113410292));
#51610=CARTESIAN_POINT('Ctrl Pts',(-3.43976627484234,-1.,2.40261515589405));
#51611=CARTESIAN_POINT('Ctrl Pts',(-3.43976627484234,1.,2.40261515589405));
#51612=CARTESIAN_POINT('Ctrl Pts',(-3.44127120683039,-1.,2.4053759295909));
#51613=CARTESIAN_POINT('Ctrl Pts',(-3.44127120683039,1.,2.4053759295909));
#51614=CARTESIAN_POINT('Ctrl Pts',(-3.44202241512147,-1.,2.40675750623143));
#51615=CARTESIAN_POINT('Ctrl Pts',(-3.44202241512147,1.,2.40675750623143));
#51616=CARTESIAN_POINT('',(-3.14877060440327,1.,2.03660101169715));
#51617=CARTESIAN_POINT('Ctrl Pts',(-3.14877060440327,-1.,2.03660101169715));
#51618=CARTESIAN_POINT('Ctrl Pts',(-3.14877060440327,-0.666666666666667,
2.03660101169715));
#51619=CARTESIAN_POINT('Ctrl Pts',(-3.14877060440327,-0.333333333333333,
2.03660101169715));
#51620=CARTESIAN_POINT('Ctrl Pts',(-3.14877060440327,0.333333333333333,
2.03660101169715));
#51621=CARTESIAN_POINT('Ctrl Pts',(-3.14877060440327,0.666666666666667,
2.03660101169715));
#51622=CARTESIAN_POINT('Ctrl Pts',(-3.14877060440327,1.,2.03660101169715));
#51623=CARTESIAN_POINT('',(-3.44202241512147,1.,2.40675750623143));
#51624=CARTESIAN_POINT('',(-3.44202241512147,0.,2.40675750623143));
#51625=CARTESIAN_POINT('Ctrl Pts',(-3.14877060440327,1.,2.03660101169715));
#51626=CARTESIAN_POINT('Ctrl Pts',(-3.14881939088124,1.,2.03659701539259));
#51627=CARTESIAN_POINT('Ctrl Pts',(-3.1490119366901,1.,2.03663974554932));
#51628=CARTESIAN_POINT('Ctrl Pts',(-3.14959882629805,1.,2.03693188810544));
#51629=CARTESIAN_POINT('Ctrl Pts',(-3.15102344775328,1.,2.03783225495961));
#51630=CARTESIAN_POINT('Ctrl Pts',(-3.15389991674792,1.,2.03984073791519));
#51631=CARTESIAN_POINT('Ctrl Pts',(-3.15817983946367,1.,2.04297406404027));
#51632=CARTESIAN_POINT('Ctrl Pts',(-3.16343165058912,1.,2.04693331247446));
#51633=CARTESIAN_POINT('Ctrl Pts',(-3.16936341689527,1.,2.05151770247233));
#51634=CARTESIAN_POINT('Ctrl Pts',(-3.17564906975371,1.,2.05650186773132));
#51635=CARTESIAN_POINT('Ctrl Pts',(-3.18197692964614,1.,2.06166849827101));
#51636=CARTESIAN_POINT('Ctrl Pts',(-3.18809755562368,1.,2.06684062744112));
#51637=CARTESIAN_POINT('Ctrl Pts',(-3.19388465568252,1.,2.07192253497857));
#51638=CARTESIAN_POINT('Ctrl Pts',(-3.19934132836019,1.,2.07690441870722));
#51639=CARTESIAN_POINT('Ctrl Pts',(-3.2045481863073,1.,2.08182850370878));
#51640=CARTESIAN_POINT('Ctrl Pts',(-3.20962575845463,1.,2.08676465517455));
#51641=CARTESIAN_POINT('Ctrl Pts',(-3.21469429601654,1.,2.09178419460443));
#51642=CARTESIAN_POINT('Ctrl Pts',(-3.21982707347009,1.,2.09692958434895));
#51643=CARTESIAN_POINT('Ctrl Pts',(-3.22503437553434,1.,2.10220384298492));
#51644=CARTESIAN_POINT('Ctrl Pts',(-3.23028945793289,1.,2.10758699642451));
#51645=CARTESIAN_POINT('Ctrl Pts',(-3.23554444767099,1.,2.11304604021773));
#51646=CARTESIAN_POINT('Ctrl Pts',(-3.24074905517293,1.,2.11854673326979));
#51647=CARTESIAN_POINT('Ctrl Pts',(-3.24587102613376,1.,2.12406646410962));
#51648=CARTESIAN_POINT('Ctrl Pts',(-3.25090574494028,1.,2.12960028396832));
#51649=CARTESIAN_POINT('Ctrl Pts',(-3.25586495065054,1.,2.13515375878803));
#51650=CARTESIAN_POINT('Ctrl Pts',(-3.26077002641879,1.,2.14073870754264));
#51651=CARTESIAN_POINT('Ctrl Pts',(-3.26564388189759,1.,2.1463680529566));
#51652=CARTESIAN_POINT('Ctrl Pts',(-3.27050245897228,1.,2.15205043199808));
#51653=CARTESIAN_POINT('Ctrl Pts',(-3.27534954469187,1.,2.15778690038347));
#51654=CARTESIAN_POINT('Ctrl Pts',(-3.280181508414,1.,2.16357391934425));
#51655=CARTESIAN_POINT('Ctrl Pts',(-3.28499019979724,1.,2.16940517773455));
#51656=CARTESIAN_POINT('Ctrl Pts',(-3.28976645712568,1.,2.17527380048423));
#51657=CARTESIAN_POINT('Ctrl Pts',(-3.2945036150049,1.,2.18117455557065));
#51658=CARTESIAN_POINT('Ctrl Pts',(-3.29920022557639,1.,2.18710556500327));
#51659=CARTESIAN_POINT('Ctrl Pts',(-3.30385816281831,1.,2.19306710376111));
#51660=CARTESIAN_POINT('Ctrl Pts',(-3.30848134694595,1.,2.19906078949923));
#51661=CARTESIAN_POINT('Ctrl Pts',(-3.31307424608949,1.,2.20508863150607));
#51662=CARTESIAN_POINT('Ctrl Pts',(-3.31764044024235,1.,2.21115211847875));
#51663=CARTESIAN_POINT('Ctrl Pts',(-3.32218125618968,1.,2.21725135110898));
#51664=CARTESIAN_POINT('Ctrl Pts',(-3.3266964672289,1.,2.22338548312772));
#51665=CARTESIAN_POINT('Ctrl Pts',(-3.33118487773611,1.,2.22955308907233));
#51666=CARTESIAN_POINT('Ctrl Pts',(-3.33564495756482,1.,2.23575256328812));
#51667=CARTESIAN_POINT('Ctrl Pts',(-3.34007543738025,1.,2.24198249391422));
#51668=CARTESIAN_POINT('Ctrl Pts',(-3.34447596770723,1.,2.24824207678256));
#51669=CARTESIAN_POINT('Ctrl Pts',(-3.34884690292285,1.,2.25453097693483));
#51670=CARTESIAN_POINT('Ctrl Pts',(-3.35318902552626,1.,2.26084915222449));
#51671=CARTESIAN_POINT('Ctrl Pts',(-3.35750328523061,1.,2.2671966857991));
#51672=CARTESIAN_POINT('Ctrl Pts',(-3.36179055004409,1.,2.2735736262093));
#51673=CARTESIAN_POINT('Ctrl Pts',(-3.36605130713076,1.,2.27997979458037));
#51674=CARTESIAN_POINT('Ctrl Pts',(-3.37028570206488,1.,2.28641481081137));
#51675=CARTESIAN_POINT('Ctrl Pts',(-3.37449367172826,1.,2.29287818007393));
#51676=CARTESIAN_POINT('Ctrl Pts',(-3.37867504959433,1.,2.29936936127624));
#51677=CARTESIAN_POINT('Ctrl Pts',(-3.3828296733661,1.,2.30588783640343));
#51678=CARTESIAN_POINT('Ctrl Pts',(-3.38695751492462,1.,2.31243319489367));
#51679=CARTESIAN_POINT('Ctrl Pts',(-3.39105869474822,1.,2.31900513925424));
#51680=CARTESIAN_POINT('Ctrl Pts',(-3.39513342019756,1.,2.3256034390248));
#51681=CARTESIAN_POINT('Ctrl Pts',(-3.39918194577956,1.,2.33222789882489));
#51682=CARTESIAN_POINT('Ctrl Pts',(-3.40320452776743,1.,2.33887832342782));
#51683=CARTESIAN_POINT('Ctrl Pts',(-3.40720137404297,1.,2.34555447649188));
#51684=CARTESIAN_POINT('Ctrl Pts',(-3.41117262314119,1.,2.35225606824109));
#51685=CARTESIAN_POINT('Ctrl Pts',(-3.41511836751469,1.,2.35898278606946));
#51686=CARTESIAN_POINT('Ctrl Pts',(-3.41903866635852,1.,2.36573431470642));
#51687=CARTESIAN_POINT('Ctrl Pts',(-3.42293356216511,1.,2.37251035954292));
#51688=CARTESIAN_POINT('Ctrl Pts',(-3.42680309754399,1.,2.37931067028926));
#51689=CARTESIAN_POINT('Ctrl Pts',(-3.4306473271292,1.,2.38613505843552));
#51690=CARTESIAN_POINT('Ctrl Pts',(-3.4344663067854,1.,2.39298338804493));
#51691=CARTESIAN_POINT('Ctrl Pts',(-3.43750133064416,1.,2.39848113410292));
#51692=CARTESIAN_POINT('Ctrl Pts',(-3.43976627484234,1.,2.40261515589405));
#51693=CARTESIAN_POINT('Ctrl Pts',(-3.44127120683039,1.,2.4053759295909));
#51694=CARTESIAN_POINT('Ctrl Pts',(-3.44202241512147,1.,2.40675750623143));
#51695=CARTESIAN_POINT('Origin',(-3.44202241512147,0.,2.40675750623143));
#51696=CARTESIAN_POINT('',(-3.35260583073571,1.,2.52982887637028));
#51697=CARTESIAN_POINT('Origin',(0.,0.,0.));
#51698=CARTESIAN_POINT('',(-3.24413672884812,1.,1.88097764062697));
#51699=CARTESIAN_POINT('Origin',(0.,1.,0.));
#51700=CARTESIAN_POINT('Ctrl Pts',(-3.24413672884812,1.,1.88097764062697));
#51701=CARTESIAN_POINT('Ctrl Pts',(-3.24413672884812,0.666666666666667,
1.88097764062697));
#51702=CARTESIAN_POINT('Ctrl Pts',(-3.24413672884812,0.333333333333333,
1.88097764062697));
#51703=CARTESIAN_POINT('Ctrl Pts',(-3.24413672884812,-0.333333333333333,
1.88097764062697));
#51704=CARTESIAN_POINT('Ctrl Pts',(-3.24413672884812,-0.666666666666667,
1.88097764062697));
#51705=CARTESIAN_POINT('Ctrl Pts',(-3.24413672884812,-1.,1.88097764062697));
#51706=CARTESIAN_POINT('Ctrl Pts',(-3.70708211654725,-1.,1.97421938526992));
#51707=CARTESIAN_POINT('Ctrl Pts',(-3.70708211654725,1.,1.97421938526992));
#51708=CARTESIAN_POINT('Ctrl Pts',(-3.70551008132332,-1.,1.97417727645308));
#51709=CARTESIAN_POINT('Ctrl Pts',(-3.70551008132332,1.,1.97417727645308));
#51710=CARTESIAN_POINT('Ctrl Pts',(-3.70236698912904,-1.,1.97408973726715));
#51711=CARTESIAN_POINT('Ctrl Pts',(-3.70236698912904,1.,1.97408973726715));
#51712=CARTESIAN_POINT('Ctrl Pts',(-3.6976552856004,-1.,1.97394846383216));
#51713=CARTESIAN_POINT('Ctrl Pts',(-3.6976552856004,1.,1.97394846383216));
#51714=CARTESIAN_POINT('Ctrl Pts',(-3.69137888599902,-1.,1.97374016225483));
#51715=CARTESIAN_POINT('Ctrl Pts',(-3.69137888599902,1.,1.97374016225483));
#51716=CARTESIAN_POINT('Ctrl Pts',(-3.68354319915092,-1.,1.97344650304519));
#51717=CARTESIAN_POINT('Ctrl Pts',(-3.68354319915092,1.,1.97344650304519));
#51718=CARTESIAN_POINT('Ctrl Pts',(-3.67571738107084,-1.,1.97311947678516));
#51719=CARTESIAN_POINT('Ctrl Pts',(-3.67571738107084,1.,1.97311947678516));
#51720=CARTESIAN_POINT('Ctrl Pts',(-3.66790152752075,-1.,1.97275897198678));
#51721=CARTESIAN_POINT('Ctrl Pts',(-3.66790152752075,1.,1.97275897198678));
#51722=CARTESIAN_POINT('Ctrl Pts',(-3.6600957816636,-1.,1.9723648543905));
#51723=CARTESIAN_POINT('Ctrl Pts',(-3.6600957816636,1.,1.9723648543905));
#51724=CARTESIAN_POINT('Ctrl Pts',(-3.652300347166,-1.,1.9719369724024));
#51725=CARTESIAN_POINT('Ctrl Pts',(-3.652300347166,1.,1.9719369724024));
#51726=CARTESIAN_POINT('Ctrl Pts',(-3.64451546723514,-1.,1.97147515441164));
#51727=CARTESIAN_POINT('Ctrl Pts',(-3.64451546723514,1.,1.97147515441164));
#51728=CARTESIAN_POINT('Ctrl Pts',(-3.63674139590412,-1.,1.97097920454464));
#51729=CARTESIAN_POINT('Ctrl Pts',(-3.63674139590412,1.,1.97097920454464));
#51730=CARTESIAN_POINT('Ctrl Pts',(-3.62897836973293,-1.,1.97044889850463));
#51731=CARTESIAN_POINT('Ctrl Pts',(-3.62897836973293,1.,1.97044889850463));
#51732=CARTESIAN_POINT('Ctrl Pts',(-3.62122658401893,-1.,1.96988398129978));
#51733=CARTESIAN_POINT('Ctrl Pts',(-3.62122658401893,1.,1.96988398129978));
#51734=CARTESIAN_POINT('Ctrl Pts',(-3.61348615496704,-1.,1.96928416040877));
#51735=CARTESIAN_POINT('Ctrl Pts',(-3.61348615496704,1.,1.96928416040877));
#51736=CARTESIAN_POINT('Ctrl Pts',(-3.60575714017989,-1.,1.9686491188594));
#51737=CARTESIAN_POINT('Ctrl Pts',(-3.60575714017989,1.,1.9686491188594));
#51738=CARTESIAN_POINT('Ctrl Pts',(-3.59803959819938,-1.,1.96797854118369));
#51739=CARTESIAN_POINT('Ctrl Pts',(-3.59803959819938,1.,1.96797854118369));
#51740=CARTESIAN_POINT('Ctrl Pts',(-3.59033364022801,-1.,1.96727213799544));
#51741=CARTESIAN_POINT('Ctrl Pts',(-3.59033364022801,1.,1.96727213799544));
#51742=CARTESIAN_POINT('Ctrl Pts',(-3.58263947663829,-1.,1.96652966688911));
#51743=CARTESIAN_POINT('Ctrl Pts',(-3.58263947663829,1.,1.96652966688911));
#51744=CARTESIAN_POINT('Ctrl Pts',(-3.57495748600959,-1.,1.96575096652789));
#51745=CARTESIAN_POINT('Ctrl Pts',(-3.57495748600959,1.,1.96575096652789));
#51746=CARTESIAN_POINT('Ctrl Pts',(-3.56728820357791,-1.,1.96493594634567));
#51747=CARTESIAN_POINT('Ctrl Pts',(-3.56728820357791,1.,1.96493594634567));
#51748=CARTESIAN_POINT('Ctrl Pts',(-3.55963218706096,-1.,1.96408450906812));
#51749=CARTESIAN_POINT('Ctrl Pts',(-3.55963218706096,1.,1.96408450906812));
#51750=CARTESIAN_POINT('Ctrl Pts',(-3.55198990600886,-1.,1.96319648628644));
#51751=CARTESIAN_POINT('Ctrl Pts',(-3.55198990600886,1.,1.96319648628644));
#51752=CARTESIAN_POINT('Ctrl Pts',(-3.54436163300443,-1.,1.96227157573067));
#51753=CARTESIAN_POINT('Ctrl Pts',(-3.54436163300443,1.,1.96227157573067));
#51754=CARTESIAN_POINT('Ctrl Pts',(-3.53674730625813,-1.,1.96130926212689));
#51755=CARTESIAN_POINT('Ctrl Pts',(-3.53674730625813,1.,1.96130926212689));
#51756=CARTESIAN_POINT('Ctrl Pts',(-3.52914648844351,-1.,1.96030879411566));
#51757=CARTESIAN_POINT('Ctrl Pts',(-3.52914648844351,1.,1.96030879411566));
#51758=CARTESIAN_POINT('Ctrl Pts',(-3.52155867431486,-1.,1.95926936324461));
#51759=CARTESIAN_POINT('Ctrl Pts',(-3.52155867431486,1.,1.95926936324461));
#51760=CARTESIAN_POINT('Ctrl Pts',(-3.51398354617794,-1.,1.95819025316779));
#51761=CARTESIAN_POINT('Ctrl Pts',(-3.51398354617794,1.,1.95819025316779));
#51762=CARTESIAN_POINT('Ctrl Pts',(-3.50642124159909,-1.,1.95707099606511));
#51763=CARTESIAN_POINT('Ctrl Pts',(-3.50642124159909,1.,1.95707099606511));
#51764=CARTESIAN_POINT('Ctrl Pts',(-3.49887263575583,-1.,1.95591153823661));
#51765=CARTESIAN_POINT('Ctrl Pts',(-3.49887263575583,1.,1.95591153823661));
#51766=CARTESIAN_POINT('Ctrl Pts',(-3.49133956289133,-1.,1.95471236969643));
#51767=CARTESIAN_POINT('Ctrl Pts',(-3.49133956289133,1.,1.95471236969643));
#51768=CARTESIAN_POINT('Ctrl Pts',(-3.48382414832634,-1.,1.95347412486308));
#51769=CARTESIAN_POINT('Ctrl Pts',(-3.48382414832634,1.,1.95347412486308));
#51770=CARTESIAN_POINT('Ctrl Pts',(-3.47632820495921,-1.,1.95219722189876));
#51771=CARTESIAN_POINT('Ctrl Pts',(-3.47632820495921,1.,1.95219722189876));
#51772=CARTESIAN_POINT('Ctrl Pts',(-3.46885258974191,-1.,1.95088147859876));
#51773=CARTESIAN_POINT('Ctrl Pts',(-3.46885258974191,1.,1.95088147859876));
#51774=CARTESIAN_POINT('Ctrl Pts',(-3.46139661060962,-1.,1.94952575850197));
#51775=CARTESIAN_POINT('Ctrl Pts',(-3.46139661060962,1.,1.94952575850197));
#51776=CARTESIAN_POINT('Ctrl Pts',(-3.45395731584051,-1.,1.94812754766524));
#51777=CARTESIAN_POINT('Ctrl Pts',(-3.45395731584051,1.,1.94812754766524));
#51778=CARTESIAN_POINT('Ctrl Pts',(-3.44653088665681,-1.,1.94668377715329));
#51779=CARTESIAN_POINT('Ctrl Pts',(-3.44653088665681,1.,1.94668377715329));
#51780=CARTESIAN_POINT('Ctrl Pts',(-3.43911410197687,-1.,1.94519168842879));
#51781=CARTESIAN_POINT('Ctrl Pts',(-3.43911410197687,1.,1.94519168842879));
#51782=CARTESIAN_POINT('Ctrl Pts',(-3.43170586602434,-1.,1.94364973660284));
#51783=CARTESIAN_POINT('Ctrl Pts',(-3.43170586602434,1.,1.94364973660284));
#51784=CARTESIAN_POINT('Ctrl Pts',(-3.42430850941503,-1.,1.94205835913696));
#51785=CARTESIAN_POINT('Ctrl Pts',(-3.42430850941503,1.,1.94205835913696));
#51786=CARTESIAN_POINT('Ctrl Pts',(-3.41692971994096,-1.,1.94042111965246));
#51787=CARTESIAN_POINT('Ctrl Pts',(-3.41692971994096,1.,1.94042111965246));
#51788=CARTESIAN_POINT('Ctrl Pts',(-3.40957978266642,-1.,1.93874306008143));
#51789=CARTESIAN_POINT('Ctrl Pts',(-3.40957978266642,1.,1.93874306008143));
#51790=CARTESIAN_POINT('Ctrl Pts',(-3.40226802104109,-1.,1.93702857723098));
#51791=CARTESIAN_POINT('Ctrl Pts',(-3.40226802104109,1.,1.93702857723098));
#51792=CARTESIAN_POINT('Ctrl Pts',(-3.39499923640795,-1.,1.93527929945985));
#51793=CARTESIAN_POINT('Ctrl Pts',(-3.39499923640795,1.,1.93527929945985));
#51794=CARTESIAN_POINT('Ctrl Pts',(-3.38777076883256,-1.,1.93349233176788));
#51795=CARTESIAN_POINT('Ctrl Pts',(-3.38777076883256,1.,1.93349233176788));
#51796=CARTESIAN_POINT('Ctrl Pts',(-3.3805676852555,-1.,1.93165739093276));
#51797=CARTESIAN_POINT('Ctrl Pts',(-3.3805676852555,1.,1.93165739093276));
#51798=CARTESIAN_POINT('Ctrl Pts',(-3.37336807068043,-1.,1.92975993109877));
#51799=CARTESIAN_POINT('Ctrl Pts',(-3.37336807068043,1.,1.92975993109877));
#51800=CARTESIAN_POINT('Ctrl Pts',(-3.36615168657567,-1.,1.92778626543786));
#51801=CARTESIAN_POINT('Ctrl Pts',(-3.36615168657567,1.,1.92778626543786));
#51802=CARTESIAN_POINT('Ctrl Pts',(-3.35890824422965,-1.,1.92572846125756));
#51803=CARTESIAN_POINT('Ctrl Pts',(-3.35890824422965,1.,1.92572846125756));
#51804=CARTESIAN_POINT('Ctrl Pts',(-3.35164424847223,-1.,1.92358838440528));
#51805=CARTESIAN_POINT('Ctrl Pts',(-3.35164424847223,1.,1.92358838440528));
#51806=CARTESIAN_POINT('Ctrl Pts',(-3.34439448941961,-1.,1.92138450828404));
#51807=CARTESIAN_POINT('Ctrl Pts',(-3.34439448941961,1.,1.92138450828404));
#51808=CARTESIAN_POINT('Ctrl Pts',(-3.33721230710012,-1.,1.9191460961021));
#51809=CARTESIAN_POINT('Ctrl Pts',(-3.33721230710012,1.,1.9191460961021));
#51810=CARTESIAN_POINT('Ctrl Pts',(-3.33014884257873,-1.,1.91690081930331));
#51811=CARTESIAN_POINT('Ctrl Pts',(-3.33014884257873,1.,1.91690081930331));
#51812=CARTESIAN_POINT('Ctrl Pts',(-3.32323403454535,-1.,1.91466343916628));
#51813=CARTESIAN_POINT('Ctrl Pts',(-3.32323403454535,1.,1.91466343916628));
#51814=CARTESIAN_POINT('Ctrl Pts',(-3.31646052426364,-1.,1.91242616234442));
#51815=CARTESIAN_POINT('Ctrl Pts',(-3.31646052426364,1.,1.91242616234442));
#51816=CARTESIAN_POINT('Ctrl Pts',(-3.30975721158596,-1.,1.91014297830446));
#51817=CARTESIAN_POINT('Ctrl Pts',(-3.30975721158596,1.,1.91014297830446));
#51818=CARTESIAN_POINT('Ctrl Pts',(-3.30300595568195,-1.,1.90773912171341));
#51819=CARTESIAN_POINT('Ctrl Pts',(-3.30300595568195,1.,1.90773912171341));
#51820=CARTESIAN_POINT('Ctrl Pts',(-3.29608978722113,-1.,1.90513891864087));
#51821=CARTESIAN_POINT('Ctrl Pts',(-3.29608978722113,1.,1.90513891864087));
#51822=CARTESIAN_POINT('Ctrl Pts',(-3.2889344860029,-1.,1.90228971247527));
#51823=CARTESIAN_POINT('Ctrl Pts',(-3.2889344860029,1.,1.90228971247527));
#51824=CARTESIAN_POINT('Ctrl Pts',(-3.28154737912352,-1.,1.89918429230462));
#51825=CARTESIAN_POINT('Ctrl Pts',(-3.28154737912352,1.,1.89918429230462));
#51826=CARTESIAN_POINT('Ctrl Pts',(-3.27407108933139,-1.,1.89589172903793));
#51827=CARTESIAN_POINT('Ctrl Pts',(-3.27407108933139,1.,1.89589172903793));
#51828=CARTESIAN_POINT('Ctrl Pts',(-3.26677653888676,-1.,1.89255393500965));
#51829=CARTESIAN_POINT('Ctrl Pts',(-3.26677653888676,1.,1.89255393500965));
#51830=CARTESIAN_POINT('Ctrl Pts',(-3.25999885193947,-1.,1.88934996203698));
#51831=CARTESIAN_POINT('Ctrl Pts',(-3.25999885193947,1.,1.88934996203698));
#51832=CARTESIAN_POINT('Ctrl Pts',(-3.25408686339463,-1.,1.88646802523466));
#51833=CARTESIAN_POINT('Ctrl Pts',(-3.25408686339463,1.,1.88646802523466));
#51834=CARTESIAN_POINT('Ctrl Pts',(-3.24935200511918,-1.,1.88407708646357));
#51835=CARTESIAN_POINT('Ctrl Pts',(-3.24935200511918,1.,1.88407708646357));
#51836=CARTESIAN_POINT('Ctrl Pts',(-3.24600543790443,-1.,1.88229202582941));
#51837=CARTESIAN_POINT('Ctrl Pts',(-3.24600543790443,1.,1.88229202582941));
#51838=CARTESIAN_POINT('Ctrl Pts',(-3.24451807186481,-1.,1.88139187908074));
#51839=CARTESIAN_POINT('Ctrl Pts',(-3.24451807186481,1.,1.88139187908074));
#51840=CARTESIAN_POINT('Ctrl Pts',(-3.24408699284121,-1.,1.88102201872555));
#51841=CARTESIAN_POINT('Ctrl Pts',(-3.24408699284121,1.,1.88102201872555));
#51842=CARTESIAN_POINT('Ctrl Pts',(-3.24410359189609,-1.,1.88091100680349));
#51843=CARTESIAN_POINT('Ctrl Pts',(-3.24410359189609,1.,1.88091100680349));
#51844=CARTESIAN_POINT('Ctrl Pts',(-3.24418789321065,-1.,1.8808893942881));
#51845=CARTESIAN_POINT('Ctrl Pts',(-3.24418789321065,1.,1.8808893942881));
#51846=CARTESIAN_POINT('',(-3.70708211654725,1.,1.97421938526992));
#51847=CARTESIAN_POINT('Ctrl Pts',(-3.70708211654725,1.,1.97421938526992));
#51848=CARTESIAN_POINT('Ctrl Pts',(-3.70551008132332,1.,1.97417727645308));
#51849=CARTESIAN_POINT('Ctrl Pts',(-3.70236698912904,1.,1.97408973726715));
#51850=CARTESIAN_POINT('Ctrl Pts',(-3.6976552856004,1.,1.97394846383216));
#51851=CARTESIAN_POINT('Ctrl Pts',(-3.69137888599902,1.,1.97374016225483));
#51852=CARTESIAN_POINT('Ctrl Pts',(-3.68354319915092,1.,1.97344650304519));
#51853=CARTESIAN_POINT('Ctrl Pts',(-3.67571738107084,1.,1.97311947678516));
#51854=CARTESIAN_POINT('Ctrl Pts',(-3.66790152752075,1.,1.97275897198678));
#51855=CARTESIAN_POINT('Ctrl Pts',(-3.6600957816636,1.,1.9723648543905));
#51856=CARTESIAN_POINT('Ctrl Pts',(-3.652300347166,1.,1.9719369724024));
#51857=CARTESIAN_POINT('Ctrl Pts',(-3.64451546723514,1.,1.97147515441164));
#51858=CARTESIAN_POINT('Ctrl Pts',(-3.63674139590412,1.,1.97097920454464));
#51859=CARTESIAN_POINT('Ctrl Pts',(-3.62897836973293,1.,1.97044889850463));
#51860=CARTESIAN_POINT('Ctrl Pts',(-3.62122658401893,1.,1.96988398129978));
#51861=CARTESIAN_POINT('Ctrl Pts',(-3.61348615496704,1.,1.96928416040877));
#51862=CARTESIAN_POINT('Ctrl Pts',(-3.60575714017989,1.,1.9686491188594));
#51863=CARTESIAN_POINT('Ctrl Pts',(-3.59803959819938,1.,1.96797854118369));
#51864=CARTESIAN_POINT('Ctrl Pts',(-3.59033364022801,1.,1.96727213799544));
#51865=CARTESIAN_POINT('Ctrl Pts',(-3.58263947663829,1.,1.96652966688911));
#51866=CARTESIAN_POINT('Ctrl Pts',(-3.57495748600959,1.,1.96575096652789));
#51867=CARTESIAN_POINT('Ctrl Pts',(-3.56728820357791,1.,1.96493594634567));
#51868=CARTESIAN_POINT('Ctrl Pts',(-3.55963218706096,1.,1.96408450906812));
#51869=CARTESIAN_POINT('Ctrl Pts',(-3.55198990600886,1.,1.96319648628644));
#51870=CARTESIAN_POINT('Ctrl Pts',(-3.54436163300443,1.,1.96227157573067));
#51871=CARTESIAN_POINT('Ctrl Pts',(-3.53674730625813,1.,1.96130926212689));
#51872=CARTESIAN_POINT('Ctrl Pts',(-3.52914648844351,1.,1.96030879411566));
#51873=CARTESIAN_POINT('Ctrl Pts',(-3.52155867431486,1.,1.95926936324461));
#51874=CARTESIAN_POINT('Ctrl Pts',(-3.51398354617794,1.,1.95819025316779));
#51875=CARTESIAN_POINT('Ctrl Pts',(-3.50642124159909,1.,1.95707099606511));
#51876=CARTESIAN_POINT('Ctrl Pts',(-3.49887263575583,1.,1.95591153823661));
#51877=CARTESIAN_POINT('Ctrl Pts',(-3.49133956289133,1.,1.95471236969643));
#51878=CARTESIAN_POINT('Ctrl Pts',(-3.48382414832634,1.,1.95347412486308));
#51879=CARTESIAN_POINT('Ctrl Pts',(-3.47632820495921,1.,1.95219722189876));
#51880=CARTESIAN_POINT('Ctrl Pts',(-3.46885258974191,1.,1.95088147859876));
#51881=CARTESIAN_POINT('Ctrl Pts',(-3.46139661060962,1.,1.94952575850197));
#51882=CARTESIAN_POINT('Ctrl Pts',(-3.45395731584051,1.,1.94812754766524));
#51883=CARTESIAN_POINT('Ctrl Pts',(-3.44653088665681,1.,1.94668377715329));
#51884=CARTESIAN_POINT('Ctrl Pts',(-3.43911410197687,1.,1.94519168842879));
#51885=CARTESIAN_POINT('Ctrl Pts',(-3.43170586602434,1.,1.94364973660284));
#51886=CARTESIAN_POINT('Ctrl Pts',(-3.42430850941503,1.,1.94205835913696));
#51887=CARTESIAN_POINT('Ctrl Pts',(-3.41692971994096,1.,1.94042111965246));
#51888=CARTESIAN_POINT('Ctrl Pts',(-3.40957978266642,1.,1.93874306008143));
#51889=CARTESIAN_POINT('Ctrl Pts',(-3.40226802104109,1.,1.93702857723098));
#51890=CARTESIAN_POINT('Ctrl Pts',(-3.39499923640795,1.,1.93527929945985));
#51891=CARTESIAN_POINT('Ctrl Pts',(-3.38777076883256,1.,1.93349233176788));
#51892=CARTESIAN_POINT('Ctrl Pts',(-3.3805676852555,1.,1.93165739093276));
#51893=CARTESIAN_POINT('Ctrl Pts',(-3.37336807068043,1.,1.92975993109877));
#51894=CARTESIAN_POINT('Ctrl Pts',(-3.36615168657567,1.,1.92778626543786));
#51895=CARTESIAN_POINT('Ctrl Pts',(-3.35890824422965,1.,1.92572846125756));
#51896=CARTESIAN_POINT('Ctrl Pts',(-3.35164424847223,1.,1.92358838440528));
#51897=CARTESIAN_POINT('Ctrl Pts',(-3.34439448941961,1.,1.92138450828404));
#51898=CARTESIAN_POINT('Ctrl Pts',(-3.33721230710012,1.,1.9191460961021));
#51899=CARTESIAN_POINT('Ctrl Pts',(-3.33014884257873,1.,1.91690081930331));
#51900=CARTESIAN_POINT('Ctrl Pts',(-3.32323403454535,1.,1.91466343916628));
#51901=CARTESIAN_POINT('Ctrl Pts',(-3.31646052426364,1.,1.91242616234442));
#51902=CARTESIAN_POINT('Ctrl Pts',(-3.30975721158596,1.,1.91014297830446));
#51903=CARTESIAN_POINT('Ctrl Pts',(-3.30300595568195,1.,1.90773912171341));
#51904=CARTESIAN_POINT('Ctrl Pts',(-3.29608978722113,1.,1.90513891864087));
#51905=CARTESIAN_POINT('Ctrl Pts',(-3.2889344860029,1.,1.90228971247527));
#51906=CARTESIAN_POINT('Ctrl Pts',(-3.28154737912352,1.,1.89918429230462));
#51907=CARTESIAN_POINT('Ctrl Pts',(-3.27407108933139,1.,1.89589172903793));
#51908=CARTESIAN_POINT('Ctrl Pts',(-3.26677653888676,1.,1.89255393500965));
#51909=CARTESIAN_POINT('Ctrl Pts',(-3.25999885193947,1.,1.88934996203698));
#51910=CARTESIAN_POINT('Ctrl Pts',(-3.25408686339463,1.,1.88646802523466));
#51911=CARTESIAN_POINT('Ctrl Pts',(-3.24935200511918,1.,1.88407708646357));
#51912=CARTESIAN_POINT('Ctrl Pts',(-3.2462565441079,1.,1.88242596600454));
#51913=CARTESIAN_POINT('Ctrl Pts',(-3.24480754676064,1.,1.88156537699203));
#51914=CARTESIAN_POINT('Ctrl Pts',(-3.24428080353022,1.,1.88117508446775));
#51915=CARTESIAN_POINT('Ctrl Pts',(-3.24415531671284,1.,1.8810229239812));
#51916=CARTESIAN_POINT('Ctrl Pts',(-3.24413672884812,1.,1.88097764062697));
#51917=CARTESIAN_POINT('',(-3.70708211654725,0.,1.97421938526992));
#51918=CARTESIAN_POINT('Ctrl Pts',(-3.42855728381368,-1.,1.519044091397));
#51919=CARTESIAN_POINT('Ctrl Pts',(-3.42855728381368,1.,1.519044091397));
#51920=CARTESIAN_POINT('Ctrl Pts',(-3.42852521763778,-1.,1.51896318668366));
#51921=CARTESIAN_POINT('Ctrl Pts',(-3.42852521763778,1.,1.51896318668366));
#51922=CARTESIAN_POINT('Ctrl Pts',(-3.42860527149177,-1.,1.51888450659652));
#51923=CARTESIAN_POINT('Ctrl Pts',(-3.42860527149177,1.,1.51888450659652));
#51924=CARTESIAN_POINT('Ctrl Pts',(-3.42915787669893,-1.,1.51901585839109));
#51925=CARTESIAN_POINT('Ctrl Pts',(-3.42915787669893,1.,1.51901585839109));
#51926=CARTESIAN_POINT('Ctrl Pts',(-3.43076036253837,-1.,1.51969006980999));
#51927=CARTESIAN_POINT('Ctrl Pts',(-3.43076036253837,1.,1.51969006980999));
#51928=CARTESIAN_POINT('Ctrl Pts',(-3.43417156977893,-1.,1.52134826724292));
#51929=CARTESIAN_POINT('Ctrl Pts',(-3.43417156977893,1.,1.52134826724292));
#51930=CARTESIAN_POINT('Ctrl Pts',(-3.4388889597401,-1.,1.5237734895035));
#51931=CARTESIAN_POINT('Ctrl Pts',(-3.4388889597401,1.,1.5237734895035));
#51932=CARTESIAN_POINT('Ctrl Pts',(-3.44469547526647,-1.,1.52686242875556));
#51933=CARTESIAN_POINT('Ctrl Pts',(-3.44469547526647,1.,1.52686242875556));
#51934=CARTESIAN_POINT('Ctrl Pts',(-3.45127136828305,-1.,1.53046244461635));
#51935=CARTESIAN_POINT('Ctrl Pts',(-3.45127136828305,1.,1.53046244461635));
#51936=CARTESIAN_POINT('Ctrl Pts',(-3.45825932955032,-1.,1.53440195378792));
#51937=CARTESIAN_POINT('Ctrl Pts',(-3.45825932955032,1.,1.53440195378792));
#51938=CARTESIAN_POINT('Ctrl Pts',(-3.46531752207153,-1.,1.53851507915502));
#51939=CARTESIAN_POINT('Ctrl Pts',(-3.46531752207153,1.,1.53851507915502));
#51940=CARTESIAN_POINT('Ctrl Pts',(-3.47217189224653,-1.,1.54266605398187));
#51941=CARTESIAN_POINT('Ctrl Pts',(-3.47217189224653,1.,1.54266605398187));
#51942=CARTESIAN_POINT('Ctrl Pts',(-3.47868272898751,-1.,1.54678009290276));
#51943=CARTESIAN_POINT('Ctrl Pts',(-3.47868272898751,1.,1.54678009290276));
#51944=CARTESIAN_POINT('Ctrl Pts',(-3.48485155928567,-1.,1.55084702970452));
#51945=CARTESIAN_POINT('Ctrl Pts',(-3.48485155928567,1.,1.55084702970452));
#51946=CARTESIAN_POINT('Ctrl Pts',(-3.4907646087742,-1.,1.55489595901116));
#51947=CARTESIAN_POINT('Ctrl Pts',(-3.4907646087742,1.,1.55489595901116));
#51948=CARTESIAN_POINT('Ctrl Pts',(-3.49655185179655,-1.,1.55897703097874));
#51949=CARTESIAN_POINT('Ctrl Pts',(-3.49655185179655,1.,1.55897703097874));
#51950=CARTESIAN_POINT('Ctrl Pts',(-3.50234321621578,-1.,1.56314187758675));
#51951=CARTESIAN_POINT('Ctrl Pts',(-3.50234321621578,1.,1.56314187758675));
#51952=CARTESIAN_POINT('Ctrl Pts',(-3.50821771695363,-1.,1.56742097575012));
#51953=CARTESIAN_POINT('Ctrl Pts',(-3.50821771695363,1.,1.56742097575012));
#51954=CARTESIAN_POINT('Ctrl Pts',(-3.51418598431665,-1.,1.57181569799743));
#51955=CARTESIAN_POINT('Ctrl Pts',(-3.51418598431665,1.,1.57181569799743));
#51956=CARTESIAN_POINT('Ctrl Pts',(-3.52021847865912,-1.,1.57631049988158));
#51957=CARTESIAN_POINT('Ctrl Pts',(-3.52021847865912,1.,1.57631049988158));
#51958=CARTESIAN_POINT('Ctrl Pts',(-3.52626275334881,-1.,1.58088027227848));
#51959=CARTESIAN_POINT('Ctrl Pts',(-3.52626275334881,1.,1.58088027227848));
#51960=CARTESIAN_POINT('Ctrl Pts',(-3.5322637814708,-1.,1.58549906268088));
#51961=CARTESIAN_POINT('Ctrl Pts',(-3.5322637814708,1.,1.58549906268088));
#51962=CARTESIAN_POINT('Ctrl Pts',(-3.53818616861077,-1.,1.59014958368739));
#51963=CARTESIAN_POINT('Ctrl Pts',(-3.53818616861077,1.,1.59014958368739));
#51964=CARTESIAN_POINT('Ctrl Pts',(-3.54402458182337,-1.,1.59482766949766));
#51965=CARTESIAN_POINT('Ctrl Pts',(-3.54402458182337,1.,1.59482766949766));
#51966=CARTESIAN_POINT('Ctrl Pts',(-3.54979148634454,-1.,1.59953698113457));
#51967=CARTESIAN_POINT('Ctrl Pts',(-3.54979148634454,1.,1.59953698113457));
#51968=CARTESIAN_POINT('Ctrl Pts',(-3.55550985096129,-1.,1.60428584699853));
#51969=CARTESIAN_POINT('Ctrl Pts',(-3.55550985096129,1.,1.60428584699853));
#51970=CARTESIAN_POINT('Ctrl Pts',(-3.5612043248298,-1.,1.60908344685457));
#51971=CARTESIAN_POINT('Ctrl Pts',(-3.5612043248298,1.,1.60908344685457));
#51972=CARTESIAN_POINT('Ctrl Pts',(-3.56689200468387,-1.,1.61393581747514));
#51973=CARTESIAN_POINT('Ctrl Pts',(-3.56689200468387,1.,1.61393581747514));
#51974=CARTESIAN_POINT('Ctrl Pts',(-3.57257679609806,-1.,1.61884340915404));
#51975=CARTESIAN_POINT('Ctrl Pts',(-3.57257679609806,1.,1.61884340915404));
#51976=CARTESIAN_POINT('Ctrl Pts',(-3.5782545595439,-1.,1.62380329464844));
#51977=CARTESIAN_POINT('Ctrl Pts',(-3.5782545595439,1.,1.62380329464844));
#51978=CARTESIAN_POINT('Ctrl Pts',(-3.58391625774343,-1.,1.62881051550745));
#51979=CARTESIAN_POINT('Ctrl Pts',(-3.58391625774343,1.,1.62881051550745));
#51980=CARTESIAN_POINT('Ctrl Pts',(-3.58955176627879,-1.,1.6338597145126));
#51981=CARTESIAN_POINT('Ctrl Pts',(-3.58955176627879,1.,1.6338597145126));
#51982=CARTESIAN_POINT('Ctrl Pts',(-3.59515368334893,-1.,1.63894676675352));
#51983=CARTESIAN_POINT('Ctrl Pts',(-3.59515368334893,1.,1.63894676675352));
#51984=CARTESIAN_POINT('Ctrl Pts',(-3.60072028513845,-1.,1.64407004385582));
#51985=CARTESIAN_POINT('Ctrl Pts',(-3.60072028513845,1.,1.64407004385582));
#51986=CARTESIAN_POINT('Ctrl Pts',(-3.60625346556992,-1.,1.64922952425832));
#51987=CARTESIAN_POINT('Ctrl Pts',(-3.60625346556992,1.,1.64922952425832));
#51988=CARTESIAN_POINT('Ctrl Pts',(-3.61175734965127,-1.,1.65442619244325));
#51989=CARTESIAN_POINT('Ctrl Pts',(-3.61175734965127,1.,1.65442619244325));
#51990=CARTESIAN_POINT('Ctrl Pts',(-3.61723666482456,-1.,1.65966133399186));
#51991=CARTESIAN_POINT('Ctrl Pts',(-3.61723666482456,1.,1.65966133399186));
#51992=CARTESIAN_POINT('Ctrl Pts',(-3.62269517989109,-1.,1.66493585923855));
#51993=CARTESIAN_POINT('Ctrl Pts',(-3.62269517989109,1.,1.66493585923855));
#51994=CARTESIAN_POINT('Ctrl Pts',(-3.62813422105271,-1.,1.67024966008045));
#51995=CARTESIAN_POINT('Ctrl Pts',(-3.62813422105271,1.,1.67024966008045));
#51996=CARTESIAN_POINT('Ctrl Pts',(-3.63355343201232,-1.,1.67560193613156));
#51997=CARTESIAN_POINT('Ctrl Pts',(-3.63355343201232,1.,1.67560193613156));
#51998=CARTESIAN_POINT('Ctrl Pts',(-3.63895140887462,-1.,1.68099146651586));
#51999=CARTESIAN_POINT('Ctrl Pts',(-3.63895140887462,1.,1.68099146651586));
#52000=CARTESIAN_POINT('Ctrl Pts',(-3.64432638915203,-1.,1.68641690471457));
#52001=CARTESIAN_POINT('Ctrl Pts',(-3.64432638915203,1.,1.68641690471457));
#52002=CARTESIAN_POINT('Ctrl Pts',(-3.64967689827371,-1.,1.69187705481689));
#52003=CARTESIAN_POINT('Ctrl Pts',(-3.64967689827371,1.,1.69187705481689));
#52004=CARTESIAN_POINT('Ctrl Pts',(-3.65500246526749,-1.,1.69737117722534));
#52005=CARTESIAN_POINT('Ctrl Pts',(-3.65500246526749,1.,1.69737117722534));
#52006=CARTESIAN_POINT('Ctrl Pts',(-3.66030338774847,-1.,1.70289888566873));
#52007=CARTESIAN_POINT('Ctrl Pts',(-3.66030338774847,1.,1.70289888566873));
#52008=CARTESIAN_POINT('Ctrl Pts',(-3.66558043198876,-1.,1.70846001610956));
#52009=CARTESIAN_POINT('Ctrl Pts',(-3.66558043198876,1.,1.70846001610956));
#52010=CARTESIAN_POINT('Ctrl Pts',(-3.67083454901611,-1.,1.71405450210383));
#52011=CARTESIAN_POINT('Ctrl Pts',(-3.67083454901611,1.,1.71405450210383));
#52012=CARTESIAN_POINT('Ctrl Pts',(-3.67606660374709,-1.,1.71968225581808));
#52013=CARTESIAN_POINT('Ctrl Pts',(-3.67606660374709,1.,1.71968225581808));
#52014=CARTESIAN_POINT('Ctrl Pts',(-3.68127704936579,-1.,1.72534302437056));
#52015=CARTESIAN_POINT('Ctrl Pts',(-3.68127704936579,1.,1.72534302437056));
#52016=CARTESIAN_POINT('Ctrl Pts',(-3.68646597019332,-1.,1.73103640956717));
#52017=CARTESIAN_POINT('Ctrl Pts',(-3.68646597019332,1.,1.73103640956717));
#52018=CARTESIAN_POINT('Ctrl Pts',(-3.69163322648036,-1.,1.73676193254557));
#52019=CARTESIAN_POINT('Ctrl Pts',(-3.69163322648036,1.,1.73676193254557));
#52020=CARTESIAN_POINT('Ctrl Pts',(-3.69677856910517,-1.,1.74251908492617));
#52021=CARTESIAN_POINT('Ctrl Pts',(-3.69677856910517,1.,1.74251908492617));
#52022=CARTESIAN_POINT('Ctrl Pts',(-3.7019017567335,-1.,1.74830738046057));
#52023=CARTESIAN_POINT('Ctrl Pts',(-3.7019017567335,1.,1.74830738046057));
#52024=CARTESIAN_POINT('Ctrl Pts',(-3.70700269736659,-1.,1.75412641804042));
#52025=CARTESIAN_POINT('Ctrl Pts',(-3.70700269736659,1.,1.75412641804042));
#52026=CARTESIAN_POINT('Ctrl Pts',(-3.71208146346136,-1.,1.75997588498865));
#52027=CARTESIAN_POINT('Ctrl Pts',(-3.71208146346136,1.,1.75997588498865));
#52028=CARTESIAN_POINT('Ctrl Pts',(-3.71713822377359,-1.,1.76585552124394));
#52029=CARTESIAN_POINT('Ctrl Pts',(-3.71713822377359,1.,1.76585552124394));
#52030=CARTESIAN_POINT('Ctrl Pts',(-3.72217319911254,-1.,1.77176509401761));
#52031=CARTESIAN_POINT('Ctrl Pts',(-3.72217319911254,1.,1.77176509401761));
#52032=CARTESIAN_POINT('Ctrl Pts',(-3.72718661205609,-1.,1.77770437039658));
#52033=CARTESIAN_POINT('Ctrl Pts',(-3.72718661205609,1.,1.77770437039658));
#52034=CARTESIAN_POINT('Ctrl Pts',(-3.7321786309547,-1.,1.78367308442901));
#52035=CARTESIAN_POINT('Ctrl Pts',(-3.7321786309547,1.,1.78367308442901));
#52036=CARTESIAN_POINT('Ctrl Pts',(-3.73714934730681,-1.,1.78967092823491));
#52037=CARTESIAN_POINT('Ctrl Pts',(-3.73714934730681,1.,1.78967092823491));
#52038=CARTESIAN_POINT('Ctrl Pts',(-3.74209880352445,-1.,1.79569757859422));
#52039=CARTESIAN_POINT('Ctrl Pts',(-3.74209880352445,1.,1.79569757859422));
#52040=CARTESIAN_POINT('Ctrl Pts',(-3.74702700875467,-1.,1.8017527148577));
#52041=CARTESIAN_POINT('Ctrl Pts',(-3.74702700875467,1.,1.8017527148577));
#52042=CARTESIAN_POINT('Ctrl Pts',(-3.75193395887977,-1.,1.80783603939617));
#52043=CARTESIAN_POINT('Ctrl Pts',(-3.75193395887977,1.,1.80783603939617));
#52044=CARTESIAN_POINT('Ctrl Pts',(-3.75681965683071,-1.,1.8139472983358));
#52045=CARTESIAN_POINT('Ctrl Pts',(-3.75681965683071,1.,1.8139472983358));
#52046=CARTESIAN_POINT('Ctrl Pts',(-3.76168412707948,-1.,1.82008629694091));
#52047=CARTESIAN_POINT('Ctrl Pts',(-3.76168412707948,1.,1.82008629694091));
#52048=CARTESIAN_POINT('Ctrl Pts',(-3.76652740353775,-1.,1.82625289220915));
#52049=CARTESIAN_POINT('Ctrl Pts',(-3.76652740353775,1.,1.82625289220915));
#52050=CARTESIAN_POINT('Ctrl Pts',(-3.77038509817999,-1.,1.83120816955645));
#52051=CARTESIAN_POINT('Ctrl Pts',(-3.77038509817999,1.,1.83120816955645));
#52052=CARTESIAN_POINT('Ctrl Pts',(-3.77326886064398,-1.,1.83493697934534));
#52053=CARTESIAN_POINT('Ctrl Pts',(-3.77326886064398,1.,1.83493697934534));
#52054=CARTESIAN_POINT('Ctrl Pts',(-3.77518714457833,-1.,1.83742834010626));
#52055=CARTESIAN_POINT('Ctrl Pts',(-3.77518714457833,1.,1.83742834010626));
#52056=CARTESIAN_POINT('Ctrl Pts',(-3.77614523045147,-1.,1.8386753923786));
#52057=CARTESIAN_POINT('Ctrl Pts',(-3.77614523045147,1.,1.8386753923786));
#52058=CARTESIAN_POINT('',(-3.42859860294306,1.,1.5189508286633));
#52059=CARTESIAN_POINT('Ctrl Pts',(-3.42859860294306,-1.,1.5189508286633));
#52060=CARTESIAN_POINT('Ctrl Pts',(-3.42859860294306,-0.666666666666667,
1.5189508286633));
#52061=CARTESIAN_POINT('Ctrl Pts',(-3.42859860294306,-0.333333333333333,
1.5189508286633));
#52062=CARTESIAN_POINT('Ctrl Pts',(-3.42859860294306,0.333333333333333,
1.5189508286633));
#52063=CARTESIAN_POINT('Ctrl Pts',(-3.42859860294306,0.666666666666667,
1.5189508286633));
#52064=CARTESIAN_POINT('Ctrl Pts',(-3.42859860294306,1.,1.5189508286633));
#52065=CARTESIAN_POINT('',(-3.77614523045147,1.,1.8386753923786));
#52066=CARTESIAN_POINT('',(-3.77614523045147,0.,1.8386753923786));
#52067=CARTESIAN_POINT('Ctrl Pts',(-3.42859860294306,1.,1.5189508286633));
#52068=CARTESIAN_POINT('Ctrl Pts',(-3.42864616361875,1.,1.51893924967331));
#52069=CARTESIAN_POINT('Ctrl Pts',(-3.42884302333841,1.,1.5189513329503));
#52070=CARTESIAN_POINT('Ctrl Pts',(-3.42946838852587,1.,1.51914806898491));
#52071=CARTESIAN_POINT('Ctrl Pts',(-3.43101631893414,1.,1.5198144909338));
#52072=CARTESIAN_POINT('Ctrl Pts',(-3.43417156977893,1.,1.52134826724292));
#52073=CARTESIAN_POINT('Ctrl Pts',(-3.4388889597401,1.,1.5237734895035));
#52074=CARTESIAN_POINT('Ctrl Pts',(-3.44469547526647,1.,1.52686242875556));
#52075=CARTESIAN_POINT('Ctrl Pts',(-3.45127136828305,1.,1.53046244461635));
#52076=CARTESIAN_POINT('Ctrl Pts',(-3.45825932955032,1.,1.53440195378792));
#52077=CARTESIAN_POINT('Ctrl Pts',(-3.46531752207153,1.,1.53851507915502));
#52078=CARTESIAN_POINT('Ctrl Pts',(-3.47217189224653,1.,1.54266605398187));
#52079=CARTESIAN_POINT('Ctrl Pts',(-3.47868272898751,1.,1.54678009290276));
#52080=CARTESIAN_POINT('Ctrl Pts',(-3.48485155928567,1.,1.55084702970452));
#52081=CARTESIAN_POINT('Ctrl Pts',(-3.4907646087742,1.,1.55489595901116));
#52082=CARTESIAN_POINT('Ctrl Pts',(-3.49655185179655,1.,1.55897703097874));
#52083=CARTESIAN_POINT('Ctrl Pts',(-3.50234321621578,1.,1.56314187758675));
#52084=CARTESIAN_POINT('Ctrl Pts',(-3.50821771695363,1.,1.56742097575012));
#52085=CARTESIAN_POINT('Ctrl Pts',(-3.51418598431665,1.,1.57181569799743));
#52086=CARTESIAN_POINT('Ctrl Pts',(-3.52021847865912,1.,1.57631049988158));
#52087=CARTESIAN_POINT('Ctrl Pts',(-3.52626275334881,1.,1.58088027227848));
#52088=CARTESIAN_POINT('Ctrl Pts',(-3.5322637814708,1.,1.58549906268088));
#52089=CARTESIAN_POINT('Ctrl Pts',(-3.53818616861077,1.,1.59014958368739));
#52090=CARTESIAN_POINT('Ctrl Pts',(-3.54402458182337,1.,1.59482766949766));
#52091=CARTESIAN_POINT('Ctrl Pts',(-3.54979148634454,1.,1.59953698113457));
#52092=CARTESIAN_POINT('Ctrl Pts',(-3.55550985096129,1.,1.60428584699853));
#52093=CARTESIAN_POINT('Ctrl Pts',(-3.5612043248298,1.,1.60908344685457));
#52094=CARTESIAN_POINT('Ctrl Pts',(-3.56689200468387,1.,1.61393581747514));
#52095=CARTESIAN_POINT('Ctrl Pts',(-3.57257679609806,1.,1.61884340915404));
#52096=CARTESIAN_POINT('Ctrl Pts',(-3.5782545595439,1.,1.62380329464844));
#52097=CARTESIAN_POINT('Ctrl Pts',(-3.58391625774343,1.,1.62881051550745));
#52098=CARTESIAN_POINT('Ctrl Pts',(-3.58955176627879,1.,1.6338597145126));
#52099=CARTESIAN_POINT('Ctrl Pts',(-3.59515368334893,1.,1.63894676675352));
#52100=CARTESIAN_POINT('Ctrl Pts',(-3.60072028513845,1.,1.64407004385582));
#52101=CARTESIAN_POINT('Ctrl Pts',(-3.60625346556992,1.,1.64922952425832));
#52102=CARTESIAN_POINT('Ctrl Pts',(-3.61175734965127,1.,1.65442619244325));
#52103=CARTESIAN_POINT('Ctrl Pts',(-3.61723666482456,1.,1.65966133399186));
#52104=CARTESIAN_POINT('Ctrl Pts',(-3.62269517989109,1.,1.66493585923855));
#52105=CARTESIAN_POINT('Ctrl Pts',(-3.62813422105271,1.,1.67024966008045));
#52106=CARTESIAN_POINT('Ctrl Pts',(-3.63355343201232,1.,1.67560193613156));
#52107=CARTESIAN_POINT('Ctrl Pts',(-3.63895140887462,1.,1.68099146651586));
#52108=CARTESIAN_POINT('Ctrl Pts',(-3.64432638915203,1.,1.68641690471457));
#52109=CARTESIAN_POINT('Ctrl Pts',(-3.64967689827371,1.,1.69187705481689));
#52110=CARTESIAN_POINT('Ctrl Pts',(-3.65500246526749,1.,1.69737117722534));
#52111=CARTESIAN_POINT('Ctrl Pts',(-3.66030338774847,1.,1.70289888566873));
#52112=CARTESIAN_POINT('Ctrl Pts',(-3.66558043198876,1.,1.70846001610956));
#52113=CARTESIAN_POINT('Ctrl Pts',(-3.67083454901611,1.,1.71405450210383));
#52114=CARTESIAN_POINT('Ctrl Pts',(-3.67606660374709,1.,1.71968225581808));
#52115=CARTESIAN_POINT('Ctrl Pts',(-3.68127704936579,1.,1.72534302437056));
#52116=CARTESIAN_POINT('Ctrl Pts',(-3.68646597019332,1.,1.73103640956717));
#52117=CARTESIAN_POINT('Ctrl Pts',(-3.69163322648036,1.,1.73676193254557));
#52118=CARTESIAN_POINT('Ctrl Pts',(-3.69677856910517,1.,1.74251908492617));
#52119=CARTESIAN_POINT('Ctrl Pts',(-3.7019017567335,1.,1.74830738046057));
#52120=CARTESIAN_POINT('Ctrl Pts',(-3.70700269736659,1.,1.75412641804042));
#52121=CARTESIAN_POINT('Ctrl Pts',(-3.71208146346136,1.,1.75997588498865));
#52122=CARTESIAN_POINT('Ctrl Pts',(-3.71713822377359,1.,1.76585552124394));
#52123=CARTESIAN_POINT('Ctrl Pts',(-3.72217319911254,1.,1.77176509401761));
#52124=CARTESIAN_POINT('Ctrl Pts',(-3.72718661205609,1.,1.77770437039658));
#52125=CARTESIAN_POINT('Ctrl Pts',(-3.7321786309547,1.,1.78367308442901));
#52126=CARTESIAN_POINT('Ctrl Pts',(-3.73714934730681,1.,1.78967092823491));
#52127=CARTESIAN_POINT('Ctrl Pts',(-3.74209880352445,1.,1.79569757859422));
#52128=CARTESIAN_POINT('Ctrl Pts',(-3.74702700875467,1.,1.8017527148577));
#52129=CARTESIAN_POINT('Ctrl Pts',(-3.75193395887977,1.,1.80783603939617));
#52130=CARTESIAN_POINT('Ctrl Pts',(-3.75681965683071,1.,1.8139472983358));
#52131=CARTESIAN_POINT('Ctrl Pts',(-3.76168412707948,1.,1.82008629694091));
#52132=CARTESIAN_POINT('Ctrl Pts',(-3.76652740353775,1.,1.82625289220915));
#52133=CARTESIAN_POINT('Ctrl Pts',(-3.77038509817999,1.,1.83120816955645));
#52134=CARTESIAN_POINT('Ctrl Pts',(-3.77326886064398,1.,1.83493697934534));
#52135=CARTESIAN_POINT('Ctrl Pts',(-3.77518714457833,1.,1.83742834010626));
#52136=CARTESIAN_POINT('Ctrl Pts',(-3.77614523045147,1.,1.8386753923786));
#52137=CARTESIAN_POINT('Origin',(-3.77614523045147,0.,1.8386753923786));
#52138=CARTESIAN_POINT('',(-3.70708211654725,1.,1.97421938526992));
#52139=CARTESIAN_POINT('Origin',(0.,0.,0.));
#52140=CARTESIAN_POINT('',(-3.49844575334386,1.,1.35032489087269));
#52141=CARTESIAN_POINT('Origin',(0.,1.,0.));
#52142=CARTESIAN_POINT('Ctrl Pts',(-3.49844575334386,1.,1.35032489087269));
#52143=CARTESIAN_POINT('Ctrl Pts',(-3.49844575334386,0.666666666666667,
1.35032489087269));
#52144=CARTESIAN_POINT('Ctrl Pts',(-3.49844575334386,0.333333333333333,
1.35032489087269));
#52145=CARTESIAN_POINT('Ctrl Pts',(-3.49844575334386,-0.333333333333333,
1.35032489087269));
#52146=CARTESIAN_POINT('Ctrl Pts',(-3.49844575334386,-0.666666666666667,
1.35032489087269));
#52147=CARTESIAN_POINT('Ctrl Pts',(-3.49844575334386,-1.,1.35032489087269));
#52148=CARTESIAN_POINT('Ctrl Pts',(-3.97027773754922,-1.,1.36999806084572));
#52149=CARTESIAN_POINT('Ctrl Pts',(-3.97027773754922,1.,1.36999806084572));
#52150=CARTESIAN_POINT('Ctrl Pts',(-3.9687184694173,-1.,1.37020239094758));
#52151=CARTESIAN_POINT('Ctrl Pts',(-3.9687184694173,1.,1.37020239094758));
#52152=CARTESIAN_POINT('Ctrl Pts',(-3.96560037975788,-1.,1.37060761746027));
#52153=CARTESIAN_POINT('Ctrl Pts',(-3.96560037975788,1.,1.37060761746027));
#52154=CARTESIAN_POINT('Ctrl Pts',(-3.96092458508407,-1.,1.37120515615663));
#52155=CARTESIAN_POINT('Ctrl Pts',(-3.96092458508407,1.,1.37120515615663));
#52156=CARTESIAN_POINT('Ctrl Pts',(-3.95469287283105,-1.,1.37198126433139));
#52157=CARTESIAN_POINT('Ctrl Pts',(-3.95469287283105,1.,1.37198126433139));
#52158=CARTESIAN_POINT('Ctrl Pts',(-3.94690771786926,-1.,1.37291699203423));
#52159=CARTESIAN_POINT('Ctrl Pts',(-3.94690771786926,1.,1.37291699203423));
#52160=CARTESIAN_POINT('Ctrl Pts',(-3.93912709041791,-1.,1.37381821967499));
#52161=CARTESIAN_POINT('Ctrl Pts',(-3.93912709041791,1.,1.37381821967499));
#52162=CARTESIAN_POINT('Ctrl Pts',(-3.93135106761941,-1.,1.37468482215784));
#52163=CARTESIAN_POINT('Ctrl Pts',(-3.93135106761941,1.,1.37468482215784));
#52164=CARTESIAN_POINT('Ctrl Pts',(-3.92357976987132,-1.,1.37551664448057));
#52165=CARTESIAN_POINT('Ctrl Pts',(-3.92357976987132,1.,1.37551664448057));
#52166=CARTESIAN_POINT('Ctrl Pts',(-3.91581337461825,-1.,1.37631350505516));
#52167=CARTESIAN_POINT('Ctrl Pts',(-3.91581337461825,1.,1.37631350505516));
#52168=CARTESIAN_POINT('Ctrl Pts',(-3.90805209522729,-1.,1.3770751963376));
#52169=CARTESIAN_POINT('Ctrl Pts',(-3.90805209522729,1.,1.3770751963376));
#52170=CARTESIAN_POINT('Ctrl Pts',(-3.90029615196255,-1.,1.3778014851263));
#52171=CARTESIAN_POINT('Ctrl Pts',(-3.90029615196255,1.,1.3778014851263));
#52172=CARTESIAN_POINT('Ctrl Pts',(-3.89254574338385,-1.,1.37849211287981));
#52173=CARTESIAN_POINT('Ctrl Pts',(-3.89254574338385,1.,1.37849211287981));
#52174=CARTESIAN_POINT('Ctrl Pts',(-3.88480102249461,-1.,1.37914679719446));
#52175=CARTESIAN_POINT('Ctrl Pts',(-3.88480102249461,1.,1.37914679719446));
#52176=CARTESIAN_POINT('Ctrl Pts',(-3.87706205830865,-1.,1.37976523097187));
#52177=CARTESIAN_POINT('Ctrl Pts',(-3.87706205830865,1.,1.37976523097187));
#52178=CARTESIAN_POINT('Ctrl Pts',(-3.86932885813403,-1.,1.38034709213129));
#52179=CARTESIAN_POINT('Ctrl Pts',(-3.86932885813403,1.,1.38034709213129));
#52180=CARTESIAN_POINT('Ctrl Pts',(-3.86160143044187,-1.,1.38089205993067));
#52181=CARTESIAN_POINT('Ctrl Pts',(-3.86160143044187,1.,1.38089205993067));
#52182=CARTESIAN_POINT('Ctrl Pts',(-3.85387983979557,-1.,1.38139983115075));
#52183=CARTESIAN_POINT('Ctrl Pts',(-3.85387983979557,1.,1.38139983115075));
#52184=CARTESIAN_POINT('Ctrl Pts',(-3.84616425605705,-1.,1.38187013346089));
#52185=CARTESIAN_POINT('Ctrl Pts',(-3.84616425605705,1.,1.38187013346089));
#52186=CARTESIAN_POINT('Ctrl Pts',(-3.83845502790609,-1.,1.38230274828774));
#52187=CARTESIAN_POINT('Ctrl Pts',(-3.83845502790609,1.,1.38230274828774));
#52188=CARTESIAN_POINT('Ctrl Pts',(-3.83075266982138,-1.,1.38269750245086));
#52189=CARTESIAN_POINT('Ctrl Pts',(-3.83075266982138,1.,1.38269750245086));
#52190=CARTESIAN_POINT('Ctrl Pts',(-3.82305771743715,-1.,1.38305421262724));
#52191=CARTESIAN_POINT('Ctrl Pts',(-3.82305771743715,1.,1.38305421262724));
#52192=CARTESIAN_POINT('Ctrl Pts',(-3.81537060817765,-1.,1.38337263902766));
#52193=CARTESIAN_POINT('Ctrl Pts',(-3.81537060817765,1.,1.38337263902766));
#52194=CARTESIAN_POINT('Ctrl Pts',(-3.80769156398429,-1.,1.38365244046226));
#52195=CARTESIAN_POINT('Ctrl Pts',(-3.80769156398429,1.,1.38365244046226));
#52196=CARTESIAN_POINT('Ctrl Pts',(-3.80002044322169,-1.,1.38389311766701));
#52197=CARTESIAN_POINT('Ctrl Pts',(-3.80002044322169,1.,1.38389311766701));
#52198=CARTESIAN_POINT('Ctrl Pts',(-3.79235669640907,-1.,1.38409399694588));
#52199=CARTESIAN_POINT('Ctrl Pts',(-3.79235669640907,1.,1.38409399694588));
#52200=CARTESIAN_POINT('Ctrl Pts',(-3.78469969805134,-1.,1.38425435883773));
#52201=CARTESIAN_POINT('Ctrl Pts',(-3.78469969805134,1.,1.38425435883773));
#52202=CARTESIAN_POINT('Ctrl Pts',(-3.77704902230441,-1.,1.38437354551435));
#52203=CARTESIAN_POINT('Ctrl Pts',(-3.77704902230441,1.,1.38437354551435));
#52204=CARTESIAN_POINT('Ctrl Pts',(-3.76940473185775,-1.,1.38445107339517));
#52205=CARTESIAN_POINT('Ctrl Pts',(-3.76940473185775,1.,1.38445107339517));
#52206=CARTESIAN_POINT('Ctrl Pts',(-3.76176768271347,-1.,1.38448675253343));
#52207=CARTESIAN_POINT('Ctrl Pts',(-3.76176768271347,1.,1.38448675253343));
#52208=CARTESIAN_POINT('Ctrl Pts',(-3.75413976318727,-1.,1.38448077997155));
#52209=CARTESIAN_POINT('Ctrl Pts',(-3.75413976318727,1.,1.38448077997155));
#52210=CARTESIAN_POINT('Ctrl Pts',(-3.7465231716786,-1.,1.38443344984389));
#52211=CARTESIAN_POINT('Ctrl Pts',(-3.7465231716786,1.,1.38443344984389));
#52212=CARTESIAN_POINT('Ctrl Pts',(-3.73891976418099,-1.,1.38434489156456));
#52213=CARTESIAN_POINT('Ctrl Pts',(-3.73891976418099,1.,1.38434489156456));
#52214=CARTESIAN_POINT('Ctrl Pts',(-3.73133035859283,-1.,1.38421479111531));
#52215=CARTESIAN_POINT('Ctrl Pts',(-3.73133035859283,1.,1.38421479111531));
#52216=CARTESIAN_POINT('Ctrl Pts',(-3.72375409358805,-1.,1.3840421342895));
#52217=CARTESIAN_POINT('Ctrl Pts',(-3.72375409358805,1.,1.3840421342895));
#52218=CARTESIAN_POINT('Ctrl Pts',(-3.7161876605181,-1.,1.38382489984585));
#52219=CARTESIAN_POINT('Ctrl Pts',(-3.7161876605181,1.,1.38382489984585));
#52220=CARTESIAN_POINT('Ctrl Pts',(-3.70862680753343,-1.,1.38356065402122));
#52221=CARTESIAN_POINT('Ctrl Pts',(-3.70862680753343,1.,1.38356065402122));
#52222=CARTESIAN_POINT('Ctrl Pts',(-3.70106792167894,-1.,1.38324717612862));
#52223=CARTESIAN_POINT('Ctrl Pts',(-3.70106792167894,1.,1.38324717612862));
#52224=CARTESIAN_POINT('Ctrl Pts',(-3.69350967899523,-1.,1.38288311171649));
#52225=CARTESIAN_POINT('Ctrl Pts',(-3.69350967899523,1.,1.38288311171649));
#52226=CARTESIAN_POINT('Ctrl Pts',(-3.68595444983844,-1.,1.38246852827185));
#52227=CARTESIAN_POINT('Ctrl Pts',(-3.68595444983844,1.,1.38246852827185));
#52228=CARTESIAN_POINT('Ctrl Pts',(-3.6784103848243,-1.,1.38200574290626));
#52229=CARTESIAN_POINT('Ctrl Pts',(-3.6784103848243,1.,1.38200574290626));
#52230=CARTESIAN_POINT('Ctrl Pts',(-3.67088843112282,-1.,1.38149812653876));
#52231=CARTESIAN_POINT('Ctrl Pts',(-3.67088843112282,1.,1.38149812653876));
#52232=CARTESIAN_POINT('Ctrl Pts',(-3.66339848520874,-1.,1.38094856333558));
#52233=CARTESIAN_POINT('Ctrl Pts',(-3.66339848520874,1.,1.38094856333558));
#52234=CARTESIAN_POINT('Ctrl Pts',(-3.65594554404396,-1.,1.38035791051215));
#52235=CARTESIAN_POINT('Ctrl Pts',(-3.65594554404396,1.,1.38035791051215));
#52236=CARTESIAN_POINT('Ctrl Pts',(-3.64852652756444,-1.,1.37972372481598));
#52237=CARTESIAN_POINT('Ctrl Pts',(-3.64852652756444,1.,1.37972372481598));
#52238=CARTESIAN_POINT('Ctrl Pts',(-3.64112507791112,-1.,1.37903818567347));
#52239=CARTESIAN_POINT('Ctrl Pts',(-3.64112507791112,1.,1.37903818567347));
#52240=CARTESIAN_POINT('Ctrl Pts',(-3.63371727442448,-1.,1.37829035457324));
#52241=CARTESIAN_POINT('Ctrl Pts',(-3.63371727442448,1.,1.37829035457324));
#52242=CARTESIAN_POINT('Ctrl Pts',(-3.62628098665112,-1.,1.37746987919868));
#52243=CARTESIAN_POINT('Ctrl Pts',(-3.62628098665112,1.,1.37746987919868));
#52244=CARTESIAN_POINT('Ctrl Pts',(-3.61880481160408,-1.,1.37657053403102));
#52245=CARTESIAN_POINT('Ctrl Pts',(-3.61880481160408,1.,1.37657053403102));
#52246=CARTESIAN_POINT('Ctrl Pts',(-3.61129546591082,-1.,1.37559314436641));
#52247=CARTESIAN_POINT('Ctrl Pts',(-3.61129546591082,1.,1.37559314436641));
#52248=CARTESIAN_POINT('Ctrl Pts',(-3.60379020124038,-1.,1.37455051379642));
#52249=CARTESIAN_POINT('Ctrl Pts',(-3.60379020124038,1.,1.37455051379642));
#52250=CARTESIAN_POINT('Ctrl Pts',(-3.59634627869117,-1.,1.37346320103184));
#52251=CARTESIAN_POINT('Ctrl Pts',(-3.59634627869117,1.,1.37346320103184));
#52252=CARTESIAN_POINT('Ctrl Pts',(-3.5890185384643,-1.,1.37235053661));
#52253=CARTESIAN_POINT('Ctrl Pts',(-3.5890185384643,1.,1.37235053661));
#52254=CARTESIAN_POINT('Ctrl Pts',(-3.58183885982745,-1.,1.37122241663073));
#52255=CARTESIAN_POINT('Ctrl Pts',(-3.58183885982745,1.,1.37122241663073));
#52256=CARTESIAN_POINT('Ctrl Pts',(-3.57479875549453,-1.,1.37007229485646));
#52257=CARTESIAN_POINT('Ctrl Pts',(-3.57479875549453,1.,1.37007229485646));
#52258=CARTESIAN_POINT('Ctrl Pts',(-3.56782080304554,-1.,1.36886584973349));
#52259=CARTESIAN_POINT('Ctrl Pts',(-3.56782080304554,1.,1.36886584973349));
#52260=CARTESIAN_POINT('Ctrl Pts',(-3.56077662028492,-1.,1.36754771771174));
#52261=CARTESIAN_POINT('Ctrl Pts',(-3.56077662028492,1.,1.36754771771174));
#52262=CARTESIAN_POINT('Ctrl Pts',(-3.55353883995793,-1.,1.36606145456711));
#52263=CARTESIAN_POINT('Ctrl Pts',(-3.55353883995793,1.,1.36606145456711));
#52264=CARTESIAN_POINT('Ctrl Pts',(-3.54602591832893,-1.,1.36436666257567));
#52265=CARTESIAN_POINT('Ctrl Pts',(-3.54602591832893,1.,1.36436666257567));
#52266=CARTESIAN_POINT('Ctrl Pts',(-3.53824396425032,-1.,1.36245507339334));
#52267=CARTESIAN_POINT('Ctrl Pts',(-3.53824396425032,1.,1.36245507339334));
#52268=CARTESIAN_POINT('Ctrl Pts',(-3.53034464961849,-1.,1.36037259643827));
#52269=CARTESIAN_POINT('Ctrl Pts',(-3.53034464961849,1.,1.36037259643827));
#52270=CARTESIAN_POINT('Ctrl Pts',(-3.52261776117121,-1.,1.35821701528975));
#52271=CARTESIAN_POINT('Ctrl Pts',(-3.52261776117121,1.,1.35821701528975));
#52272=CARTESIAN_POINT('Ctrl Pts',(-3.51542230699919,-1.,1.35611275237288));
#52273=CARTESIAN_POINT('Ctrl Pts',(-3.51542230699919,1.,1.35611275237288));
#52274=CARTESIAN_POINT('Ctrl Pts',(-3.50913227060177,-1.,1.35419113576022));
#52275=CARTESIAN_POINT('Ctrl Pts',(-3.50913227060177,1.,1.35419113576022));
#52276=CARTESIAN_POINT('Ctrl Pts',(-3.50408168106113,-1.,1.3525703284343));
#52277=CARTESIAN_POINT('Ctrl Pts',(-3.50408168106113,1.,1.3525703284343));
#52278=CARTESIAN_POINT('Ctrl Pts',(-3.50049707063673,-1.,1.35133076331065));
#52279=CARTESIAN_POINT('Ctrl Pts',(-3.50049707063673,1.,1.35133076331065));
#52280=CARTESIAN_POINT('Ctrl Pts',(-3.49888720256612,-1.,1.35067437417289));
#52281=CARTESIAN_POINT('Ctrl Pts',(-3.49888720256612,1.,1.35067437417289));
#52282=CARTESIAN_POINT('Ctrl Pts',(-3.49840357193384,-1.,1.35037650302887));
#52283=CARTESIAN_POINT('Ctrl Pts',(-3.49840357193384,1.,1.35037650302887));
#52284=CARTESIAN_POINT('Ctrl Pts',(-3.49840260053616,-1.,1.35026426118351));
#52285=CARTESIAN_POINT('Ctrl Pts',(-3.49840260053616,1.,1.35026426118351));
#52286=CARTESIAN_POINT('Ctrl Pts',(-3.49848248301936,-1.,1.35022972712301));
#52287=CARTESIAN_POINT('Ctrl Pts',(-3.49848248301936,1.,1.35022972712301));
#52288=CARTESIAN_POINT('',(-3.97027773754922,1.,1.36999806084572));
#52289=CARTESIAN_POINT('Ctrl Pts',(-3.97027773754922,1.,1.36999806084572));
#52290=CARTESIAN_POINT('Ctrl Pts',(-3.9687184694173,1.,1.37020239094758));
#52291=CARTESIAN_POINT('Ctrl Pts',(-3.96560037975788,1.,1.37060761746027));
#52292=CARTESIAN_POINT('Ctrl Pts',(-3.96092458508407,1.,1.37120515615663));
#52293=CARTESIAN_POINT('Ctrl Pts',(-3.95469287283105,1.,1.37198126433139));
#52294=CARTESIAN_POINT('Ctrl Pts',(-3.94690771786926,1.,1.37291699203423));
#52295=CARTESIAN_POINT('Ctrl Pts',(-3.93912709041791,1.,1.37381821967499));
#52296=CARTESIAN_POINT('Ctrl Pts',(-3.93135106761941,1.,1.37468482215784));
#52297=CARTESIAN_POINT('Ctrl Pts',(-3.92357976987132,1.,1.37551664448057));
#52298=CARTESIAN_POINT('Ctrl Pts',(-3.91581337461825,1.,1.37631350505516));
#52299=CARTESIAN_POINT('Ctrl Pts',(-3.90805209522729,1.,1.3770751963376));
#52300=CARTESIAN_POINT('Ctrl Pts',(-3.90029615196255,1.,1.3778014851263));
#52301=CARTESIAN_POINT('Ctrl Pts',(-3.89254574338385,1.,1.37849211287981));
#52302=CARTESIAN_POINT('Ctrl Pts',(-3.88480102249461,1.,1.37914679719446));
#52303=CARTESIAN_POINT('Ctrl Pts',(-3.87706205830865,1.,1.37976523097187));
#52304=CARTESIAN_POINT('Ctrl Pts',(-3.86932885813403,1.,1.38034709213129));
#52305=CARTESIAN_POINT('Ctrl Pts',(-3.86160143044187,1.,1.38089205993067));
#52306=CARTESIAN_POINT('Ctrl Pts',(-3.85387983979557,1.,1.38139983115075));
#52307=CARTESIAN_POINT('Ctrl Pts',(-3.84616425605705,1.,1.38187013346089));
#52308=CARTESIAN_POINT('Ctrl Pts',(-3.83845502790609,1.,1.38230274828774));
#52309=CARTESIAN_POINT('Ctrl Pts',(-3.83075266982138,1.,1.38269750245086));
#52310=CARTESIAN_POINT('Ctrl Pts',(-3.82305771743715,1.,1.38305421262724));
#52311=CARTESIAN_POINT('Ctrl Pts',(-3.81537060817765,1.,1.38337263902766));
#52312=CARTESIAN_POINT('Ctrl Pts',(-3.80769156398429,1.,1.38365244046226));
#52313=CARTESIAN_POINT('Ctrl Pts',(-3.80002044322169,1.,1.38389311766701));
#52314=CARTESIAN_POINT('Ctrl Pts',(-3.79235669640907,1.,1.38409399694588));
#52315=CARTESIAN_POINT('Ctrl Pts',(-3.78469969805134,1.,1.38425435883773));
#52316=CARTESIAN_POINT('Ctrl Pts',(-3.77704902230441,1.,1.38437354551435));
#52317=CARTESIAN_POINT('Ctrl Pts',(-3.76940473185775,1.,1.38445107339517));
#52318=CARTESIAN_POINT('Ctrl Pts',(-3.76176768271347,1.,1.38448675253343));
#52319=CARTESIAN_POINT('Ctrl Pts',(-3.75413976318727,1.,1.38448077997155));
#52320=CARTESIAN_POINT('Ctrl Pts',(-3.7465231716786,1.,1.38443344984389));
#52321=CARTESIAN_POINT('Ctrl Pts',(-3.73891976418099,1.,1.38434489156456));
#52322=CARTESIAN_POINT('Ctrl Pts',(-3.73133035859283,1.,1.38421479111531));
#52323=CARTESIAN_POINT('Ctrl Pts',(-3.72375409358805,1.,1.3840421342895));
#52324=CARTESIAN_POINT('Ctrl Pts',(-3.7161876605181,1.,1.38382489984585));
#52325=CARTESIAN_POINT('Ctrl Pts',(-3.70862680753343,1.,1.38356065402122));
#52326=CARTESIAN_POINT('Ctrl Pts',(-3.70106792167894,1.,1.38324717612862));
#52327=CARTESIAN_POINT('Ctrl Pts',(-3.69350967899523,1.,1.38288311171649));
#52328=CARTESIAN_POINT('Ctrl Pts',(-3.68595444983844,1.,1.38246852827185));
#52329=CARTESIAN_POINT('Ctrl Pts',(-3.6784103848243,1.,1.38200574290626));
#52330=CARTESIAN_POINT('Ctrl Pts',(-3.67088843112282,1.,1.38149812653876));
#52331=CARTESIAN_POINT('Ctrl Pts',(-3.66339848520874,1.,1.38094856333558));
#52332=CARTESIAN_POINT('Ctrl Pts',(-3.65594554404396,1.,1.38035791051215));
#52333=CARTESIAN_POINT('Ctrl Pts',(-3.64852652756444,1.,1.37972372481598));
#52334=CARTESIAN_POINT('Ctrl Pts',(-3.64112507791112,1.,1.37903818567347));
#52335=CARTESIAN_POINT('Ctrl Pts',(-3.63371727442448,1.,1.37829035457324));
#52336=CARTESIAN_POINT('Ctrl Pts',(-3.62628098665112,1.,1.37746987919868));
#52337=CARTESIAN_POINT('Ctrl Pts',(-3.61880481160408,1.,1.37657053403102));
#52338=CARTESIAN_POINT('Ctrl Pts',(-3.61129546591082,1.,1.37559314436641));
#52339=CARTESIAN_POINT('Ctrl Pts',(-3.60379020124038,1.,1.37455051379642));
#52340=CARTESIAN_POINT('Ctrl Pts',(-3.59634627869117,1.,1.37346320103184));
#52341=CARTESIAN_POINT('Ctrl Pts',(-3.5890185384643,1.,1.37235053661));
#52342=CARTESIAN_POINT('Ctrl Pts',(-3.58183885982745,1.,1.37122241663073));
#52343=CARTESIAN_POINT('Ctrl Pts',(-3.57479875549453,1.,1.37007229485646));
#52344=CARTESIAN_POINT('Ctrl Pts',(-3.56782080304554,1.,1.36886584973349));
#52345=CARTESIAN_POINT('Ctrl Pts',(-3.56077662028492,1.,1.36754771771174));
#52346=CARTESIAN_POINT('Ctrl Pts',(-3.55353883995793,1.,1.36606145456711));
#52347=CARTESIAN_POINT('Ctrl Pts',(-3.54602591832893,1.,1.36436666257567));
#52348=CARTESIAN_POINT('Ctrl Pts',(-3.53824396425032,1.,1.36245507339334));
#52349=CARTESIAN_POINT('Ctrl Pts',(-3.53034464961849,1.,1.36037259643827));
#52350=CARTESIAN_POINT('Ctrl Pts',(-3.52261776117121,1.,1.35821701528975));
#52351=CARTESIAN_POINT('Ctrl Pts',(-3.51542230699919,1.,1.35611275237288));
#52352=CARTESIAN_POINT('Ctrl Pts',(-3.50913227060177,1.,1.35419113576022));
#52353=CARTESIAN_POINT('Ctrl Pts',(-3.50408168106113,1.,1.3525703284343));
#52354=CARTESIAN_POINT('Ctrl Pts',(-3.5007660381658,1.,1.35142377279535));
#52355=CARTESIAN_POINT('Ctrl Pts',(-3.49920025459856,1.,1.35080045218652));
#52356=CARTESIAN_POINT('Ctrl Pts',(-3.49861894124915,1.,1.35049736560633));
#52357=CARTESIAN_POINT('Ctrl Pts',(-3.49847119623841,1.,1.35036670893102));
#52358=CARTESIAN_POINT('Ctrl Pts',(-3.49844575334386,1.,1.35032489087269));
#52359=CARTESIAN_POINT('',(-3.97027773754922,0.,1.36999806084572));
#52360=CARTESIAN_POINT('Ctrl Pts',(-3.62397690409552,-1.,0.96399761336957));
#52361=CARTESIAN_POINT('Ctrl Pts',(-3.62397690409552,1.,0.96399761336957));
#52362=CARTESIAN_POINT('Ctrl Pts',(-3.62393257642191,-1.,0.963922720982576));
#52363=CARTESIAN_POINT('Ctrl Pts',(-3.62393257642191,1.,0.963922720982576));
#52364=CARTESIAN_POINT('Ctrl Pts',(-3.62399933640277,-1.,0.963832486396055));
#52365=CARTESIAN_POINT('Ctrl Pts',(-3.62399933640277,1.,0.963832486396055));
#52366=CARTESIAN_POINT('Ctrl Pts',(-3.62456568607055,-1.,0.963875774532102));
#52367=CARTESIAN_POINT('Ctrl Pts',(-3.62456568607055,1.,0.963875774532102));
#52368=CARTESIAN_POINT('Ctrl Pts',(-3.62625391255277,-1.,0.964291001274618));
#52369=CARTESIAN_POINT('Ctrl Pts',(-3.62625391255277,1.,0.964291001274618));
#52370=CARTESIAN_POINT('Ctrl Pts',(-3.62988252139998,-1.,0.965395153165716));
#52371=CARTESIAN_POINT('Ctrl Pts',(-3.62988252139998,1.,0.965395153165716));
#52372=CARTESIAN_POINT('Ctrl Pts',(-3.6349212208096,-1.,0.967052554540877));
#52373=CARTESIAN_POINT('Ctrl Pts',(-3.6349212208096,1.,0.967052554540877));
#52374=CARTESIAN_POINT('Ctrl Pts',(-3.64113946505393,-1.,0.969195124674829));
#52375=CARTESIAN_POINT('Ctrl Pts',(-3.64113946505393,1.,0.969195124674829));
#52376=CARTESIAN_POINT('Ctrl Pts',(-3.64819756447072,-1.,0.971722122060277));
#52377=CARTESIAN_POINT('Ctrl Pts',(-3.64819756447072,1.,0.971722122060277));
#52378=CARTESIAN_POINT('Ctrl Pts',(-3.6557157673487,-1.,0.974519971354138));
#52379=CARTESIAN_POINT('Ctrl Pts',(-3.6557157673487,1.,0.974519971354138));
#52380=CARTESIAN_POINT('Ctrl Pts',(-3.66333049637403,-1.,0.977478312751416));
#52381=CARTESIAN_POINT('Ctrl Pts',(-3.66333049637403,1.,0.977478312751416));
#52382=CARTESIAN_POINT('Ctrl Pts',(-3.67074983340444,-1.,0.980505922458494));
#52383=CARTESIAN_POINT('Ctrl Pts',(-3.67074983340444,1.,0.980505922458494));
#52384=CARTESIAN_POINT('Ctrl Pts',(-3.67782408841876,-1.,0.983550791470864));
#52385=CARTESIAN_POINT('Ctrl Pts',(-3.67782408841876,1.,0.983550791470864));
#52386=CARTESIAN_POINT('Ctrl Pts',(-3.6845531792623,-1.,0.986602639864285));
#52387=CARTESIAN_POINT('Ctrl Pts',(-3.6845531792623,1.,0.986602639864285));
#52388=CARTESIAN_POINT('Ctrl Pts',(-3.69102682138955,-1.,0.989676715398858));
#52389=CARTESIAN_POINT('Ctrl Pts',(-3.69102682138955,1.,0.989676715398858));
#52390=CARTESIAN_POINT('Ctrl Pts',(-3.69738123415696,-1.,0.992802218332103));
#52391=CARTESIAN_POINT('Ctrl Pts',(-3.69738123415696,1.,0.992802218332103));
#52392=CARTESIAN_POINT('Ctrl Pts',(-3.70375282282107,-1.,0.996009819772431));
#52393=CARTESIAN_POINT('Ctrl Pts',(-3.70375282282107,1.,0.996009819772431));
#52394=CARTESIAN_POINT('Ctrl Pts',(-3.7102243971387,-1.,0.999317260756344));
#52395=CARTESIAN_POINT('Ctrl Pts',(-3.7102243971387,1.,0.999317260756344));
#52396=CARTESIAN_POINT('Ctrl Pts',(-3.71680667125047,-1.,1.00272423396802));
#52397=CARTESIAN_POINT('Ctrl Pts',(-3.71680667125047,1.,1.00272423396802));
#52398=CARTESIAN_POINT('Ctrl Pts',(-3.72346803750544,-1.,1.00622000735696));
#52399=CARTESIAN_POINT('Ctrl Pts',(-3.72346803750544,1.,1.00622000735696));
#52400=CARTESIAN_POINT('Ctrl Pts',(-3.73015276704407,-1.,1.00978798539491));
#52401=CARTESIAN_POINT('Ctrl Pts',(-3.73015276704407,1.,1.00978798539491));
#52402=CARTESIAN_POINT('Ctrl Pts',(-3.73680245055747,-1.,1.01341114319906));
#52403=CARTESIAN_POINT('Ctrl Pts',(-3.73680245055747,1.,1.01341114319906));
#52404=CARTESIAN_POINT('Ctrl Pts',(-3.74337942504993,-1.,1.01707794311088));
#52405=CARTESIAN_POINT('Ctrl Pts',(-3.74337942504993,1.,1.01707794311088));
#52406=CARTESIAN_POINT('Ctrl Pts',(-3.74987777155873,-1.,1.02078510487439));
#52407=CARTESIAN_POINT('Ctrl Pts',(-3.74987777155873,1.,1.02078510487439));
#52408=CARTESIAN_POINT('Ctrl Pts',(-3.75631037456224,-1.,1.02453429444668));
#52409=CARTESIAN_POINT('Ctrl Pts',(-3.75631037456224,1.,1.02453429444668));
#52410=CARTESIAN_POINT('Ctrl Pts',(-3.76270122291245,-1.,1.02833014458184));
#52411=CARTESIAN_POINT('Ctrl Pts',(-3.76270122291245,1.,1.02833014458184));
#52412=CARTESIAN_POINT('Ctrl Pts',(-3.76907609832516,-1.,1.03217786604919));
#52413=CARTESIAN_POINT('Ctrl Pts',(-3.76907609832516,1.,1.03217786604919));
#52414=CARTESIAN_POINT('Ctrl Pts',(-3.77545283140427,-1.,1.03608074678008));
#52415=CARTESIAN_POINT('Ctrl Pts',(-3.77545283140427,1.,1.03608074678008));
#52416=CARTESIAN_POINT('Ctrl Pts',(-3.7818353500817,-1.,1.04003862055798));
#52417=CARTESIAN_POINT('Ctrl Pts',(-3.7818353500817,1.,1.04003862055798));
#52418=CARTESIAN_POINT('Ctrl Pts',(-3.78821910787179,-1.,1.04404924374422));
#52419=CARTESIAN_POINT('Ctrl Pts',(-3.78821910787179,1.,1.04404924374422));
#52420=CARTESIAN_POINT('Ctrl Pts',(-3.79459440308786,-1.,1.04810913267639));
#52421=CARTESIAN_POINT('Ctrl Pts',(-3.79459440308786,1.,1.04810913267639));
#52422=CARTESIAN_POINT('Ctrl Pts',(-3.80095039790681,-1.,1.05221457990016));
#52423=CARTESIAN_POINT('Ctrl Pts',(-3.80095039790681,1.,1.05221457990016));
#52424=CARTESIAN_POINT('Ctrl Pts',(-3.80727913637791,-1.,1.05636266918644));
#52425=CARTESIAN_POINT('Ctrl Pts',(-3.80727913637791,1.,1.05636266918644));
#52426=CARTESIAN_POINT('Ctrl Pts',(-3.8135786611749,-1.,1.06055206187299));
#52427=CARTESIAN_POINT('Ctrl Pts',(-3.8135786611749,1.,1.06055206187299));
#52428=CARTESIAN_POINT('Ctrl Pts',(-3.81985083953012,-1.,1.0647824403893));
#52429=CARTESIAN_POINT('Ctrl Pts',(-3.81985083953012,1.,1.0647824403893));
#52430=CARTESIAN_POINT('Ctrl Pts',(-3.82609989967276,-1.,1.06905413180359));
#52431=CARTESIAN_POINT('Ctrl Pts',(-3.82609989967276,1.,1.06905413180359));
#52432=CARTESIAN_POINT('Ctrl Pts',(-3.83233071195144,-1.,1.07336766633459));
#52433=CARTESIAN_POINT('Ctrl Pts',(-3.83233071195144,1.,1.07336766633459));
#52434=CARTESIAN_POINT('Ctrl Pts',(-3.83854714117491,-1.,1.07772335353858));
#52435=CARTESIAN_POINT('Ctrl Pts',(-3.83854714117491,1.,1.07772335353858));
#52436=CARTESIAN_POINT('Ctrl Pts',(-3.8447504803063,-1.,1.08212087917991));
#52437=CARTESIAN_POINT('Ctrl Pts',(-3.8447504803063,1.,1.08212087917991));
#52438=CARTESIAN_POINT('Ctrl Pts',(-3.85094025222713,-1.,1.08655950846384));
#52439=CARTESIAN_POINT('Ctrl Pts',(-3.85094025222713,1.,1.08655950846384));
#52440=CARTESIAN_POINT('Ctrl Pts',(-3.85711487933931,-1.,1.09103825516294));
#52441=CARTESIAN_POINT('Ctrl Pts',(-3.85711487933931,1.,1.09103825516294));
#52442=CARTESIAN_POINT('Ctrl Pts',(-3.86327241021247,-1.,1.09555606505013));
#52443=CARTESIAN_POINT('Ctrl Pts',(-3.86327241021247,1.,1.09555606505013));
#52444=CARTESIAN_POINT('Ctrl Pts',(-3.86941120134849,-1.,1.10011198761195));
#52445=CARTESIAN_POINT('Ctrl Pts',(-3.86941120134849,1.,1.10011198761195));
#52446=CARTESIAN_POINT('Ctrl Pts',(-3.87553067187514,-1.,1.10470536603287));
#52447=CARTESIAN_POINT('Ctrl Pts',(-3.87553067187514,1.,1.10470536603287));
#52448=CARTESIAN_POINT('Ctrl Pts',(-3.88163105531724,-1.,1.10933577224008));
#52449=CARTESIAN_POINT('Ctrl Pts',(-3.88163105531724,1.,1.10933577224008));
#52450=CARTESIAN_POINT('Ctrl Pts',(-3.88771308285171,-1.,1.11400292434429));
#52451=CARTESIAN_POINT('Ctrl Pts',(-3.88771308285171,1.,1.11400292434429));
#52452=CARTESIAN_POINT('Ctrl Pts',(-3.89377768340344,-1.,1.11870660794603));
#52453=CARTESIAN_POINT('Ctrl Pts',(-3.89377768340344,1.,1.11870660794603));
#52454=CARTESIAN_POINT('Ctrl Pts',(-3.89982569750025,-1.,1.12344660099043));
#52455=CARTESIAN_POINT('Ctrl Pts',(-3.89982569750025,1.,1.12344660099043));
#52456=CARTESIAN_POINT('Ctrl Pts',(-3.90585753318737,-1.,1.12822258281553));
#52457=CARTESIAN_POINT('Ctrl Pts',(-3.90585753318737,1.,1.12822258281553));
#52458=CARTESIAN_POINT('Ctrl Pts',(-3.91187321145649,-1.,1.13303414693896));
#52459=CARTESIAN_POINT('Ctrl Pts',(-3.91187321145649,1.,1.13303414693896));
#52460=CARTESIAN_POINT('Ctrl Pts',(-3.91787251936827,-1.,1.13788084225554));
#52461=CARTESIAN_POINT('Ctrl Pts',(-3.91787251936827,1.,1.13788084225554));
#52462=CARTESIAN_POINT('Ctrl Pts',(-3.92385513133997,-1.,1.14276220561593));
#52463=CARTESIAN_POINT('Ctrl Pts',(-3.92385513133997,1.,1.14276220561593));
#52464=CARTESIAN_POINT('Ctrl Pts',(-3.92982073294257,-1.,1.14767779451123));
#52465=CARTESIAN_POINT('Ctrl Pts',(-3.92982073294257,1.,1.14767779451123));
#52466=CARTESIAN_POINT('Ctrl Pts',(-3.9357691705628,-1.,1.1526272271632));
#52467=CARTESIAN_POINT('Ctrl Pts',(-3.9357691705628,1.,1.1526272271632));
#52468=CARTESIAN_POINT('Ctrl Pts',(-3.94170046685203,-1.,1.15761018340956));
#52469=CARTESIAN_POINT('Ctrl Pts',(-3.94170046685203,1.,1.15761018340956));
#52470=CARTESIAN_POINT('Ctrl Pts',(-3.94761474780583,-1.,1.16262637999157));
#52471=CARTESIAN_POINT('Ctrl Pts',(-3.94761474780583,1.,1.16262637999157));
#52472=CARTESIAN_POINT('Ctrl Pts',(-3.95351219509876,-1.,1.16767555244438));
#52473=CARTESIAN_POINT('Ctrl Pts',(-3.95351219509876,1.,1.16767555244438));
#52474=CARTESIAN_POINT('Ctrl Pts',(-3.95939299213276,-1.,1.17275743590361));
#52475=CARTESIAN_POINT('Ctrl Pts',(-3.95939299213276,1.,1.17275743590361));
#52476=CARTESIAN_POINT('Ctrl Pts',(-3.96525726358159,-1.,1.17787174135592));
#52477=CARTESIAN_POINT('Ctrl Pts',(-3.96525726358159,1.,1.17787174135592));
#52478=CARTESIAN_POINT('Ctrl Pts',(-3.97110505165415,-1.,1.18301815039831));
#52479=CARTESIAN_POINT('Ctrl Pts',(-3.97110505165415,1.,1.18301815039831));
#52480=CARTESIAN_POINT('Ctrl Pts',(-3.97693634767754,-1.,1.18819633715539));
#52481=CARTESIAN_POINT('Ctrl Pts',(-3.97693634767754,1.,1.18819633715539));
#52482=CARTESIAN_POINT('Ctrl Pts',(-3.98275111052561,-1.,1.19340598349475));
#52483=CARTESIAN_POINT('Ctrl Pts',(-3.98275111052561,1.,1.19340598349475));
#52484=CARTESIAN_POINT('Ctrl Pts',(-3.98854928957189,-1.,1.19864679609566));
#52485=CARTESIAN_POINT('Ctrl Pts',(-3.98854928957189,1.,1.19864679609566));
#52486=CARTESIAN_POINT('Ctrl Pts',(-3.99433084799666,-1.,1.20391852375139));
#52487=CARTESIAN_POINT('Ctrl Pts',(-3.99433084799666,1.,1.20391852375139));
#52488=CARTESIAN_POINT('Ctrl Pts',(-4.00009577950721,-1.,1.20922097029551));
#52489=CARTESIAN_POINT('Ctrl Pts',(-4.00009577950721,1.,1.20922097029551));
#52490=CARTESIAN_POINT('Ctrl Pts',(-4.00584409522722,-1.,1.21455398918133));
#52491=CARTESIAN_POINT('Ctrl Pts',(-4.00584409522722,1.,1.21455398918133));
#52492=CARTESIAN_POINT('Ctrl Pts',(-4.01042947140789,-1.,1.21884478244403));
#52493=CARTESIAN_POINT('Ctrl Pts',(-4.01042947140789,1.,1.21884478244403));
#52494=CARTESIAN_POINT('Ctrl Pts',(-4.01386104433519,-1.,1.22207656455845));
#52495=CARTESIAN_POINT('Ctrl Pts',(-4.01386104433519,1.,1.22207656455845));
#52496=CARTESIAN_POINT('Ctrl Pts',(-4.01614544569895,-1.,1.22423716681317));
#52497=CARTESIAN_POINT('Ctrl Pts',(-4.01614544569895,1.,1.22423716681317));
#52498=CARTESIAN_POINT('Ctrl Pts',(-4.01728681790024,-1.,1.22531898815164));
#52499=CARTESIAN_POINT('Ctrl Pts',(-4.01728681790024,1.,1.22531898815164));
#52500=CARTESIAN_POINT('',(-3.62400312501199,1.,0.963899035118986));
#52501=CARTESIAN_POINT('Ctrl Pts',(-3.62400312501199,-1.,0.963899035118986));
#52502=CARTESIAN_POINT('Ctrl Pts',(-3.62400312501199,-0.666666666666667,
0.963899035118986));
#52503=CARTESIAN_POINT('Ctrl Pts',(-3.62400312501199,-0.333333333333333,
0.963899035118986));
#52504=CARTESIAN_POINT('Ctrl Pts',(-3.62400312501199,0.333333333333333,
0.963899035118986));
#52505=CARTESIAN_POINT('Ctrl Pts',(-3.62400312501199,0.666666666666667,
0.963899035118985));
#52506=CARTESIAN_POINT('Ctrl Pts',(-3.62400312501199,1.,0.963899035118985));
#52507=CARTESIAN_POINT('',(-4.01728681790024,1.,1.22531898815164));
#52508=CARTESIAN_POINT('',(-4.01728681790024,0.,1.22531898815164));
#52509=CARTESIAN_POINT('Ctrl Pts',(-3.62400312501199,1.,0.963899035118985));
#52510=CARTESIAN_POINT('Ctrl Pts',(-3.62404828878374,1.,0.963880158556713));
#52511=CARTESIAN_POINT('Ctrl Pts',(-3.62424461507455,1.,0.963861297423579));
#52512=CARTESIAN_POINT('Ctrl Pts',(-3.62489305727516,1.,0.963957782642589));
#52513=CARTESIAN_POINT('Ctrl Pts',(-3.62652618145252,1.,0.964373850166081));
#52514=CARTESIAN_POINT('Ctrl Pts',(-3.62988252139998,1.,0.965395153165716));
#52515=CARTESIAN_POINT('Ctrl Pts',(-3.6349212208096,1.,0.967052554540877));
#52516=CARTESIAN_POINT('Ctrl Pts',(-3.64113946505393,1.,0.969195124674829));
#52517=CARTESIAN_POINT('Ctrl Pts',(-3.64819756447072,1.,0.971722122060277));
#52518=CARTESIAN_POINT('Ctrl Pts',(-3.6557157673487,1.,0.974519971354138));
#52519=CARTESIAN_POINT('Ctrl Pts',(-3.66333049637403,1.,0.977478312751416));
#52520=CARTESIAN_POINT('Ctrl Pts',(-3.67074983340444,1.,0.980505922458494));
#52521=CARTESIAN_POINT('Ctrl Pts',(-3.67782408841876,1.,0.983550791470864));
#52522=CARTESIAN_POINT('Ctrl Pts',(-3.6845531792623,1.,0.986602639864285));
#52523=CARTESIAN_POINT('Ctrl Pts',(-3.69102682138955,1.,0.989676715398858));
#52524=CARTESIAN_POINT('Ctrl Pts',(-3.69738123415696,1.,0.992802218332103));
#52525=CARTESIAN_POINT('Ctrl Pts',(-3.70375282282107,1.,0.996009819772431));
#52526=CARTESIAN_POINT('Ctrl Pts',(-3.7102243971387,1.,0.999317260756344));
#52527=CARTESIAN_POINT('Ctrl Pts',(-3.71680667125047,1.,1.00272423396802));
#52528=CARTESIAN_POINT('Ctrl Pts',(-3.72346803750544,1.,1.00622000735696));
#52529=CARTESIAN_POINT('Ctrl Pts',(-3.73015276704407,1.,1.00978798539491));
#52530=CARTESIAN_POINT('Ctrl Pts',(-3.73680245055747,1.,1.01341114319906));
#52531=CARTESIAN_POINT('Ctrl Pts',(-3.74337942504993,1.,1.01707794311088));
#52532=CARTESIAN_POINT('Ctrl Pts',(-3.74987777155873,1.,1.02078510487439));
#52533=CARTESIAN_POINT('Ctrl Pts',(-3.75631037456224,1.,1.02453429444668));
#52534=CARTESIAN_POINT('Ctrl Pts',(-3.76270122291245,1.,1.02833014458184));
#52535=CARTESIAN_POINT('Ctrl Pts',(-3.76907609832516,1.,1.03217786604919));
#52536=CARTESIAN_POINT('Ctrl Pts',(-3.77545283140427,1.,1.03608074678008));
#52537=CARTESIAN_POINT('Ctrl Pts',(-3.7818353500817,1.,1.04003862055798));
#52538=CARTESIAN_POINT('Ctrl Pts',(-3.78821910787179,1.,1.04404924374422));
#52539=CARTESIAN_POINT('Ctrl Pts',(-3.79459440308786,1.,1.04810913267639));
#52540=CARTESIAN_POINT('Ctrl Pts',(-3.80095039790681,1.,1.05221457990016));
#52541=CARTESIAN_POINT('Ctrl Pts',(-3.80727913637791,1.,1.05636266918644));
#52542=CARTESIAN_POINT('Ctrl Pts',(-3.8135786611749,1.,1.06055206187299));
#52543=CARTESIAN_POINT('Ctrl Pts',(-3.81985083953012,1.,1.0647824403893));
#52544=CARTESIAN_POINT('Ctrl Pts',(-3.82609989967276,1.,1.06905413180359));
#52545=CARTESIAN_POINT('Ctrl Pts',(-3.83233071195144,1.,1.07336766633459));
#52546=CARTESIAN_POINT('Ctrl Pts',(-3.83854714117491,1.,1.07772335353858));
#52547=CARTESIAN_POINT('Ctrl Pts',(-3.8447504803063,1.,1.08212087917991));
#52548=CARTESIAN_POINT('Ctrl Pts',(-3.85094025222713,1.,1.08655950846384));
#52549=CARTESIAN_POINT('Ctrl Pts',(-3.85711487933931,1.,1.09103825516294));
#52550=CARTESIAN_POINT('Ctrl Pts',(-3.86327241021247,1.,1.09555606505013));
#52551=CARTESIAN_POINT('Ctrl Pts',(-3.86941120134849,1.,1.10011198761195));
#52552=CARTESIAN_POINT('Ctrl Pts',(-3.87553067187514,1.,1.10470536603287));
#52553=CARTESIAN_POINT('Ctrl Pts',(-3.88163105531724,1.,1.10933577224008));
#52554=CARTESIAN_POINT('Ctrl Pts',(-3.88771308285171,1.,1.11400292434429));
#52555=CARTESIAN_POINT('Ctrl Pts',(-3.89377768340344,1.,1.11870660794603));
#52556=CARTESIAN_POINT('Ctrl Pts',(-3.89982569750025,1.,1.12344660099043));
#52557=CARTESIAN_POINT('Ctrl Pts',(-3.90585753318737,1.,1.12822258281553));
#52558=CARTESIAN_POINT('Ctrl Pts',(-3.91187321145649,1.,1.13303414693896));
#52559=CARTESIAN_POINT('Ctrl Pts',(-3.91787251936827,1.,1.13788084225554));
#52560=CARTESIAN_POINT('Ctrl Pts',(-3.92385513133997,1.,1.14276220561593));
#52561=CARTESIAN_POINT('Ctrl Pts',(-3.92982073294257,1.,1.14767779451123));
#52562=CARTESIAN_POINT('Ctrl Pts',(-3.9357691705628,1.,1.1526272271632));
#52563=CARTESIAN_POINT('Ctrl Pts',(-3.94170046685203,1.,1.15761018340956));
#52564=CARTESIAN_POINT('Ctrl Pts',(-3.94761474780583,1.,1.16262637999157));
#52565=CARTESIAN_POINT('Ctrl Pts',(-3.95351219509876,1.,1.16767555244438));
#52566=CARTESIAN_POINT('Ctrl Pts',(-3.95939299213276,1.,1.17275743590361));
#52567=CARTESIAN_POINT('Ctrl Pts',(-3.96525726358159,1.,1.17787174135592));
#52568=CARTESIAN_POINT('Ctrl Pts',(-3.97110505165415,1.,1.18301815039831));
#52569=CARTESIAN_POINT('Ctrl Pts',(-3.97693634767754,1.,1.18819633715539));
#52570=CARTESIAN_POINT('Ctrl Pts',(-3.98275111052561,1.,1.19340598349475));
#52571=CARTESIAN_POINT('Ctrl Pts',(-3.98854928957189,1.,1.19864679609566));
#52572=CARTESIAN_POINT('Ctrl Pts',(-3.99433084799666,1.,1.20391852375139));
#52573=CARTESIAN_POINT('Ctrl Pts',(-4.00009577950721,1.,1.20922097029551));
#52574=CARTESIAN_POINT('Ctrl Pts',(-4.00584409522722,1.,1.21455398918133));
#52575=CARTESIAN_POINT('Ctrl Pts',(-4.01042947140789,1.,1.21884478244403));
#52576=CARTESIAN_POINT('Ctrl Pts',(-4.01386104433519,1.,1.22207656455845));
#52577=CARTESIAN_POINT('Ctrl Pts',(-4.01614544569895,1.,1.22423716681317));
#52578=CARTESIAN_POINT('Ctrl Pts',(-4.01728681790024,1.,1.22531898815164));
#52579=CARTESIAN_POINT('Origin',(-4.01728681790024,0.,1.22531898815164));
#52580=CARTESIAN_POINT('',(-3.97027773754922,1.,1.36999806084572));
#52581=CARTESIAN_POINT('Origin',(0.,0.,0.));
#52582=CARTESIAN_POINT('',(-3.66661143271648,1.,0.786422660833743));
#52583=CARTESIAN_POINT('Origin',(0.,1.,0.));
#52584=CARTESIAN_POINT('Ctrl Pts',(-3.66661143271648,1.,0.786422660833743));
#52585=CARTESIAN_POINT('Ctrl Pts',(-3.66661143271648,0.666666666666667,
0.786422660833743));
#52586=CARTESIAN_POINT('Ctrl Pts',(-3.66661143271648,0.333333333333333,
0.786422660833743));
#52587=CARTESIAN_POINT('Ctrl Pts',(-3.66661143271648,-0.333333333333333,
0.786422660833743));
#52588=CARTESIAN_POINT('Ctrl Pts',(-3.66661143271648,-0.666666666666667,
0.786422660833743));
#52589=CARTESIAN_POINT('Ctrl Pts',(-3.66661143271648,-1.,0.786422660833743));
#52590=CARTESIAN_POINT('Ctrl Pts',(-4.13571194405636,-1.,0.732042837400619));
#52591=CARTESIAN_POINT('Ctrl Pts',(-4.13571194405636,1.,0.732042837400619));
#52592=CARTESIAN_POINT('Ctrl Pts',(-4.13420383737278,-1.,0.732488575135926));
#52593=CARTESIAN_POINT('Ctrl Pts',(-4.13420383737278,1.,0.732488575135926));
#52594=CARTESIAN_POINT('Ctrl Pts',(-4.13118752796397,-1.,0.733376589325634));
#52595=CARTESIAN_POINT('Ctrl Pts',(-4.13118752796397,1.,0.733376589325634));
#52596=CARTESIAN_POINT('Ctrl Pts',(-4.12666277572794,-1.,0.734698226767512));
#52597=CARTESIAN_POINT('Ctrl Pts',(-4.12666277572794,1.,0.734698226767512));
#52598=CARTESIAN_POINT('Ctrl Pts',(-4.12062919626082,-1.,0.736439634335347));
#52599=CARTESIAN_POINT('Ctrl Pts',(-4.12062919626082,1.,0.736439634335347));
#52600=CARTESIAN_POINT('Ctrl Pts',(-4.11308626953795,-1.,0.738581708229118));
#52601=CARTESIAN_POINT('Ctrl Pts',(-4.11308626953795,1.,0.738581708229118));
#52602=CARTESIAN_POINT('Ctrl Pts',(-4.1055424175856,-1.,0.740688998555151));
#52603=CARTESIAN_POINT('Ctrl Pts',(-4.1055424175856,1.,0.740688998555151));
#52604=CARTESIAN_POINT('Ctrl Pts',(-4.09799769702712,-1.,0.742761369690017));
#52605=CARTESIAN_POINT('Ctrl Pts',(-4.09799769702712,1.,0.742761369690017));
#52606=CARTESIAN_POINT('Ctrl Pts',(-4.09045220253011,-1.,0.744798649705514));
#52607=CARTESIAN_POINT('Ctrl Pts',(-4.09045220253011,1.,0.744798649705514));
#52608=CARTESIAN_POINT('Ctrl Pts',(-4.08290608094789,-1.,0.746800631490821));
#52609=CARTESIAN_POINT('Ctrl Pts',(-4.08290608094789,1.,0.746800631490821));
#52610=CARTESIAN_POINT('Ctrl Pts',(-4.07535951055363,-1.,0.748767076679177));
#52611=CARTESIAN_POINT('Ctrl Pts',(-4.07535951055363,1.,0.748767076679177));
#52612=CARTESIAN_POINT('Ctrl Pts',(-4.06781267241886,-1.,0.750697720483175));
#52613=CARTESIAN_POINT('Ctrl Pts',(-4.06781267241886,1.,0.750697720483175));
#52614=CARTESIAN_POINT('Ctrl Pts',(-4.06026572221399,-1.,0.752592276482869));
#52615=CARTESIAN_POINT('Ctrl Pts',(-4.06026572221399,1.,0.752592276482869));
#52616=CARTESIAN_POINT('Ctrl Pts',(-4.05271876688106,-1.,0.754450441816411));
#52617=CARTESIAN_POINT('Ctrl Pts',(-4.05271876688106,1.,0.754450441816411));
#52618=CARTESIAN_POINT('Ctrl Pts',(-4.04517182654344,-1.,0.756271902370186));
#52619=CARTESIAN_POINT('Ctrl Pts',(-4.04517182654344,1.,0.756271902370186));
#52620=CARTESIAN_POINT('Ctrl Pts',(-4.03762485803468,-1.,0.758056338885553));
#52621=CARTESIAN_POINT('Ctrl Pts',(-4.03762485803468,1.,0.758056338885553));
#52622=CARTESIAN_POINT('Ctrl Pts',(-4.0300778195465,-1.,0.759803433244166));
#52623=CARTESIAN_POINT('Ctrl Pts',(-4.0300778195465,1.,0.759803433244166));
#52624=CARTESIAN_POINT('Ctrl Pts',(-4.02253072741347,-1.,0.761512875859941));
#52625=CARTESIAN_POINT('Ctrl Pts',(-4.02253072741347,1.,0.761512875859941));
#52626=CARTESIAN_POINT('Ctrl Pts',(-4.01498370680434,-1.,0.763184371182826));
#52627=CARTESIAN_POINT('Ctrl Pts',(-4.01498370680434,1.,0.763184371182826));
#52628=CARTESIAN_POINT('Ctrl Pts',(-4.00743706791366,-1.,0.764817648784946));
#52629=CARTESIAN_POINT('Ctrl Pts',(-4.00743706791366,1.,0.764817648784946));
#52630=CARTESIAN_POINT('Ctrl Pts',(-3.99989129179464,-1.,0.766412457135785));
#52631=CARTESIAN_POINT('Ctrl Pts',(-3.99989129179464,1.,0.766412457135785));
#52632=CARTESIAN_POINT('Ctrl Pts',(-3.99234687880892,-1.,0.767968531377708));
#52633=CARTESIAN_POINT('Ctrl Pts',(-3.99234687880892,1.,0.767968531377708));
#52634=CARTESIAN_POINT('Ctrl Pts',(-3.98480422348403,-1.,0.769485566245459));
#52635=CARTESIAN_POINT('Ctrl Pts',(-3.98480422348403,1.,0.769485566245459));
#52636=CARTESIAN_POINT('Ctrl Pts',(-3.97726349165507,-1.,0.770963190030503));
#52637=CARTESIAN_POINT('Ctrl Pts',(-3.97726349165507,1.,0.770963190030503));
#52638=CARTESIAN_POINT('Ctrl Pts',(-3.96972446532832,-1.,0.772400931772238));
#52639=CARTESIAN_POINT('Ctrl Pts',(-3.96972446532832,1.,0.772400931772238));
#52640=CARTESIAN_POINT('Ctrl Pts',(-3.96218649639876,-1.,0.773798212026682));
#52641=CARTESIAN_POINT('Ctrl Pts',(-3.96218649639876,1.,0.773798212026682));
#52642=CARTESIAN_POINT('Ctrl Pts',(-3.95464885452364,-1.,0.775154418039441));
#52643=CARTESIAN_POINT('Ctrl Pts',(-3.95464885452364,1.,0.775154418039441));
#52644=CARTESIAN_POINT('Ctrl Pts',(-3.94711101619471,-1.,0.77646896669796));
#52645=CARTESIAN_POINT('Ctrl Pts',(-3.94711101619471,1.,0.77646896669796));
#52646=CARTESIAN_POINT('Ctrl Pts',(-3.93957296768098,-1.,0.777741370568549));
#52647=CARTESIAN_POINT('Ctrl Pts',(-3.93957296768098,1.,0.777741370568549));
#52648=CARTESIAN_POINT('Ctrl Pts',(-3.93203552473153,-1.,0.778971308134786));
#52649=CARTESIAN_POINT('Ctrl Pts',(-3.93203552473153,1.,0.778971308134786));
#52650=CARTESIAN_POINT('Ctrl Pts',(-3.92450058323799,-1.,0.780158678615506));
#52651=CARTESIAN_POINT('Ctrl Pts',(-3.92450058323799,1.,0.780158678615506));
#52652=CARTESIAN_POINT('Ctrl Pts',(-3.9169703605466,-1.,0.781303428618343));
#52653=CARTESIAN_POINT('Ctrl Pts',(-3.9169703605466,1.,0.781303428618343));
#52654=CARTESIAN_POINT('Ctrl Pts',(-3.90944671004536,-1.,0.782405395622758));
#52655=CARTESIAN_POINT('Ctrl Pts',(-3.90944671004536,1.,0.782405395622758));
#52656=CARTESIAN_POINT('Ctrl Pts',(-3.90193039043971,-1.,0.783464141529082));
#52657=CARTESIAN_POINT('Ctrl Pts',(-3.90193039043971,1.,0.783464141529082));
#52658=CARTESIAN_POINT('Ctrl Pts',(-3.89442039235105,-1.,0.784478799358335));
#52659=CARTESIAN_POINT('Ctrl Pts',(-3.89442039235105,1.,0.784478799358335));
#52660=CARTESIAN_POINT('Ctrl Pts',(-3.88691313167399,-1.,0.785447890340723));
#52661=CARTESIAN_POINT('Ctrl Pts',(-3.88691313167399,1.,0.785447890340723));
#52662=CARTESIAN_POINT('Ctrl Pts',(-3.87940402818186,-1.,0.786369675812592));
#52663=CARTESIAN_POINT('Ctrl Pts',(-3.87940402818186,1.,0.786369675812592));
#52664=CARTESIAN_POINT('Ctrl Pts',(-3.87188916600905,-1.,0.78724252761798));
#52665=CARTESIAN_POINT('Ctrl Pts',(-3.87188916600905,1.,0.78724252761798));
#52666=CARTESIAN_POINT('Ctrl Pts',(-3.86436702561342,-1.,0.788065315093771));
#52667=CARTESIAN_POINT('Ctrl Pts',(-3.86436702561342,1.,0.788065315093771));
#52668=CARTESIAN_POINT('Ctrl Pts',(-3.85683995872536,-1.,0.788837734090688));
#52669=CARTESIAN_POINT('Ctrl Pts',(-3.85683995872536,1.,0.788837734090688));
#52670=CARTESIAN_POINT('Ctrl Pts',(-3.8493163780891,-1.,0.789560798155618));
#52671=CARTESIAN_POINT('Ctrl Pts',(-3.8493163780891,1.,0.789560798155618));
#52672=CARTESIAN_POINT('Ctrl Pts',(-3.84180762342476,-1.,0.790236124191289));
#52673=CARTESIAN_POINT('Ctrl Pts',(-3.84180762342476,1.,0.790236124191289));
#52674=CARTESIAN_POINT('Ctrl Pts',(-3.83432392054804,-1.,0.79086501270534));
#52675=CARTESIAN_POINT('Ctrl Pts',(-3.83432392054804,1.,0.79086501270534));
#52676=CARTESIAN_POINT('Ctrl Pts',(-3.82687033899799,-1.,0.791447528662381));
#52677=CARTESIAN_POINT('Ctrl Pts',(-3.82687033899799,1.,0.791447528662381));
#52678=CARTESIAN_POINT('Ctrl Pts',(-3.81944345442237,-1.,0.791981740718606));
#52679=CARTESIAN_POINT('Ctrl Pts',(-3.81944345442237,1.,0.791981740718606));
#52680=CARTESIAN_POINT('Ctrl Pts',(-3.81202588694726,-1.,0.792462483517568));
#52681=CARTESIAN_POINT('Ctrl Pts',(-3.81202588694726,1.,0.792462483517568));
#52682=CARTESIAN_POINT('Ctrl Pts',(-3.80459229925598,-1.,0.792882695234693));
#52683=CARTESIAN_POINT('Ctrl Pts',(-3.80459229925598,1.,0.792882695234693));
#52684=CARTESIAN_POINT('Ctrl Pts',(-3.79711921389862,-1.,0.7932356129732));
#52685=CARTESIAN_POINT('Ctrl Pts',(-3.79711921389862,1.,0.7932356129732));
#52686=CARTESIAN_POINT('Ctrl Pts',(-3.78959439439222,-1.,0.793516871680966));
#52687=CARTESIAN_POINT('Ctrl Pts',(-3.78959439439222,1.,0.793516871680966));
#52688=CARTESIAN_POINT('Ctrl Pts',(-3.78202460377617,-1.,0.793726235781339));
#52689=CARTESIAN_POINT('Ctrl Pts',(-3.78202460377617,1.,0.793726235781339));
#52690=CARTESIAN_POINT('Ctrl Pts',(-3.77444863801264,-1.,0.793870523787515));
#52691=CARTESIAN_POINT('Ctrl Pts',(-3.77444863801264,1.,0.793870523787515));
#52692=CARTESIAN_POINT('Ctrl Pts',(-3.76692626931184,-1.,0.793961083689141));
#52693=CARTESIAN_POINT('Ctrl Pts',(-3.76692626931184,1.,0.793961083689141));
#52694=CARTESIAN_POINT('Ctrl Pts',(-3.75951468666325,-1.,0.794008429135047));
#52695=CARTESIAN_POINT('Ctrl Pts',(-3.75951468666325,1.,0.794008429135047));
#52696=CARTESIAN_POINT('Ctrl Pts',(-3.75224692493895,-1.,0.79401734737144));
#52697=CARTESIAN_POINT('Ctrl Pts',(-3.75224692493895,1.,0.79401734737144));
#52698=CARTESIAN_POINT('Ctrl Pts',(-3.74511357728827,-1.,0.79398270045988));
#52699=CARTESIAN_POINT('Ctrl Pts',(-3.74511357728827,1.,0.79398270045988));
#52700=CARTESIAN_POINT('Ctrl Pts',(-3.73803280541576,-1.,0.79388270093679));
#52701=CARTESIAN_POINT('Ctrl Pts',(-3.73803280541576,1.,0.79388270093679));
#52702=CARTESIAN_POINT('Ctrl Pts',(-3.7308691469564,-1.,0.793682750269347));
#52703=CARTESIAN_POINT('Ctrl Pts',(-3.7308691469564,1.,0.793682750269347));
#52704=CARTESIAN_POINT('Ctrl Pts',(-3.7234879729357,-1.,0.79334702378387));
#52705=CARTESIAN_POINT('Ctrl Pts',(-3.7234879729357,1.,0.79334702378387));
#52706=CARTESIAN_POINT('Ctrl Pts',(-3.7158024239604,-1.,0.792848377370115));
#52707=CARTESIAN_POINT('Ctrl Pts',(-3.7158024239604,1.,0.792848377370115));
#52708=CARTESIAN_POINT('Ctrl Pts',(-3.70781724021879,-1.,0.792177688845967));
#52709=CARTESIAN_POINT('Ctrl Pts',(-3.70781724021879,1.,0.792177688845967));
#52710=CARTESIAN_POINT('Ctrl Pts',(-3.69968940808982,-1.,0.791356575696509));
#52711=CARTESIAN_POINT('Ctrl Pts',(-3.69968940808982,1.,0.791356575696509));
#52712=CARTESIAN_POINT('Ctrl Pts',(-3.69172044327754,-1.,0.79043628498958));
#52713=CARTESIAN_POINT('Ctrl Pts',(-3.69172044327754,1.,0.79043628498958));
#52714=CARTESIAN_POINT('Ctrl Pts',(-3.68428439784285,-1.,0.789483546065158));
#52715=CARTESIAN_POINT('Ctrl Pts',(-3.68428439784285,1.,0.789483546065158));
#52716=CARTESIAN_POINT('Ctrl Pts',(-3.67777119516438,-1.,0.788569566220662));
#52717=CARTESIAN_POINT('Ctrl Pts',(-3.67777119516438,1.,0.788569566220662));
#52718=CARTESIAN_POINT('Ctrl Pts',(-3.672529236635,-1.,0.787758799995426));
#52719=CARTESIAN_POINT('Ctrl Pts',(-3.672529236635,1.,0.787758799995426));
#52720=CARTESIAN_POINT('Ctrl Pts',(-3.66879484800625,-1.,0.787095252589507));
#52721=CARTESIAN_POINT('Ctrl Pts',(-3.66879484800625,1.,0.787095252589507));
#52722=CARTESIAN_POINT('Ctrl Pts',(-3.66710211819938,-1.,0.786698783541657));
#52723=CARTESIAN_POINT('Ctrl Pts',(-3.66710211819938,1.,0.786698783541657));
#52724=CARTESIAN_POINT('Ctrl Pts',(-3.66657784454965,-1.,0.786480236184947));
#52725=CARTESIAN_POINT('Ctrl Pts',(-3.66657784454965,1.,0.786480236184947));
#52726=CARTESIAN_POINT('Ctrl Pts',(-3.66655932661846,-1.,0.786369528183039));
#52727=CARTESIAN_POINT('Ctrl Pts',(-3.66655932661846,1.,0.786369528183039));
#52728=CARTESIAN_POINT('Ctrl Pts',(-3.66663282329846,-1.,0.786322922920599));
#52729=CARTESIAN_POINT('Ctrl Pts',(-3.66663282329846,1.,0.786322922920599));
#52730=CARTESIAN_POINT('',(-4.13571194405636,1.,0.732042837400619));
#52731=CARTESIAN_POINT('Ctrl Pts',(-4.13571194405636,1.,0.732042837400619));
#52732=CARTESIAN_POINT('Ctrl Pts',(-4.13420383737278,1.,0.732488575135926));
#52733=CARTESIAN_POINT('Ctrl Pts',(-4.13118752796397,1.,0.733376589325634));
#52734=CARTESIAN_POINT('Ctrl Pts',(-4.12666277572794,1.,0.734698226767512));
#52735=CARTESIAN_POINT('Ctrl Pts',(-4.12062919626082,1.,0.736439634335347));
#52736=CARTESIAN_POINT('Ctrl Pts',(-4.11308626953795,1.,0.738581708229118));
#52737=CARTESIAN_POINT('Ctrl Pts',(-4.1055424175856,1.,0.740688998555151));
#52738=CARTESIAN_POINT('Ctrl Pts',(-4.09799769702712,1.,0.742761369690017));
#52739=CARTESIAN_POINT('Ctrl Pts',(-4.09045220253011,1.,0.744798649705514));
#52740=CARTESIAN_POINT('Ctrl Pts',(-4.08290608094789,1.,0.746800631490821));
#52741=CARTESIAN_POINT('Ctrl Pts',(-4.07535951055363,1.,0.748767076679177));
#52742=CARTESIAN_POINT('Ctrl Pts',(-4.06781267241886,1.,0.750697720483175));
#52743=CARTESIAN_POINT('Ctrl Pts',(-4.06026572221399,1.,0.752592276482869));
#52744=CARTESIAN_POINT('Ctrl Pts',(-4.05271876688106,1.,0.754450441816411));
#52745=CARTESIAN_POINT('Ctrl Pts',(-4.04517182654344,1.,0.756271902370186));
#52746=CARTESIAN_POINT('Ctrl Pts',(-4.03762485803468,1.,0.758056338885553));
#52747=CARTESIAN_POINT('Ctrl Pts',(-4.0300778195465,1.,0.759803433244166));
#52748=CARTESIAN_POINT('Ctrl Pts',(-4.02253072741347,1.,0.761512875859941));
#52749=CARTESIAN_POINT('Ctrl Pts',(-4.01498370680434,1.,0.763184371182826));
#52750=CARTESIAN_POINT('Ctrl Pts',(-4.00743706791366,1.,0.764817648784946));
#52751=CARTESIAN_POINT('Ctrl Pts',(-3.99989129179464,1.,0.766412457135785));
#52752=CARTESIAN_POINT('Ctrl Pts',(-3.99234687880892,1.,0.767968531377708));
#52753=CARTESIAN_POINT('Ctrl Pts',(-3.98480422348403,1.,0.769485566245459));
#52754=CARTESIAN_POINT('Ctrl Pts',(-3.97726349165507,1.,0.770963190030503));
#52755=CARTESIAN_POINT('Ctrl Pts',(-3.96972446532832,1.,0.772400931772238));
#52756=CARTESIAN_POINT('Ctrl Pts',(-3.96218649639876,1.,0.773798212026682));
#52757=CARTESIAN_POINT('Ctrl Pts',(-3.95464885452364,1.,0.775154418039441));
#52758=CARTESIAN_POINT('Ctrl Pts',(-3.94711101619471,1.,0.77646896669796));
#52759=CARTESIAN_POINT('Ctrl Pts',(-3.93957296768098,1.,0.777741370568549));
#52760=CARTESIAN_POINT('Ctrl Pts',(-3.93203552473153,1.,0.778971308134786));
#52761=CARTESIAN_POINT('Ctrl Pts',(-3.92450058323799,1.,0.780158678615506));
#52762=CARTESIAN_POINT('Ctrl Pts',(-3.9169703605466,1.,0.781303428618343));
#52763=CARTESIAN_POINT('Ctrl Pts',(-3.90944671004536,1.,0.782405395622758));
#52764=CARTESIAN_POINT('Ctrl Pts',(-3.90193039043971,1.,0.783464141529082));
#52765=CARTESIAN_POINT('Ctrl Pts',(-3.89442039235105,1.,0.784478799358335));
#52766=CARTESIAN_POINT('Ctrl Pts',(-3.88691313167399,1.,0.785447890340723));
#52767=CARTESIAN_POINT('Ctrl Pts',(-3.87940402818186,1.,0.786369675812592));
#52768=CARTESIAN_POINT('Ctrl Pts',(-3.87188916600905,1.,0.78724252761798));
#52769=CARTESIAN_POINT('Ctrl Pts',(-3.86436702561342,1.,0.788065315093771));
#52770=CARTESIAN_POINT('Ctrl Pts',(-3.85683995872536,1.,0.788837734090688));
#52771=CARTESIAN_POINT('Ctrl Pts',(-3.8493163780891,1.,0.789560798155618));
#52772=CARTESIAN_POINT('Ctrl Pts',(-3.84180762342476,1.,0.790236124191289));
#52773=CARTESIAN_POINT('Ctrl Pts',(-3.83432392054804,1.,0.79086501270534));
#52774=CARTESIAN_POINT('Ctrl Pts',(-3.82687033899799,1.,0.791447528662381));
#52775=CARTESIAN_POINT('Ctrl Pts',(-3.81944345442237,1.,0.791981740718606));
#52776=CARTESIAN_POINT('Ctrl Pts',(-3.81202588694726,1.,0.792462483517568));
#52777=CARTESIAN_POINT('Ctrl Pts',(-3.80459229925598,1.,0.792882695234693));
#52778=CARTESIAN_POINT('Ctrl Pts',(-3.79711921389862,1.,0.7932356129732));
#52779=CARTESIAN_POINT('Ctrl Pts',(-3.78959439439222,1.,0.793516871680966));
#52780=CARTESIAN_POINT('Ctrl Pts',(-3.78202460377617,1.,0.793726235781339));
#52781=CARTESIAN_POINT('Ctrl Pts',(-3.77444863801264,1.,0.793870523787515));
#52782=CARTESIAN_POINT('Ctrl Pts',(-3.76692626931184,1.,0.793961083689141));
#52783=CARTESIAN_POINT('Ctrl Pts',(-3.75951468666325,1.,0.794008429135047));
#52784=CARTESIAN_POINT('Ctrl Pts',(-3.75224692493895,1.,0.79401734737144));
#52785=CARTESIAN_POINT('Ctrl Pts',(-3.74511357728827,1.,0.79398270045988));
#52786=CARTESIAN_POINT('Ctrl Pts',(-3.73803280541576,1.,0.79388270093679));
#52787=CARTESIAN_POINT('Ctrl Pts',(-3.7308691469564,1.,0.793682750269347));
#52788=CARTESIAN_POINT('Ctrl Pts',(-3.7234879729357,1.,0.79334702378387));
#52789=CARTESIAN_POINT('Ctrl Pts',(-3.7158024239604,1.,0.792848377370115));
#52790=CARTESIAN_POINT('Ctrl Pts',(-3.70781724021879,1.,0.792177688845967));
#52791=CARTESIAN_POINT('Ctrl Pts',(-3.69968940808982,1.,0.791356575696509));
#52792=CARTESIAN_POINT('Ctrl Pts',(-3.69172044327754,1.,0.79043628498958));
#52793=CARTESIAN_POINT('Ctrl Pts',(-3.68428439784285,1.,0.789483546065158));
#52794=CARTESIAN_POINT('Ctrl Pts',(-3.67777119516438,1.,0.788569566220662));
#52795=CARTESIAN_POINT('Ctrl Pts',(-3.672529236635,1.,0.787758799995426));
#52796=CARTESIAN_POINT('Ctrl Pts',(-3.66907505398769,1.,0.787145041181588));
#52797=CARTESIAN_POINT('Ctrl Pts',(-3.66743103898844,1.,0.786774337198499));
#52798=CARTESIAN_POINT('Ctrl Pts',(-3.66680946938396,1.,0.786565919559889));
#52799=CARTESIAN_POINT('Ctrl Pts',(-3.66664310415236,1.,0.786459983896781));
#52800=CARTESIAN_POINT('Ctrl Pts',(-3.66661143271648,1.,0.786422660833743));
#52801=CARTESIAN_POINT('',(-4.13571194405636,0.,0.732042837400619));
#52802=CARTESIAN_POINT('Ctrl Pts',(-3.73016218570874,-1.,0.385214314776329));
#52803=CARTESIAN_POINT('Ctrl Pts',(-3.73016218570874,1.,0.385214314776329));
#52804=CARTESIAN_POINT('Ctrl Pts',(-3.73010668803185,-1.,0.385147278814804));
#52805=CARTESIAN_POINT('Ctrl Pts',(-3.73010668803185,1.,0.385147278814804));
#52806=CARTESIAN_POINT('Ctrl Pts',(-3.73015851028729,-1.,0.385047711603887));
#52807=CARTESIAN_POINT('Ctrl Pts',(-3.73015851028729,1.,0.385047711603887));
#52808=CARTESIAN_POINT('Ctrl Pts',(-3.73072465900727,-1.,0.385001870183841));
#52809=CARTESIAN_POINT('Ctrl Pts',(-3.73072465900727,1.,0.385001870183841));
#52810=CARTESIAN_POINT('Ctrl Pts',(-3.73245705639337,-1.,0.385147887989514));
#52811=CARTESIAN_POINT('Ctrl Pts',(-3.73245705639337,1.,0.385147887989514));
#52812=CARTESIAN_POINT('Ctrl Pts',(-3.73621371845475,-1.,0.385670806454744));
#52813=CARTESIAN_POINT('Ctrl Pts',(-3.73621371845475,1.,0.385670806454744));
#52814=CARTESIAN_POINT('Ctrl Pts',(-3.74144965781088,-1.,0.386519576222035));
#52815=CARTESIAN_POINT('Ctrl Pts',(-3.74144965781088,1.,0.386519576222035));
#52816=CARTESIAN_POINT('Ctrl Pts',(-3.74792651696269,-1.,0.387663020050396));
#52817=CARTESIAN_POINT('Ctrl Pts',(-3.74792651696269,1.,0.387663020050396));
#52818=CARTESIAN_POINT('Ctrl Pts',(-3.75529302894757,-1.,0.389054775898251));
#52819=CARTESIAN_POINT('Ctrl Pts',(-3.75529302894757,1.,0.389054775898251));
#52820=CARTESIAN_POINT('Ctrl Pts',(-3.76315635032993,-1.,0.390642072979259));
#52821=CARTESIAN_POINT('Ctrl Pts',(-3.76315635032993,1.,0.390642072979259));
#52822=CARTESIAN_POINT('Ctrl Pts',(-3.77114011595892,-1.,0.392372786223346));
#52823=CARTESIAN_POINT('Ctrl Pts',(-3.77114011595892,1.,0.392372786223346));
#52824=CARTESIAN_POINT('Ctrl Pts',(-3.77894173114368,-1.,0.394202481011595));
#52825=CARTESIAN_POINT('Ctrl Pts',(-3.77894173114368,1.,0.394202481011595));
#52826=CARTESIAN_POINT('Ctrl Pts',(-3.78640521279479,-1.,0.396103205335028));
#52827=CARTESIAN_POINT('Ctrl Pts',(-3.78640521279479,1.,0.396103205335028));
#52828=CARTESIAN_POINT('Ctrl Pts',(-3.79352887163457,-1.,0.398064818684158));
#52829=CARTESIAN_POINT('Ctrl Pts',(-3.79352887163457,1.,0.398064818684158));
#52830=CARTESIAN_POINT('Ctrl Pts',(-3.80040370384659,-1.,0.400088346504726));
#52831=CARTESIAN_POINT('Ctrl Pts',(-3.80040370384659,1.,0.400088346504726));
#52832=CARTESIAN_POINT('Ctrl Pts',(-3.80716881962763,-1.,0.402181320148474));
#52833=CARTESIAN_POINT('Ctrl Pts',(-3.80716881962763,1.,0.402181320148474));
#52834=CARTESIAN_POINT('Ctrl Pts',(-3.81396374287762,-1.,0.404352694628236));
#52835=CARTESIAN_POINT('Ctrl Pts',(-3.81396374287762,1.,0.404352694628236));
#52836=CARTESIAN_POINT('Ctrl Pts',(-3.82087303913741,-1.,0.406607038258906));
#52837=CARTESIAN_POINT('Ctrl Pts',(-3.82087303913741,1.,0.406607038258906));
#52838=CARTESIAN_POINT('Ctrl Pts',(-3.82790724256397,-1.,0.408942371447377));
#52839=CARTESIAN_POINT('Ctrl Pts',(-3.82790724256397,1.,0.408942371447377));
#52840=CARTESIAN_POINT('Ctrl Pts',(-3.83503345578645,-1.,0.411353038798459));
#52841=CARTESIAN_POINT('Ctrl Pts',(-3.83503345578645,1.,0.411353038798459));
#52842=CARTESIAN_POINT('Ctrl Pts',(-3.84219403994742,-1.,0.413831367016726));
#52843=CARTESIAN_POINT('Ctrl Pts',(-3.84219403994742,1.,0.413831367016726));
#52844=CARTESIAN_POINT('Ctrl Pts',(-3.8493286415751,-1.,0.41636967805292));
#52845=CARTESIAN_POINT('Ctrl Pts',(-3.8493286415751,1.,0.41636967805292));
#52846=CARTESIAN_POINT('Ctrl Pts',(-3.85639825648031,-1.,0.418962468086809));
#52847=CARTESIAN_POINT('Ctrl Pts',(-3.85639825648031,1.,0.418962468086809));
#52848=CARTESIAN_POINT('Ctrl Pts',(-3.86339652542749,-1.,0.421607423177575));
#52849=CARTESIAN_POINT('Ctrl Pts',(-3.86339652542749,1.,0.421607423177575));
#52850=CARTESIAN_POINT('Ctrl Pts',(-3.87033643487882,-1.,0.424304173195142));
#52851=CARTESIAN_POINT('Ctrl Pts',(-3.87033643487882,1.,0.424304173195142));
#52852=CARTESIAN_POINT('Ctrl Pts',(-3.87724240306609,-1.,0.427053541173469));
#52853=CARTESIAN_POINT('Ctrl Pts',(-3.87724240306609,1.,0.427053541173469));
#52854=CARTESIAN_POINT('Ctrl Pts',(-3.88414070943334,-1.,0.429856640579733));
#52855=CARTESIAN_POINT('Ctrl Pts',(-3.88414070943334,1.,0.429856640579733));
#52856=CARTESIAN_POINT('Ctrl Pts',(-3.89104947940592,-1.,0.432713929544439));
#52857=CARTESIAN_POINT('Ctrl Pts',(-3.89104947940592,1.,0.432713929544439));
#52858=CARTESIAN_POINT('Ctrl Pts',(-3.8979725665544,-1.,0.435624629433505));
#52859=CARTESIAN_POINT('Ctrl Pts',(-3.8979725665544,1.,0.435624629433505));
#52860=CARTESIAN_POINT('Ctrl Pts',(-3.90490512938546,-1.,0.438587235458233));
#52861=CARTESIAN_POINT('Ctrl Pts',(-3.90490512938546,1.,0.438587235458233));
#52862=CARTESIAN_POINT('Ctrl Pts',(-3.91183704069146,-1.,0.441599824524047));
#52863=CARTESIAN_POINT('Ctrl Pts',(-3.91183704069146,1.,0.441599824524047));
#52864=CARTESIAN_POINT('Ctrl Pts',(-3.91875701610721,-1.,0.444660430230592));
#52865=CARTESIAN_POINT('Ctrl Pts',(-3.91875701610721,1.,0.444660430230592));
#52866=CARTESIAN_POINT('Ctrl Pts',(-3.92565674143424,-1.,0.447767416837296));
#52867=CARTESIAN_POINT('Ctrl Pts',(-3.92565674143424,1.,0.447767416837296));
#52868=CARTESIAN_POINT('Ctrl Pts',(-3.93253407403128,-1.,0.450919768356347));
#52869=CARTESIAN_POINT('Ctrl Pts',(-3.93253407403128,1.,0.450919768356347));
#52870=CARTESIAN_POINT('Ctrl Pts',(-3.93939080846298,-1.,0.454116879027576));
#52871=CARTESIAN_POINT('Ctrl Pts',(-3.93939080846298,1.,0.454116879027576));
#52872=CARTESIAN_POINT('Ctrl Pts',(-3.94623117206675,-1.,0.457358410451674));
#52873=CARTESIAN_POINT('Ctrl Pts',(-3.94623117206675,1.,0.457358410451674));
#52874=CARTESIAN_POINT('Ctrl Pts',(-3.95306005817363,-1.,0.460644124429119));
#52875=CARTESIAN_POINT('Ctrl Pts',(-3.95306005817363,1.,0.460644124429119));
#52876=CARTESIAN_POINT('Ctrl Pts',(-3.95988133243543,-1.,0.463973722115744));
#52877=CARTESIAN_POINT('Ctrl Pts',(-3.95988133243543,1.,0.463973722115744));
#52878=CARTESIAN_POINT('Ctrl Pts',(-3.96669622273946,-1.,0.467346690880671));
#52879=CARTESIAN_POINT('Ctrl Pts',(-3.96669622273946,1.,0.467346690880671));
#52880=CARTESIAN_POINT('Ctrl Pts',(-3.97350414289415,-1.,0.470762379613477));
#52881=CARTESIAN_POINT('Ctrl Pts',(-3.97350414289415,1.,0.470762379613477));
#52882=CARTESIAN_POINT('Ctrl Pts',(-3.9803033804443,-1.,0.474220061019542));
#52883=CARTESIAN_POINT('Ctrl Pts',(-3.9803033804443,1.,0.474220061019542));
#52884=CARTESIAN_POINT('Ctrl Pts',(-3.98709184306743,-1.,0.477718999122033));
#52885=CARTESIAN_POINT('Ctrl Pts',(-3.98709184306743,1.,0.477718999122033));
#52886=CARTESIAN_POINT('Ctrl Pts',(-3.99386775880655,-1.,0.481258512209638));
#52887=CARTESIAN_POINT('Ctrl Pts',(-3.99386775880655,1.,0.481258512209638));
#52888=CARTESIAN_POINT('Ctrl Pts',(-4.00063045119234,-1.,0.484838042421754));
#52889=CARTESIAN_POINT('Ctrl Pts',(-4.00063045119234,1.,0.484838042421754));
#52890=CARTESIAN_POINT('Ctrl Pts',(-4.0073800839092,-1.,0.48845713042453));
#52891=CARTESIAN_POINT('Ctrl Pts',(-4.0073800839092,1.,0.48845713042453));
#52892=CARTESIAN_POINT('Ctrl Pts',(-4.01411733503486,-1.,0.49211538341793));
#52893=CARTESIAN_POINT('Ctrl Pts',(-4.01411733503486,1.,0.49211538341793));
#52894=CARTESIAN_POINT('Ctrl Pts',(-4.02084308851813,-1.,0.495812444326223));
#52895=CARTESIAN_POINT('Ctrl Pts',(-4.02084308851813,1.,0.495812444326223));
#52896=CARTESIAN_POINT('Ctrl Pts',(-4.0275581398015,-1.,0.499547962340889));
#52897=CARTESIAN_POINT('Ctrl Pts',(-4.0275581398015,1.,0.499547962340889));
#52898=CARTESIAN_POINT('Ctrl Pts',(-4.0342628417439,-1.,0.503321556915513));
#52899=CARTESIAN_POINT('Ctrl Pts',(-4.0342628417439,1.,0.503321556915513));
#52900=CARTESIAN_POINT('Ctrl Pts',(-4.04095715149074,-1.,0.507132823288361));
#52901=CARTESIAN_POINT('Ctrl Pts',(-4.04095715149074,1.,0.507132823288361));
#52902=CARTESIAN_POINT('Ctrl Pts',(-4.04764078815591,-1.,0.510981349219173));
#52903=CARTESIAN_POINT('Ctrl Pts',(-4.04764078815591,1.,0.510981349219173));
#52904=CARTESIAN_POINT('Ctrl Pts',(-4.05431335771261,-1.,0.514866728193104));
#52905=CARTESIAN_POINT('Ctrl Pts',(-4.05431335771261,1.,0.514866728193104));
#52906=CARTESIAN_POINT('Ctrl Pts',(-4.06097448037934,-1.,0.518788572336809));
#52907=CARTESIAN_POINT('Ctrl Pts',(-4.06097448037934,1.,0.518788572336809));
#52908=CARTESIAN_POINT('Ctrl Pts',(-4.06762394471075,-1.,0.522746528602767));
#52909=CARTESIAN_POINT('Ctrl Pts',(-4.06762394471075,1.,0.522746528602767));
#52910=CARTESIAN_POINT('Ctrl Pts',(-4.07426172299496,-1.,0.526740277226999));
#52911=CARTESIAN_POINT('Ctrl Pts',(-4.07426172299496,1.,0.526740277226999));
#52912=CARTESIAN_POINT('Ctrl Pts',(-4.08088789536488,-1.,0.530769518728075));
#52913=CARTESIAN_POINT('Ctrl Pts',(-4.08088789536488,1.,0.530769518728075));
#52914=CARTESIAN_POINT('Ctrl Pts',(-4.08750259988693,-1.,0.534833963476999));
#52915=CARTESIAN_POINT('Ctrl Pts',(-4.08750259988693,1.,0.534833963476999));
#52916=CARTESIAN_POINT('Ctrl Pts',(-4.09410597627116,-1.,0.53893332117992));
#52917=CARTESIAN_POINT('Ctrl Pts',(-4.09410597627116,1.,0.53893332117992));
#52918=CARTESIAN_POINT('Ctrl Pts',(-4.10069810244473,-1.,0.543067286878457));
#52919=CARTESIAN_POINT('Ctrl Pts',(-4.10069810244473,1.,0.543067286878457));
#52920=CARTESIAN_POINT('Ctrl Pts',(-4.1072789702877,-1.,0.547235539486759));
#52921=CARTESIAN_POINT('Ctrl Pts',(-4.1072789702877,1.,0.547235539486759));
#52922=CARTESIAN_POINT('Ctrl Pts',(-4.11384852025578,-1.,0.551437758498246));
#52923=CARTESIAN_POINT('Ctrl Pts',(-4.11384852025578,1.,0.551437758498246));
#52924=CARTESIAN_POINT('Ctrl Pts',(-4.1204066619623,-1.,0.555673636130778));
#52925=CARTESIAN_POINT('Ctrl Pts',(-4.1204066619623,1.,0.555673636130778));
#52926=CARTESIAN_POINT('Ctrl Pts',(-4.12695329951859,-1.,0.559942890594628));
#52927=CARTESIAN_POINT('Ctrl Pts',(-4.12695329951859,1.,0.559942890594628));
#52928=CARTESIAN_POINT('Ctrl Pts',(-4.13348835726086,-1.,0.564245279535705));
#52929=CARTESIAN_POINT('Ctrl Pts',(-4.13348835726086,1.,0.564245279535705));
#52930=CARTESIAN_POINT('Ctrl Pts',(-4.14001179828669,-1.,0.568580610187116));
#52931=CARTESIAN_POINT('Ctrl Pts',(-4.14001179828669,1.,0.568580610187116));
#52932=CARTESIAN_POINT('Ctrl Pts',(-4.14652361065787,-1.,0.572948736066276));
#52933=CARTESIAN_POINT('Ctrl Pts',(-4.14652361065787,1.,0.572948736066276));
#52934=CARTESIAN_POINT('Ctrl Pts',(-4.1517237611974,-1.,0.576469391673916));
#52935=CARTESIAN_POINT('Ctrl Pts',(-4.1517237611974,1.,0.576469391673916));
#52936=CARTESIAN_POINT('Ctrl Pts',(-4.15561864787379,-1.,0.579124568912543));
#52937=CARTESIAN_POINT('Ctrl Pts',(-4.15561864787379,1.,0.579124568912543));
#52938=CARTESIAN_POINT('Ctrl Pts',(-4.15821291712391,-1.,0.580901211462913));
#52939=CARTESIAN_POINT('Ctrl Pts',(-4.15821291712391,1.,0.580901211462913));
#52940=CARTESIAN_POINT('Ctrl Pts',(-4.15950947128175,-1.,0.581791163835814));
#52941=CARTESIAN_POINT('Ctrl Pts',(-4.15950947128175,1.,0.581791163835814));
#52942=CARTESIAN_POINT('',(-3.73017266276632,1.,0.385112848332549));
#52943=CARTESIAN_POINT('Ctrl Pts',(-3.73017266276632,-1.,0.385112848332549));
#52944=CARTESIAN_POINT('Ctrl Pts',(-3.73017266276632,-0.666666666666667,
0.385112848332549));
#52945=CARTESIAN_POINT('Ctrl Pts',(-3.73017266276632,-0.333333333333333,
0.385112848332549));
#52946=CARTESIAN_POINT('Ctrl Pts',(-3.73017266276632,0.333333333333333,
0.385112848332549));
#52947=CARTESIAN_POINT('Ctrl Pts',(-3.73017266276632,0.666666666666667,
0.385112848332549));
#52948=CARTESIAN_POINT('Ctrl Pts',(-3.73017266276632,1.,0.385112848332549));
#52949=CARTESIAN_POINT('',(-4.15950947128175,1.,0.581791163835814));
#52950=CARTESIAN_POINT('',(-4.15950947128175,0.,0.581791163835814));
#52951=CARTESIAN_POINT('Ctrl Pts',(-3.73017266276632,1.,0.385112848332549));
#52952=CARTESIAN_POINT('Ctrl Pts',(-3.73021431755218,1.,0.385087139001609));
#52953=CARTESIAN_POINT('Ctrl Pts',(-3.73040527620929,1.,0.385037797882046));
#52954=CARTESIAN_POINT('Ctrl Pts',(-3.73106082862399,1.,0.385031656499141));
#52955=CARTESIAN_POINT('Ctrl Pts',(-3.73273893363318,1.,0.385187124633964));
#52956=CARTESIAN_POINT('Ctrl Pts',(-3.73621371845475,1.,0.385670806454744));
#52957=CARTESIAN_POINT('Ctrl Pts',(-3.74144965781088,1.,0.386519576222035));
#52958=CARTESIAN_POINT('Ctrl Pts',(-3.74792651696269,1.,0.387663020050396));
#52959=CARTESIAN_POINT('Ctrl Pts',(-3.75529302894757,1.,0.389054775898251));
#52960=CARTESIAN_POINT('Ctrl Pts',(-3.76315635032993,1.,0.390642072979259));
#52961=CARTESIAN_POINT('Ctrl Pts',(-3.77114011595892,1.,0.392372786223346));
#52962=CARTESIAN_POINT('Ctrl Pts',(-3.77894173114368,1.,0.394202481011595));
#52963=CARTESIAN_POINT('Ctrl Pts',(-3.78640521279479,1.,0.396103205335028));
#52964=CARTESIAN_POINT('Ctrl Pts',(-3.79352887163457,1.,0.398064818684158));
#52965=CARTESIAN_POINT('Ctrl Pts',(-3.80040370384659,1.,0.400088346504726));
#52966=CARTESIAN_POINT('Ctrl Pts',(-3.80716881962763,1.,0.402181320148474));
#52967=CARTESIAN_POINT('Ctrl Pts',(-3.81396374287762,1.,0.404352694628236));
#52968=CARTESIAN_POINT('Ctrl Pts',(-3.82087303913741,1.,0.406607038258906));
#52969=CARTESIAN_POINT('Ctrl Pts',(-3.82790724256397,1.,0.408942371447377));
#52970=CARTESIAN_POINT('Ctrl Pts',(-3.83503345578645,1.,0.411353038798459));
#52971=CARTESIAN_POINT('Ctrl Pts',(-3.84219403994742,1.,0.413831367016726));
#52972=CARTESIAN_POINT('Ctrl Pts',(-3.8493286415751,1.,0.41636967805292));
#52973=CARTESIAN_POINT('Ctrl Pts',(-3.85639825648031,1.,0.418962468086809));
#52974=CARTESIAN_POINT('Ctrl Pts',(-3.86339652542749,1.,0.421607423177575));
#52975=CARTESIAN_POINT('Ctrl Pts',(-3.87033643487882,1.,0.424304173195142));
#52976=CARTESIAN_POINT('Ctrl Pts',(-3.87724240306609,1.,0.427053541173469));
#52977=CARTESIAN_POINT('Ctrl Pts',(-3.88414070943334,1.,0.429856640579733));
#52978=CARTESIAN_POINT('Ctrl Pts',(-3.89104947940592,1.,0.432713929544439));
#52979=CARTESIAN_POINT('Ctrl Pts',(-3.8979725665544,1.,0.435624629433505));
#52980=CARTESIAN_POINT('Ctrl Pts',(-3.90490512938546,1.,0.438587235458233));
#52981=CARTESIAN_POINT('Ctrl Pts',(-3.91183704069146,1.,0.441599824524047));
#52982=CARTESIAN_POINT('Ctrl Pts',(-3.91875701610721,1.,0.444660430230592));
#52983=CARTESIAN_POINT('Ctrl Pts',(-3.92565674143424,1.,0.447767416837296));
#52984=CARTESIAN_POINT('Ctrl Pts',(-3.93253407403128,1.,0.450919768356347));
#52985=CARTESIAN_POINT('Ctrl Pts',(-3.93939080846298,1.,0.454116879027576));
#52986=CARTESIAN_POINT('Ctrl Pts',(-3.94623117206675,1.,0.457358410451674));
#52987=CARTESIAN_POINT('Ctrl Pts',(-3.95306005817363,1.,0.460644124429119));
#52988=CARTESIAN_POINT('Ctrl Pts',(-3.95988133243543,1.,0.463973722115744));
#52989=CARTESIAN_POINT('Ctrl Pts',(-3.96669622273946,1.,0.467346690880671));
#52990=CARTESIAN_POINT('Ctrl Pts',(-3.97350414289415,1.,0.470762379613477));
#52991=CARTESIAN_POINT('Ctrl Pts',(-3.9803033804443,1.,0.474220061019542));
#52992=CARTESIAN_POINT('Ctrl Pts',(-3.98709184306743,1.,0.477718999122033));
#52993=CARTESIAN_POINT('Ctrl Pts',(-3.99386775880655,1.,0.481258512209638));
#52994=CARTESIAN_POINT('Ctrl Pts',(-4.00063045119234,1.,0.484838042421754));
#52995=CARTESIAN_POINT('Ctrl Pts',(-4.0073800839092,1.,0.48845713042453));
#52996=CARTESIAN_POINT('Ctrl Pts',(-4.01411733503486,1.,0.49211538341793));
#52997=CARTESIAN_POINT('Ctrl Pts',(-4.02084308851813,1.,0.495812444326223));
#52998=CARTESIAN_POINT('Ctrl Pts',(-4.0275581398015,1.,0.499547962340889));
#52999=CARTESIAN_POINT('Ctrl Pts',(-4.0342628417439,1.,0.503321556915513));
#53000=CARTESIAN_POINT('Ctrl Pts',(-4.04095715149074,1.,0.507132823288361));
#53001=CARTESIAN_POINT('Ctrl Pts',(-4.04764078815591,1.,0.510981349219173));
#53002=CARTESIAN_POINT('Ctrl Pts',(-4.05431335771261,1.,0.514866728193104));
#53003=CARTESIAN_POINT('Ctrl Pts',(-4.06097448037934,1.,0.518788572336809));
#53004=CARTESIAN_POINT('Ctrl Pts',(-4.06762394471075,1.,0.522746528602767));
#53005=CARTESIAN_POINT('Ctrl Pts',(-4.07426172299496,1.,0.526740277226999));
#53006=CARTESIAN_POINT('Ctrl Pts',(-4.08088789536488,1.,0.530769518728075));
#53007=CARTESIAN_POINT('Ctrl Pts',(-4.08750259988693,1.,0.534833963476999));
#53008=CARTESIAN_POINT('Ctrl Pts',(-4.09410597627116,1.,0.53893332117992));
#53009=CARTESIAN_POINT('Ctrl Pts',(-4.10069810244473,1.,0.543067286878457));
#53010=CARTESIAN_POINT('Ctrl Pts',(-4.1072789702877,1.,0.547235539486759));
#53011=CARTESIAN_POINT('Ctrl Pts',(-4.11384852025578,1.,0.551437758498246));
#53012=CARTESIAN_POINT('Ctrl Pts',(-4.1204066619623,1.,0.555673636130778));
#53013=CARTESIAN_POINT('Ctrl Pts',(-4.12695329951859,1.,0.559942890594628));
#53014=CARTESIAN_POINT('Ctrl Pts',(-4.13348835726086,1.,0.564245279535705));
#53015=CARTESIAN_POINT('Ctrl Pts',(-4.14001179828669,1.,0.568580610187116));
#53016=CARTESIAN_POINT('Ctrl Pts',(-4.14652361065787,1.,0.572948736066276));
#53017=CARTESIAN_POINT('Ctrl Pts',(-4.1517237611974,1.,0.576469391673916));
#53018=CARTESIAN_POINT('Ctrl Pts',(-4.15561864787379,1.,0.579124568912543));
#53019=CARTESIAN_POINT('Ctrl Pts',(-4.15821291712391,1.,0.580901211462913));
#53020=CARTESIAN_POINT('Ctrl Pts',(-4.15950947128175,1.,0.581791163835814));
#53021=CARTESIAN_POINT('Origin',(-4.15950947128175,0.,0.581791163835814));
#53022=CARTESIAN_POINT('',(-4.13571194405636,1.,0.732042837400619));
#53023=CARTESIAN_POINT('Origin',(0.,0.,0.));
#53024=CARTESIAN_POINT('',(-3.74449296982994,1.,0.203156094897896));
#53025=CARTESIAN_POINT('Origin',(0.,1.,0.));
#53026=CARTESIAN_POINT('Ctrl Pts',(-3.74449296982994,1.,0.203156094897896));
#53027=CARTESIAN_POINT('Ctrl Pts',(-3.74449296982994,0.666666666666667,
0.203156094897896));
#53028=CARTESIAN_POINT('Ctrl Pts',(-3.74449296982994,0.333333333333333,
0.203156094897896));
#53029=CARTESIAN_POINT('Ctrl Pts',(-3.74449296982994,-0.333333333333333,
0.203156094897896));
#53030=CARTESIAN_POINT('Ctrl Pts',(-3.74449296982994,-0.666666666666667,
0.203156094897896));
#53031=CARTESIAN_POINT('Ctrl Pts',(-3.74449296982994,-1.,0.203156094897896));
#53032=CARTESIAN_POINT('Ctrl Pts',(-4.19931119685982,-1.,0.0760622897878236));
#53033=CARTESIAN_POINT('Ctrl Pts',(-4.19931119685982,1.,0.0760622897878236));
#53034=CARTESIAN_POINT('Ctrl Pts',(-4.19789138621624,-1.,0.0767384596142195));
#53035=CARTESIAN_POINT('Ctrl Pts',(-4.19789138621624,1.,0.0767384596142195));
#53036=CARTESIAN_POINT('Ctrl Pts',(-4.19505112860624,-1.,0.0780873956244402));
#53037=CARTESIAN_POINT('Ctrl Pts',(-4.19505112860624,1.,0.0780873956244402));
#53038=CARTESIAN_POINT('Ctrl Pts',(-4.19078883322483,-1.,0.0801005887117603));
#53039=CARTESIAN_POINT('Ctrl Pts',(-4.19078883322483,1.,0.0801005887117603));
#53040=CARTESIAN_POINT('Ctrl Pts',(-4.1851019532944,-1.,0.082764416438951));
#53041=CARTESIAN_POINT('Ctrl Pts',(-4.1851019532944,1.,0.082764416438951));
#53042=CARTESIAN_POINT('Ctrl Pts',(-4.17798698669991,-1.,0.0860600915552515));
#53043=CARTESIAN_POINT('Ctrl Pts',(-4.17798698669991,1.,0.0860600915552515));
#53044=CARTESIAN_POINT('Ctrl Pts',(-4.17086566491823,-1.,0.0893215560850327));
#53045=CARTESIAN_POINT('Ctrl Pts',(-4.17086566491823,1.,0.0893215560850327));
#53046=CARTESIAN_POINT('Ctrl Pts',(-4.16373802265942,-1.,0.092548667216769));
#53047=CARTESIAN_POINT('Ctrl Pts',(-4.16373802265942,1.,0.092548667216769));
#53048=CARTESIAN_POINT('Ctrl Pts',(-4.15660412653006,-1.,0.0957412403297067));
#53049=CARTESIAN_POINT('Ctrl Pts',(-4.15660412653006,1.,0.0957412403297067));
#53050=CARTESIAN_POINT('Ctrl Pts',(-4.1494640891762,-1.,0.0988990478899811));
#53051=CARTESIAN_POINT('Ctrl Pts',(-4.1494640891762,1.,0.0988990478899811));
#53052=CARTESIAN_POINT('Ctrl Pts',(-4.14231804938737,-1.,0.102021826577454));
#53053=CARTESIAN_POINT('Ctrl Pts',(-4.14231804938737,1.,0.102021826577454));
#53054=CARTESIAN_POINT('Ctrl Pts',(-4.13516614458396,-1.,0.105109286538864));
#53055=CARTESIAN_POINT('Ctrl Pts',(-4.13516614458396,1.,0.105109286538864));
#53056=CARTESIAN_POINT('Ctrl Pts',(-4.12800848371386,-1.,0.10816112052835));
#53057=CARTESIAN_POINT('Ctrl Pts',(-4.12800848371386,1.,0.10816112052835));
#53058=CARTESIAN_POINT('Ctrl Pts',(-4.12084512502444,-1.,0.111177012683377));
#53059=CARTESIAN_POINT('Ctrl Pts',(-4.12084512502444,1.,0.111177012683377));
#53060=CARTESIAN_POINT('Ctrl Pts',(-4.11367603925313,-1.,0.114156649609601));
#53061=CARTESIAN_POINT('Ctrl Pts',(-4.11367603925313,1.,0.114156649609601));
#53062=CARTESIAN_POINT('Ctrl Pts',(-4.10650113382187,-1.,0.117099722731704));
#53063=CARTESIAN_POINT('Ctrl Pts',(-4.10650113382187,1.,0.117099722731704));
#53064=CARTESIAN_POINT('Ctrl Pts',(-4.09932031767243,-1.,0.120005924388162));
#53065=CARTESIAN_POINT('Ctrl Pts',(-4.09932031767243,1.,0.120005924388162));
#53066=CARTESIAN_POINT('Ctrl Pts',(-4.09213355850836,-1.,0.122874946249119));
#53067=CARTESIAN_POINT('Ctrl Pts',(-4.09213355850836,1.,0.122874946249119));
#53068=CARTESIAN_POINT('Ctrl Pts',(-4.08494093372315,-1.,0.125706476822529));
#53069=CARTESIAN_POINT('Ctrl Pts',(-4.08494093372315,1.,0.125706476822529));
#53070=CARTESIAN_POINT('Ctrl Pts',(-4.07774270738809,-1.,0.128500200484814));
#53071=CARTESIAN_POINT('Ctrl Pts',(-4.07774270738809,1.,0.128500200484814));
#53072=CARTESIAN_POINT('Ctrl Pts',(-4.07053931528579,-1.,0.131255793548914));
#53073=CARTESIAN_POINT('Ctrl Pts',(-4.07053931528579,1.,0.131255793548914));
#53074=CARTESIAN_POINT('Ctrl Pts',(-4.06333121018476,-1.,0.133972916144225));
#53075=CARTESIAN_POINT('Ctrl Pts',(-4.06333121018476,1.,0.133972916144225));
#53076=CARTESIAN_POINT('Ctrl Pts',(-4.05611873400122,-1.,0.136651205046111));
#53077=CARTESIAN_POINT('Ctrl Pts',(-4.05611873400122,1.,0.136651205046111));
#53078=CARTESIAN_POINT('Ctrl Pts',(-4.04890199238056,-1.,0.139290267180059));
#53079=CARTESIAN_POINT('Ctrl Pts',(-4.04890199238056,1.,0.139290267180059));
#53080=CARTESIAN_POINT('Ctrl Pts',(-4.04168069633842,-1.,0.141889671485508));
#53081=CARTESIAN_POINT('Ctrl Pts',(-4.04168069633842,1.,0.141889671485508));
#53082=CARTESIAN_POINT('Ctrl Pts',(-4.03445411510403,-1.,0.144448947038352));
#53083=CARTESIAN_POINT('Ctrl Pts',(-4.03445411510403,1.,0.144448947038352));
#53084=CARTESIAN_POINT('Ctrl Pts',(-4.02722143147048,-1.,0.146967602878998));
#53085=CARTESIAN_POINT('Ctrl Pts',(-4.02722143147048,1.,0.146967602878998));
#53086=CARTESIAN_POINT('Ctrl Pts',(-4.01998203715588,-1.,0.149445144968707));
#53087=CARTESIAN_POINT('Ctrl Pts',(-4.01998203715588,1.,0.149445144968707));
#53088=CARTESIAN_POINT('Ctrl Pts',(-4.01273584234684,-1.,0.151881094022909));
#53089=CARTESIAN_POINT('Ctrl Pts',(-4.01273584234684,1.,0.151881094022909));
#53090=CARTESIAN_POINT('Ctrl Pts',(-4.00548360245297,-1.,0.15427500487231));
#53091=CARTESIAN_POINT('Ctrl Pts',(-4.00548360245297,1.,0.15427500487231));
#53092=CARTESIAN_POINT('Ctrl Pts',(-3.99822717425869,-1.,0.156626481393735));
#53093=CARTESIAN_POINT('Ctrl Pts',(-3.99822717425869,1.,0.156626481393735));
#53094=CARTESIAN_POINT('Ctrl Pts',(-3.99096873945862,-1.,0.158935123982796));
#53095=CARTESIAN_POINT('Ctrl Pts',(-3.99096873945862,1.,0.158935123982796));
#53096=CARTESIAN_POINT('Ctrl Pts',(-3.98371010319866,-1.,0.161200482186087));
#53097=CARTESIAN_POINT('Ctrl Pts',(-3.98371010319866,1.,0.161200482186087));
#53098=CARTESIAN_POINT('Ctrl Pts',(-3.97645194630944,-1.,0.163422004609999));
#53099=CARTESIAN_POINT('Ctrl Pts',(-3.97645194630944,1.,0.163422004609999));
#53100=CARTESIAN_POINT('Ctrl Pts',(-3.9691931362141,-1.,0.165598992851097));
#53101=CARTESIAN_POINT('Ctrl Pts',(-3.9691931362141,1.,0.165598992851097));
#53102=CARTESIAN_POINT('Ctrl Pts',(-3.96192990160296,-1.,0.167730547023312));
#53103=CARTESIAN_POINT('Ctrl Pts',(-3.96192990160296,1.,0.167730547023312));
#53104=CARTESIAN_POINT('Ctrl Pts',(-3.95465744665263,-1.,0.16981566637413));
#53105=CARTESIAN_POINT('Ctrl Pts',(-3.95465744665263,1.,0.16981566637413));
#53106=CARTESIAN_POINT('Ctrl Pts',(-3.94737164900861,-1.,0.171853355369233));
#53107=CARTESIAN_POINT('Ctrl Pts',(-3.94737164900861,1.,0.171853355369233));
#53108=CARTESIAN_POINT('Ctrl Pts',(-3.94007083096214,-1.,0.173842734974607));
#53109=CARTESIAN_POINT('Ctrl Pts',(-3.94007083096214,1.,0.173842734974607));
#53110=CARTESIAN_POINT('Ctrl Pts',(-3.93275726771049,-1.,0.175783136893872));
#53111=CARTESIAN_POINT('Ctrl Pts',(-3.93275726771049,1.,0.175783136893872));
#53112=CARTESIAN_POINT('Ctrl Pts',(-3.92543942697672,-1.,0.177674246152328));
#53113=CARTESIAN_POINT('Ctrl Pts',(-3.92543942697672,1.,0.177674246152328));
#53114=CARTESIAN_POINT('Ctrl Pts',(-3.91812876180948,-1.,0.179515885822894));
#53115=CARTESIAN_POINT('Ctrl Pts',(-3.91812876180948,1.,0.179515885822894));
#53116=CARTESIAN_POINT('Ctrl Pts',(-3.91083557557193,-1.,0.181307740731796));
#53117=CARTESIAN_POINT('Ctrl Pts',(-3.91083557557193,1.,0.181307740731796));
#53118=CARTESIAN_POINT('Ctrl Pts',(-3.90356488555138,-1.,0.183049081993193));
#53119=CARTESIAN_POINT('Ctrl Pts',(-3.90356488555138,1.,0.183049081993193));
#53120=CARTESIAN_POINT('Ctrl Pts',(-3.89631300742633,-1.,0.184738537728035));
#53121=CARTESIAN_POINT('Ctrl Pts',(-3.89631300742633,1.,0.184738537728035));
#53122=CARTESIAN_POINT('Ctrl Pts',(-3.88906196725817,-1.,0.186373724985263));
#53123=CARTESIAN_POINT('Ctrl Pts',(-3.88906196725817,1.,0.186373724985263));
#53124=CARTESIAN_POINT('Ctrl Pts',(-3.88178563496187,-1.,0.187951632512663));
#53125=CARTESIAN_POINT('Ctrl Pts',(-3.88178563496187,1.,0.187951632512663));
#53126=CARTESIAN_POINT('Ctrl Pts',(-3.87445976418377,-1.,0.189469253358254));
#53127=CARTESIAN_POINT('Ctrl Pts',(-3.87445976418377,1.,0.189469253358254));
#53128=CARTESIAN_POINT('Ctrl Pts',(-3.8670715862477,-1.,0.190924190418613));
#53129=CARTESIAN_POINT('Ctrl Pts',(-3.8670715862477,1.,0.190924190418613));
#53130=CARTESIAN_POINT('Ctrl Pts',(-3.85962774407652,-1.,0.192315153044979));
#53131=CARTESIAN_POINT('Ctrl Pts',(-3.85962774407652,1.,0.192315153044979));
#53132=CARTESIAN_POINT('Ctrl Pts',(-3.85216762264019,-1.,0.193642806777747));
#53133=CARTESIAN_POINT('Ctrl Pts',(-3.85216762264019,1.,0.193642806777747));
#53134=CARTESIAN_POINT('Ctrl Pts',(-3.84475203347052,-1.,0.194909009460254));
#53135=CARTESIAN_POINT('Ctrl Pts',(-3.84475203347052,1.,0.194909009460254));
#53136=CARTESIAN_POINT('Ctrl Pts',(-3.83743910616265,-1.,0.196115198971889));
#53137=CARTESIAN_POINT('Ctrl Pts',(-3.83743910616265,1.,0.196115198971889));
#53138=CARTESIAN_POINT('Ctrl Pts',(-3.83026221776488,-1.,0.197260935827375));
#53139=CARTESIAN_POINT('Ctrl Pts',(-3.83026221776488,1.,0.197260935827375));
#53140=CARTESIAN_POINT('Ctrl Pts',(-3.82321127348981,-1.,0.19834261690047));
#53141=CARTESIAN_POINT('Ctrl Pts',(-3.82321127348981,1.,0.19834261690047));
#53142=CARTESIAN_POINT('Ctrl Pts',(-3.81620203429702,-1.,0.199351525297396));
#53143=CARTESIAN_POINT('Ctrl Pts',(-3.81620203429702,1.,0.199351525297396));
#53144=CARTESIAN_POINT('Ctrl Pts',(-3.80909529318501,-1.,0.20027467943329));
#53145=CARTESIAN_POINT('Ctrl Pts',(-3.80909529318501,1.,0.20027467943329));
#53146=CARTESIAN_POINT('Ctrl Pts',(-3.80175247447171,-1.,0.201097756307252));
#53147=CARTESIAN_POINT('Ctrl Pts',(-3.80175247447171,1.,0.201097756307252));
#53148=CARTESIAN_POINT('Ctrl Pts',(-3.79408354187274,-1.,0.201807533800799));
#53149=CARTESIAN_POINT('Ctrl Pts',(-3.79408354187274,1.,0.201807533800799));
#53150=CARTESIAN_POINT('Ctrl Pts',(-3.78609175019317,-1.,0.202394260512193));
#53151=CARTESIAN_POINT('Ctrl Pts',(-3.78609175019317,1.,0.202394260512193));
#53152=CARTESIAN_POINT('Ctrl Pts',(-3.77793553476879,-1.,0.202854729699196));
#53153=CARTESIAN_POINT('Ctrl Pts',(-3.77793553476879,1.,0.202854729699196));
#53154=CARTESIAN_POINT('Ctrl Pts',(-3.76992071595267,-1.,0.203192390045337));
#53155=CARTESIAN_POINT('Ctrl Pts',(-3.76992071595267,1.,0.203192390045337));
#53156=CARTESIAN_POINT('Ctrl Pts',(-3.76242717937273,-1.,0.203414634707646));
#53157=CARTESIAN_POINT('Ctrl Pts',(-3.76242717937273,1.,0.203414634707646));
#53158=CARTESIAN_POINT('Ctrl Pts',(-3.75585118707924,-1.,0.203530796848403));
#53159=CARTESIAN_POINT('Ctrl Pts',(-3.75585118707924,1.,0.203530796848403));
#53160=CARTESIAN_POINT('Ctrl Pts',(-3.75054693397716,-1.,0.203550035479097));
#53161=CARTESIAN_POINT('Ctrl Pts',(-3.75054693397716,1.,0.203550035479097));
#53162=CARTESIAN_POINT('Ctrl Pts',(-3.74675472018582,-1.,0.203478844530229));
#53163=CARTESIAN_POINT('Ctrl Pts',(-3.74675472018582,1.,0.203478844530229));
#53164=CARTESIAN_POINT('Ctrl Pts',(-3.7450208092684,-1.,0.203352057956055));
#53165=CARTESIAN_POINT('Ctrl Pts',(-3.7450208092684,1.,0.203352057956055));
#53166=CARTESIAN_POINT('Ctrl Pts',(-3.74446880195845,-1.,0.203218215747894));
#53167=CARTESIAN_POINT('Ctrl Pts',(-3.74446880195845,1.,0.203218215747894));
#53168=CARTESIAN_POINT('Ctrl Pts',(-3.74443319346666,-1.,0.20311176758786));
#53169=CARTESIAN_POINT('Ctrl Pts',(-3.74443319346666,1.,0.20311176758786));
#53170=CARTESIAN_POINT('Ctrl Pts',(-3.74449849461127,-1.,0.203054238699719));
#53171=CARTESIAN_POINT('Ctrl Pts',(-3.74449849461127,1.,0.203054238699719));
#53172=CARTESIAN_POINT('',(-4.19931119685982,1.,0.0760622897878236));
#53173=CARTESIAN_POINT('Ctrl Pts',(-4.19931119685982,1.,0.0760622897878236));
#53174=CARTESIAN_POINT('Ctrl Pts',(-4.19789138621624,1.,0.0767384596142195));
#53175=CARTESIAN_POINT('Ctrl Pts',(-4.19505112860624,1.,0.0780873956244402));
#53176=CARTESIAN_POINT('Ctrl Pts',(-4.19078883322483,1.,0.0801005887117603));
#53177=CARTESIAN_POINT('Ctrl Pts',(-4.1851019532944,1.,0.082764416438951));
#53178=CARTESIAN_POINT('Ctrl Pts',(-4.17798698669991,1.,0.0860600915552515));
#53179=CARTESIAN_POINT('Ctrl Pts',(-4.17086566491823,1.,0.0893215560850327));
#53180=CARTESIAN_POINT('Ctrl Pts',(-4.16373802265942,1.,0.092548667216769));
#53181=CARTESIAN_POINT('Ctrl Pts',(-4.15660412653006,1.,0.0957412403297067));
#53182=CARTESIAN_POINT('Ctrl Pts',(-4.1494640891762,1.,0.0988990478899811));
#53183=CARTESIAN_POINT('Ctrl Pts',(-4.14231804938737,1.,0.102021826577454));
#53184=CARTESIAN_POINT('Ctrl Pts',(-4.13516614458396,1.,0.105109286538864));
#53185=CARTESIAN_POINT('Ctrl Pts',(-4.12800848371386,1.,0.10816112052835));
#53186=CARTESIAN_POINT('Ctrl Pts',(-4.12084512502444,1.,0.111177012683377));
#53187=CARTESIAN_POINT('Ctrl Pts',(-4.11367603925313,1.,0.114156649609601));
#53188=CARTESIAN_POINT('Ctrl Pts',(-4.10650113382187,1.,0.117099722731704));
#53189=CARTESIAN_POINT('Ctrl Pts',(-4.09932031767243,1.,0.120005924388162));
#53190=CARTESIAN_POINT('Ctrl Pts',(-4.09213355850836,1.,0.122874946249119));
#53191=CARTESIAN_POINT('Ctrl Pts',(-4.08494093372315,1.,0.125706476822529));
#53192=CARTESIAN_POINT('Ctrl Pts',(-4.07774270738809,1.,0.128500200484814));
#53193=CARTESIAN_POINT('Ctrl Pts',(-4.07053931528579,1.,0.131255793548914));
#53194=CARTESIAN_POINT('Ctrl Pts',(-4.06333121018476,1.,0.133972916144225));
#53195=CARTESIAN_POINT('Ctrl Pts',(-4.05611873400122,1.,0.136651205046111));
#53196=CARTESIAN_POINT('Ctrl Pts',(-4.04890199238056,1.,0.139290267180059));
#53197=CARTESIAN_POINT('Ctrl Pts',(-4.04168069633842,1.,0.141889671485508));
#53198=CARTESIAN_POINT('Ctrl Pts',(-4.03445411510403,1.,0.144448947038352));
#53199=CARTESIAN_POINT('Ctrl Pts',(-4.02722143147048,1.,0.146967602878998));
#53200=CARTESIAN_POINT('Ctrl Pts',(-4.01998203715588,1.,0.149445144968707));
#53201=CARTESIAN_POINT('Ctrl Pts',(-4.01273584234684,1.,0.151881094022909));
#53202=CARTESIAN_POINT('Ctrl Pts',(-4.00548360245297,1.,0.15427500487231));
#53203=CARTESIAN_POINT('Ctrl Pts',(-3.99822717425869,1.,0.156626481393735));
#53204=CARTESIAN_POINT('Ctrl Pts',(-3.99096873945862,1.,0.158935123982796));
#53205=CARTESIAN_POINT('Ctrl Pts',(-3.98371010319866,1.,0.161200482186087));
#53206=CARTESIAN_POINT('Ctrl Pts',(-3.97645194630944,1.,0.163422004609999));
#53207=CARTESIAN_POINT('Ctrl Pts',(-3.9691931362141,1.,0.165598992851097));
#53208=CARTESIAN_POINT('Ctrl Pts',(-3.96192990160296,1.,0.167730547023312));
#53209=CARTESIAN_POINT('Ctrl Pts',(-3.95465744665263,1.,0.16981566637413));
#53210=CARTESIAN_POINT('Ctrl Pts',(-3.94737164900861,1.,0.171853355369233));
#53211=CARTESIAN_POINT('Ctrl Pts',(-3.94007083096214,1.,0.173842734974607));
#53212=CARTESIAN_POINT('Ctrl Pts',(-3.93275726771049,1.,0.175783136893872));
#53213=CARTESIAN_POINT('Ctrl Pts',(-3.92543942697672,1.,0.177674246152328));
#53214=CARTESIAN_POINT('Ctrl Pts',(-3.91812876180948,1.,0.179515885822894));
#53215=CARTESIAN_POINT('Ctrl Pts',(-3.91083557557193,1.,0.181307740731796));
#53216=CARTESIAN_POINT('Ctrl Pts',(-3.90356488555138,1.,0.183049081993193));
#53217=CARTESIAN_POINT('Ctrl Pts',(-3.89631300742633,1.,0.184738537728035));
#53218=CARTESIAN_POINT('Ctrl Pts',(-3.88906196725817,1.,0.186373724985263));
#53219=CARTESIAN_POINT('Ctrl Pts',(-3.88178563496187,1.,0.187951632512663));
#53220=CARTESIAN_POINT('Ctrl Pts',(-3.87445976418377,1.,0.189469253358254));
#53221=CARTESIAN_POINT('Ctrl Pts',(-3.8670715862477,1.,0.190924190418613));
#53222=CARTESIAN_POINT('Ctrl Pts',(-3.85962774407652,1.,0.192315153044979));
#53223=CARTESIAN_POINT('Ctrl Pts',(-3.85216762264019,1.,0.193642806777747));
#53224=CARTESIAN_POINT('Ctrl Pts',(-3.84475203347052,1.,0.194909009460254));
#53225=CARTESIAN_POINT('Ctrl Pts',(-3.83743910616265,1.,0.196115198971889));
#53226=CARTESIAN_POINT('Ctrl Pts',(-3.83026221776488,1.,0.197260935827375));
#53227=CARTESIAN_POINT('Ctrl Pts',(-3.82321127348981,1.,0.19834261690047));
#53228=CARTESIAN_POINT('Ctrl Pts',(-3.81620203429702,1.,0.199351525297396));
#53229=CARTESIAN_POINT('Ctrl Pts',(-3.80909529318501,1.,0.20027467943329));
#53230=CARTESIAN_POINT('Ctrl Pts',(-3.80175247447171,1.,0.201097756307252));
#53231=CARTESIAN_POINT('Ctrl Pts',(-3.79408354187274,1.,0.201807533800799));
#53232=CARTESIAN_POINT('Ctrl Pts',(-3.78609175019317,1.,0.202394260512193));
#53233=CARTESIAN_POINT('Ctrl Pts',(-3.77793553476879,1.,0.202854729699196));
#53234=CARTESIAN_POINT('Ctrl Pts',(-3.76992071595267,1.,0.203192390045337));
#53235=CARTESIAN_POINT('Ctrl Pts',(-3.76242717937273,1.,0.203414634707646));
#53236=CARTESIAN_POINT('Ctrl Pts',(-3.75585118707924,1.,0.203530796848403));
#53237=CARTESIAN_POINT('Ctrl Pts',(-3.75054693397716,1.,0.203550035479097));
#53238=CARTESIAN_POINT('Ctrl Pts',(-3.74703926501843,1.,0.203484186269314));
#53239=CARTESIAN_POINT('Ctrl Pts',(-3.74535749969262,1.,0.203375226874331));
#53240=CARTESIAN_POINT('Ctrl Pts',(-3.74471097893961,1.,0.203266610111264));
#53241=CARTESIAN_POINT('Ctrl Pts',(-3.74453008995129,1.,0.203188003947965));
#53242=CARTESIAN_POINT('Ctrl Pts',(-3.74449296982994,1.,0.203156094897896));
#53243=CARTESIAN_POINT('',(-4.19931119685982,0.,0.0760622897878236));
#53244=CARTESIAN_POINT('Ctrl Pts',(-3.74449849461127,-1.,-0.20305423869972));
#53245=CARTESIAN_POINT('Ctrl Pts',(-3.74449849461127,1.,-0.20305423869972));
#53246=CARTESIAN_POINT('Ctrl Pts',(-3.7444331934681,-1.,-0.203111767587923));
#53247=CARTESIAN_POINT('Ctrl Pts',(-3.7444331934681,1.,-0.203111767587923));
#53248=CARTESIAN_POINT('Ctrl Pts',(-3.7444688019622,-1.,-0.203218215748059));
#53249=CARTESIAN_POINT('Ctrl Pts',(-3.7444688019622,1.,-0.203218215748059));
#53250=CARTESIAN_POINT('Ctrl Pts',(-3.74502080927395,-1.,-0.203352057956297));
#53251=CARTESIAN_POINT('Ctrl Pts',(-3.74502080927395,1.,-0.203352057956297));
#53252=CARTESIAN_POINT('Ctrl Pts',(-3.7467547201908,-1.,-0.203478844530447));
#53253=CARTESIAN_POINT('Ctrl Pts',(-3.7467547201908,1.,-0.203478844530447));
#53254=CARTESIAN_POINT('Ctrl Pts',(-3.75054693397875,-1.,-0.203550035479166));
#53255=CARTESIAN_POINT('Ctrl Pts',(-3.75054693397875,1.,-0.203550035479166));
#53256=CARTESIAN_POINT('Ctrl Pts',(-3.75585118707734,-1.,-0.203530796848322));
#53257=CARTESIAN_POINT('Ctrl Pts',(-3.75585118707734,1.,-0.203530796848322));
#53258=CARTESIAN_POINT('Ctrl Pts',(-3.76242717936885,-1.,-0.203414634707478));
#53259=CARTESIAN_POINT('Ctrl Pts',(-3.76242717936885,1.,-0.203414634707478));
#53260=CARTESIAN_POINT('Ctrl Pts',(-3.7699207159487,-1.,-0.203192390045164));
#53261=CARTESIAN_POINT('Ctrl Pts',(-3.7699207159487,1.,-0.203192390045164));
#53262=CARTESIAN_POINT('Ctrl Pts',(-3.77793553476614,-1.,-0.202854729699081));
#53263=CARTESIAN_POINT('Ctrl Pts',(-3.77793553476614,1.,-0.202854729699081));
#53264=CARTESIAN_POINT('Ctrl Pts',(-3.78609175019242,-1.,-0.20239426051216));
#53265=CARTESIAN_POINT('Ctrl Pts',(-3.78609175019242,1.,-0.20239426051216));
#53266=CARTESIAN_POINT('Ctrl Pts',(-3.7940835418736,-1.,-0.201807533800837));
#53267=CARTESIAN_POINT('Ctrl Pts',(-3.7940835418736,1.,-0.201807533800837));
#53268=CARTESIAN_POINT('Ctrl Pts',(-3.80175247447337,-1.,-0.201097756307326));
#53269=CARTESIAN_POINT('Ctrl Pts',(-3.80175247447337,1.,-0.201097756307326));
#53270=CARTESIAN_POINT('Ctrl Pts',(-3.80909529318669,-1.,-0.200274679433364));
#53271=CARTESIAN_POINT('Ctrl Pts',(-3.80909529318669,1.,-0.200274679433364));
#53272=CARTESIAN_POINT('Ctrl Pts',(-3.81620203429815,-1.,-0.199351525297447));
#53273=CARTESIAN_POINT('Ctrl Pts',(-3.81620203429815,1.,-0.199351525297447));
#53274=CARTESIAN_POINT('Ctrl Pts',(-3.82321127349016,-1.,-0.198342616900486));
#53275=CARTESIAN_POINT('Ctrl Pts',(-3.82321127349016,1.,-0.198342616900486));
#53276=CARTESIAN_POINT('Ctrl Pts',(-3.83026221776456,-1.,-0.197260935827361));
#53277=CARTESIAN_POINT('Ctrl Pts',(-3.83026221776456,1.,-0.197260935827361));
#53278=CARTESIAN_POINT('Ctrl Pts',(-3.83743910616195,-1.,-0.196115198971859));
#53279=CARTESIAN_POINT('Ctrl Pts',(-3.83743910616195,1.,-0.196115198971859));
#53280=CARTESIAN_POINT('Ctrl Pts',(-3.84475203346977,-1.,-0.194909009460221));
#53281=CARTESIAN_POINT('Ctrl Pts',(-3.84475203346977,1.,-0.194909009460221));
#53282=CARTESIAN_POINT('Ctrl Pts',(-3.85216762263966,-1.,-0.193642806777723));
#53283=CARTESIAN_POINT('Ctrl Pts',(-3.85216762263966,1.,-0.193642806777723));
#53284=CARTESIAN_POINT('Ctrl Pts',(-3.85962774407633,-1.,-0.192315153044971));
#53285=CARTESIAN_POINT('Ctrl Pts',(-3.85962774407633,1.,-0.192315153044971));
#53286=CARTESIAN_POINT('Ctrl Pts',(-3.86707158624783,-1.,-0.19092419041862));
#53287=CARTESIAN_POINT('Ctrl Pts',(-3.86707158624783,1.,-0.19092419041862));
#53288=CARTESIAN_POINT('Ctrl Pts',(-3.87445976418412,-1.,-0.189469253358272));
#53289=CARTESIAN_POINT('Ctrl Pts',(-3.87445976418412,1.,-0.189469253358272));
#53290=CARTESIAN_POINT('Ctrl Pts',(-3.88178563496228,-1.,-0.187951632512685));
#53291=CARTESIAN_POINT('Ctrl Pts',(-3.88178563496228,1.,-0.187951632512685));
#53292=CARTESIAN_POINT('Ctrl Pts',(-3.88906196725848,-1.,-0.18637372498528));
#53293=CARTESIAN_POINT('Ctrl Pts',(-3.88906196725848,1.,-0.18637372498528));
#53294=CARTESIAN_POINT('Ctrl Pts',(-3.89631300742646,-1.,-0.184738537728043));
#53295=CARTESIAN_POINT('Ctrl Pts',(-3.89631300742646,1.,-0.184738537728043));
#53296=CARTESIAN_POINT('Ctrl Pts',(-3.90356488555132,-1.,-0.183049081993191));
#53297=CARTESIAN_POINT('Ctrl Pts',(-3.90356488555132,1.,-0.183049081993191));
#53298=CARTESIAN_POINT('Ctrl Pts',(-3.91083557557175,-1.,-0.181307740731786));
#53299=CARTESIAN_POINT('Ctrl Pts',(-3.91083557557175,1.,-0.181307740731786));
#53300=CARTESIAN_POINT('Ctrl Pts',(-3.91812876180926,-1.,-0.179515885822882));
#53301=CARTESIAN_POINT('Ctrl Pts',(-3.91812876180926,1.,-0.179515885822882));
#53302=CARTESIAN_POINT('Ctrl Pts',(-3.92543942697655,-1.,-0.177674246152317));
#53303=CARTESIAN_POINT('Ctrl Pts',(-3.92543942697655,1.,-0.177674246152317));
#53304=CARTESIAN_POINT('Ctrl Pts',(-3.93275726771042,-1.,-0.175783136893868));
#53305=CARTESIAN_POINT('Ctrl Pts',(-3.93275726771042,1.,-0.175783136893868));
#53306=CARTESIAN_POINT('Ctrl Pts',(-3.94007083096217,-1.,-0.17384273497461));
#53307=CARTESIAN_POINT('Ctrl Pts',(-3.94007083096217,1.,-0.17384273497461));
#53308=CARTESIAN_POINT('Ctrl Pts',(-3.94737164900868,-1.,-0.17185335536924));
#53309=CARTESIAN_POINT('Ctrl Pts',(-3.94737164900868,1.,-0.17185335536924));
#53310=CARTESIAN_POINT('Ctrl Pts',(-3.95465744665268,-1.,-0.169815666374139));
#53311=CARTESIAN_POINT('Ctrl Pts',(-3.95465744665268,1.,-0.169815666374139));
#53312=CARTESIAN_POINT('Ctrl Pts',(-3.96192990160296,-1.,-0.167730547023319));
#53313=CARTESIAN_POINT('Ctrl Pts',(-3.96192990160296,1.,-0.167730547023319));
#53314=CARTESIAN_POINT('Ctrl Pts',(-3.96919313621407,-1.,-0.165598992851102));
#53315=CARTESIAN_POINT('Ctrl Pts',(-3.96919313621407,1.,-0.165598992851102));
#53316=CARTESIAN_POINT('Ctrl Pts',(-3.97645194630943,-1.,-0.163422004609999));
#53317=CARTESIAN_POINT('Ctrl Pts',(-3.97645194630943,1.,-0.163422004609999));
#53318=CARTESIAN_POINT('Ctrl Pts',(-3.98371010319872,-1.,-0.161200482186085));
#53319=CARTESIAN_POINT('Ctrl Pts',(-3.98371010319872,1.,-0.161200482186085));
#53320=CARTESIAN_POINT('Ctrl Pts',(-3.99096873945878,-1.,-0.158935123982793));
#53321=CARTESIAN_POINT('Ctrl Pts',(-3.99096873945878,1.,-0.158935123982793));
#53322=CARTESIAN_POINT('Ctrl Pts',(-3.99822717425893,-1.,-0.156626481393734));
#53323=CARTESIAN_POINT('Ctrl Pts',(-3.99822717425893,1.,-0.156626481393734));
#53324=CARTESIAN_POINT('Ctrl Pts',(-4.00548360245319,-1.,-0.154275004872311));
#53325=CARTESIAN_POINT('Ctrl Pts',(-4.00548360245319,1.,-0.154275004872311));
#53326=CARTESIAN_POINT('Ctrl Pts',(-4.01273584234689,-1.,-0.151881094022911));
#53327=CARTESIAN_POINT('Ctrl Pts',(-4.01273584234689,1.,-0.151881094022911));
#53328=CARTESIAN_POINT('Ctrl Pts',(-4.01998203715564,-1.,-0.149445144968707));
#53329=CARTESIAN_POINT('Ctrl Pts',(-4.01998203715564,1.,-0.149445144968707));
#53330=CARTESIAN_POINT('Ctrl Pts',(-4.02722143146994,-1.,-0.146967602878994));
#53331=CARTESIAN_POINT('Ctrl Pts',(-4.02722143146994,1.,-0.146967602878994));
#53332=CARTESIAN_POINT('Ctrl Pts',(-4.03445411510333,-1.,-0.144448947038345));
#53333=CARTESIAN_POINT('Ctrl Pts',(-4.03445411510333,1.,-0.144448947038345));
#53334=CARTESIAN_POINT('Ctrl Pts',(-4.04168069633781,-1.,-0.1418896714855));
#53335=CARTESIAN_POINT('Ctrl Pts',(-4.04168069633781,1.,-0.1418896714855));
#53336=CARTESIAN_POINT('Ctrl Pts',(-4.04890199238036,-1.,-0.139290267180057));
#53337=CARTESIAN_POINT('Ctrl Pts',(-4.04890199238036,1.,-0.139290267180057));
#53338=CARTESIAN_POINT('Ctrl Pts',(-4.05611873400172,-1.,-0.136651205046119));
#53339=CARTESIAN_POINT('Ctrl Pts',(-4.05611873400172,1.,-0.136651205046119));
#53340=CARTESIAN_POINT('Ctrl Pts',(-4.06333121018596,-1.,-0.133972916144245));
#53341=CARTESIAN_POINT('Ctrl Pts',(-4.06333121018596,1.,-0.133972916144245));
#53342=CARTESIAN_POINT('Ctrl Pts',(-4.0705393152874,-1.,-0.13125579354894));
#53343=CARTESIAN_POINT('Ctrl Pts',(-4.0705393152874,1.,-0.13125579354894));
#53344=CARTESIAN_POINT('Ctrl Pts',(-4.07774270738954,-1.,-0.128500200484838));
#53345=CARTESIAN_POINT('Ctrl Pts',(-4.07774270738954,1.,-0.128500200484838));
#53346=CARTESIAN_POINT('Ctrl Pts',(-4.08494093372377,-1.,-0.12570647682254));
#53347=CARTESIAN_POINT('Ctrl Pts',(-4.08494093372377,1.,-0.12570647682254));
#53348=CARTESIAN_POINT('Ctrl Pts',(-4.09213355850756,-1.,-0.122874946249107));
#53349=CARTESIAN_POINT('Ctrl Pts',(-4.09213355850756,1.,-0.122874946249107));
#53350=CARTESIAN_POINT('Ctrl Pts',(-4.09932031767002,-1.,-0.120005924388124));
#53351=CARTESIAN_POINT('Ctrl Pts',(-4.09932031767002,1.,-0.120005924388124));
#53352=CARTESIAN_POINT('Ctrl Pts',(-4.10650113381833,-1.,-0.117099722731648));
#53353=CARTESIAN_POINT('Ctrl Pts',(-4.10650113381833,1.,-0.117099722731648));
#53354=CARTESIAN_POINT('Ctrl Pts',(-4.11367603924961,-1.,-0.114156649609546));
#53355=CARTESIAN_POINT('Ctrl Pts',(-4.11367603924961,1.,-0.114156649609546));
#53356=CARTESIAN_POINT('Ctrl Pts',(-4.1208451250225,-1.,-0.111177012683347));
#53357=CARTESIAN_POINT('Ctrl Pts',(-4.1208451250225,1.,-0.111177012683347));
#53358=CARTESIAN_POINT('Ctrl Pts',(-4.12800848371504,-1.,-0.108161120528369));
#53359=CARTESIAN_POINT('Ctrl Pts',(-4.12800848371504,1.,-0.108161120528369));
#53360=CARTESIAN_POINT('Ctrl Pts',(-4.13516614458895,-1.,-0.105109286538945));
#53361=CARTESIAN_POINT('Ctrl Pts',(-4.13516614458895,1.,-0.105109286538945));
#53362=CARTESIAN_POINT('Ctrl Pts',(-4.14231804939538,-1.,-0.102021826577584));
#53363=CARTESIAN_POINT('Ctrl Pts',(-4.14231804939538,1.,-0.102021826577584));
#53364=CARTESIAN_POINT('Ctrl Pts',(-4.14946408918485,-1.,-0.0988990478901226));
#53365=CARTESIAN_POINT('Ctrl Pts',(-4.14946408918485,1.,-0.0988990478901226));
#53366=CARTESIAN_POINT('Ctrl Pts',(-4.15660412653577,-1.,-0.0957412403298007));
#53367=CARTESIAN_POINT('Ctrl Pts',(-4.15660412653577,1.,-0.0957412403298007));
#53368=CARTESIAN_POINT('Ctrl Pts',(-4.16373802265839,-1.,-0.0925486672167531));
#53369=CARTESIAN_POINT('Ctrl Pts',(-4.16373802265839,1.,-0.0925486672167531));
#53370=CARTESIAN_POINT('Ctrl Pts',(-4.17086566490794,-1.,-0.0893215560848649));
#53371=CARTESIAN_POINT('Ctrl Pts',(-4.17086566490794,1.,-0.0893215560848649));
#53372=CARTESIAN_POINT('Ctrl Pts',(-4.17798698668094,-1.,-0.0860600915549397));
#53373=CARTESIAN_POINT('Ctrl Pts',(-4.17798698668094,1.,-0.0860600915549397));
#53374=CARTESIAN_POINT('Ctrl Pts',(-4.18510195327123,-1.,-0.0827644164385679));
#53375=CARTESIAN_POINT('Ctrl Pts',(-4.18510195327123,1.,-0.0827644164385679));
#53376=CARTESIAN_POINT('Ctrl Pts',(-4.19078883320504,-1.,-0.080100588711432));
#53377=CARTESIAN_POINT('Ctrl Pts',(-4.19078883320504,1.,-0.080100588711432));
#53378=CARTESIAN_POINT('Ctrl Pts',(-4.19505112859416,-1.,-0.0780873956242397));
#53379=CARTESIAN_POINT('Ctrl Pts',(-4.19505112859416,1.,-0.0780873956242397));
#53380=CARTESIAN_POINT('Ctrl Pts',(-4.1978913862118,-1.,-0.0767384596141464));
#53381=CARTESIAN_POINT('Ctrl Pts',(-4.1978913862118,1.,-0.0767384596141464));
#53382=CARTESIAN_POINT('Ctrl Pts',(-4.19931119685982,-1.,-0.0760622897878246));
#53383=CARTESIAN_POINT('Ctrl Pts',(-4.19931119685982,1.,-0.0760622897878246));
#53384=CARTESIAN_POINT('',(-3.74449296983004,1.,-0.2031560948961));
#53385=CARTESIAN_POINT('Ctrl Pts',(-3.74449296983004,-1.,-0.203156094896101));
#53386=CARTESIAN_POINT('Ctrl Pts',(-3.74449296983004,-0.666666666666667,
-0.203156094896101));
#53387=CARTESIAN_POINT('Ctrl Pts',(-3.74449296983004,-0.333333333333333,
-0.203156094896101));
#53388=CARTESIAN_POINT('Ctrl Pts',(-3.74449296983004,0.333333333333333,
-0.203156094896101));
#53389=CARTESIAN_POINT('Ctrl Pts',(-3.74449296983004,0.666666666666667,
-0.203156094896101));
#53390=CARTESIAN_POINT('Ctrl Pts',(-3.74449296983004,1.,-0.203156094896101));
#53391=CARTESIAN_POINT('',(-4.19931119685982,1.,-0.0760622897878246));
#53392=CARTESIAN_POINT('',(-4.19931119685982,0.,-0.0760622897878246));
#53393=CARTESIAN_POINT('Ctrl Pts',(-3.74449296983004,1.,-0.203156094896101));
#53394=CARTESIAN_POINT('Ctrl Pts',(-3.74453008995092,1.,-0.203188003946657));
#53395=CARTESIAN_POINT('Ctrl Pts',(-3.74471097893844,1.,-0.203266610110531));
#53396=CARTESIAN_POINT('Ctrl Pts',(-3.74535749969115,1.,-0.203375226874121));
#53397=CARTESIAN_POINT('Ctrl Pts',(-3.74703926501752,1.,-0.203484186269415));
#53398=CARTESIAN_POINT('Ctrl Pts',(-3.75054693397875,1.,-0.203550035479166));
#53399=CARTESIAN_POINT('Ctrl Pts',(-3.75585118707734,1.,-0.203530796848322));
#53400=CARTESIAN_POINT('Ctrl Pts',(-3.76242717936885,1.,-0.203414634707478));
#53401=CARTESIAN_POINT('Ctrl Pts',(-3.7699207159487,1.,-0.203192390045164));
#53402=CARTESIAN_POINT('Ctrl Pts',(-3.77793553476614,1.,-0.202854729699081));
#53403=CARTESIAN_POINT('Ctrl Pts',(-3.78609175019242,1.,-0.20239426051216));
#53404=CARTESIAN_POINT('Ctrl Pts',(-3.7940835418736,1.,-0.201807533800837));
#53405=CARTESIAN_POINT('Ctrl Pts',(-3.80175247447337,1.,-0.201097756307326));
#53406=CARTESIAN_POINT('Ctrl Pts',(-3.80909529318669,1.,-0.200274679433364));
#53407=CARTESIAN_POINT('Ctrl Pts',(-3.81620203429815,1.,-0.199351525297447));
#53408=CARTESIAN_POINT('Ctrl Pts',(-3.82321127349016,1.,-0.198342616900486));
#53409=CARTESIAN_POINT('Ctrl Pts',(-3.83026221776456,1.,-0.197260935827361));
#53410=CARTESIAN_POINT('Ctrl Pts',(-3.83743910616195,1.,-0.196115198971859));
#53411=CARTESIAN_POINT('Ctrl Pts',(-3.84475203346977,1.,-0.194909009460221));
#53412=CARTESIAN_POINT('Ctrl Pts',(-3.85216762263966,1.,-0.193642806777723));
#53413=CARTESIAN_POINT('Ctrl Pts',(-3.85962774407633,1.,-0.192315153044971));
#53414=CARTESIAN_POINT('Ctrl Pts',(-3.86707158624783,1.,-0.19092419041862));
#53415=CARTESIAN_POINT('Ctrl Pts',(-3.87445976418412,1.,-0.189469253358272));
#53416=CARTESIAN_POINT('Ctrl Pts',(-3.88178563496228,1.,-0.187951632512685));
#53417=CARTESIAN_POINT('Ctrl Pts',(-3.88906196725848,1.,-0.18637372498528));
#53418=CARTESIAN_POINT('Ctrl Pts',(-3.89631300742646,1.,-0.184738537728043));
#53419=CARTESIAN_POINT('Ctrl Pts',(-3.90356488555132,1.,-0.183049081993191));
#53420=CARTESIAN_POINT('Ctrl Pts',(-3.91083557557175,1.,-0.181307740731786));
#53421=CARTESIAN_POINT('Ctrl Pts',(-3.91812876180926,1.,-0.179515885822882));
#53422=CARTESIAN_POINT('Ctrl Pts',(-3.92543942697655,1.,-0.177674246152317));
#53423=CARTESIAN_POINT('Ctrl Pts',(-3.93275726771042,1.,-0.175783136893868));
#53424=CARTESIAN_POINT('Ctrl Pts',(-3.94007083096217,1.,-0.17384273497461));
#53425=CARTESIAN_POINT('Ctrl Pts',(-3.94737164900868,1.,-0.17185335536924));
#53426=CARTESIAN_POINT('Ctrl Pts',(-3.95465744665268,1.,-0.169815666374139));
#53427=CARTESIAN_POINT('Ctrl Pts',(-3.96192990160296,1.,-0.167730547023319));
#53428=CARTESIAN_POINT('Ctrl Pts',(-3.96919313621407,1.,-0.165598992851102));
#53429=CARTESIAN_POINT('Ctrl Pts',(-3.97645194630943,1.,-0.163422004609999));
#53430=CARTESIAN_POINT('Ctrl Pts',(-3.98371010319872,1.,-0.161200482186085));
#53431=CARTESIAN_POINT('Ctrl Pts',(-3.99096873945878,1.,-0.158935123982793));
#53432=CARTESIAN_POINT('Ctrl Pts',(-3.99822717425893,1.,-0.156626481393734));
#53433=CARTESIAN_POINT('Ctrl Pts',(-4.00548360245319,1.,-0.154275004872311));
#53434=CARTESIAN_POINT('Ctrl Pts',(-4.01273584234689,1.,-0.151881094022911));
#53435=CARTESIAN_POINT('Ctrl Pts',(-4.01998203715564,1.,-0.149445144968707));
#53436=CARTESIAN_POINT('Ctrl Pts',(-4.02722143146994,1.,-0.146967602878994));
#53437=CARTESIAN_POINT('Ctrl Pts',(-4.03445411510333,1.,-0.144448947038345));
#53438=CARTESIAN_POINT('Ctrl Pts',(-4.04168069633781,1.,-0.1418896714855));
#53439=CARTESIAN_POINT('Ctrl Pts',(-4.04890199238036,1.,-0.139290267180057));
#53440=CARTESIAN_POINT('Ctrl Pts',(-4.05611873400172,1.,-0.136651205046119));
#53441=CARTESIAN_POINT('Ctrl Pts',(-4.06333121018596,1.,-0.133972916144245));
#53442=CARTESIAN_POINT('Ctrl Pts',(-4.0705393152874,1.,-0.13125579354894));
#53443=CARTESIAN_POINT('Ctrl Pts',(-4.07774270738954,1.,-0.128500200484838));
#53444=CARTESIAN_POINT('Ctrl Pts',(-4.08494093372377,1.,-0.12570647682254));
#53445=CARTESIAN_POINT('Ctrl Pts',(-4.09213355850756,1.,-0.122874946249107));
#53446=CARTESIAN_POINT('Ctrl Pts',(-4.09932031767002,1.,-0.120005924388124));
#53447=CARTESIAN_POINT('Ctrl Pts',(-4.10650113381833,1.,-0.117099722731648));
#53448=CARTESIAN_POINT('Ctrl Pts',(-4.11367603924961,1.,-0.114156649609546));
#53449=CARTESIAN_POINT('Ctrl Pts',(-4.1208451250225,1.,-0.111177012683347));
#53450=CARTESIAN_POINT('Ctrl Pts',(-4.12800848371504,1.,-0.108161120528369));
#53451=CARTESIAN_POINT('Ctrl Pts',(-4.13516614458895,1.,-0.105109286538945));
#53452=CARTESIAN_POINT('Ctrl Pts',(-4.14231804939538,1.,-0.102021826577584));
#53453=CARTESIAN_POINT('Ctrl Pts',(-4.14946408918485,1.,-0.0988990478901226));
#53454=CARTESIAN_POINT('Ctrl Pts',(-4.15660412653577,1.,-0.0957412403298007));
#53455=CARTESIAN_POINT('Ctrl Pts',(-4.16373802265839,1.,-0.0925486672167531));
#53456=CARTESIAN_POINT('Ctrl Pts',(-4.17086566490794,1.,-0.0893215560848649));
#53457=CARTESIAN_POINT('Ctrl Pts',(-4.17798698668094,1.,-0.0860600915549397));
#53458=CARTESIAN_POINT('Ctrl Pts',(-4.18510195327123,1.,-0.0827644164385679));
#53459=CARTESIAN_POINT('Ctrl Pts',(-4.19078883320504,1.,-0.080100588711432));
#53460=CARTESIAN_POINT('Ctrl Pts',(-4.19505112859416,1.,-0.0780873956242397));
#53461=CARTESIAN_POINT('Ctrl Pts',(-4.1978913862118,1.,-0.0767384596141464));
#53462=CARTESIAN_POINT('Ctrl Pts',(-4.19931119685982,1.,-0.0760622897878246));
#53463=CARTESIAN_POINT('Origin',(-4.19931119685982,0.,-0.0760622897878246));
#53464=CARTESIAN_POINT('',(-4.19931119685982,1.,0.0760622897878236));
#53465=CARTESIAN_POINT('Origin',(0.,0.,0.));
#53466=CARTESIAN_POINT('',(-3.73017266276651,1.,-0.385112848330761));
#53467=CARTESIAN_POINT('Origin',(0.,1.,0.));
#53468=CARTESIAN_POINT('Ctrl Pts',(-3.73017266276651,1.,-0.385112848330762));
#53469=CARTESIAN_POINT('Ctrl Pts',(-3.73017266276651,0.666666666666667,
-0.385112848330762));
#53470=CARTESIAN_POINT('Ctrl Pts',(-3.73017266276651,0.333333333333333,
-0.385112848330762));
#53471=CARTESIAN_POINT('Ctrl Pts',(-3.73017266276651,-0.333333333333333,
-0.385112848330762));
#53472=CARTESIAN_POINT('Ctrl Pts',(-3.73017266276651,-0.666666666666667,
-0.385112848330762));
#53473=CARTESIAN_POINT('Ctrl Pts',(-3.73017266276651,-1.,-0.385112848330762));
#53474=CARTESIAN_POINT('Ctrl Pts',(-4.15950947128175,-1.,-0.581791163835815));
#53475=CARTESIAN_POINT('Ctrl Pts',(-4.15950947128175,1.,-0.581791163835815));
#53476=CARTESIAN_POINT('Ctrl Pts',(-4.1582129171283,-1.,-0.580901211463535));
#53477=CARTESIAN_POINT('Ctrl Pts',(-4.1582129171283,1.,-0.580901211463535));
#53478=CARTESIAN_POINT('Ctrl Pts',(-4.15561864788576,-1.,-0.579124568914235));
#53479=CARTESIAN_POINT('Ctrl Pts',(-4.15561864788576,1.,-0.579124568914235));
#53480=CARTESIAN_POINT('Ctrl Pts',(-4.151723761217,-1.,-0.576469391676688));
#53481=CARTESIAN_POINT('Ctrl Pts',(-4.151723761217,1.,-0.576469391676688));
#53482=CARTESIAN_POINT('Ctrl Pts',(-4.14652361068081,-1.,-0.572948736069522));
#53483=CARTESIAN_POINT('Ctrl Pts',(-4.14652361068081,1.,-0.572948736069522));
#53484=CARTESIAN_POINT('Ctrl Pts',(-4.14001179830547,-1.,-0.568580610189774));
#53485=CARTESIAN_POINT('Ctrl Pts',(-4.14001179830547,1.,-0.568580610189774));
#53486=CARTESIAN_POINT('Ctrl Pts',(-4.13348835727104,-1.,-0.564245279537148));
#53487=CARTESIAN_POINT('Ctrl Pts',(-4.13348835727104,1.,-0.564245279537148));
#53488=CARTESIAN_POINT('Ctrl Pts',(-4.12695329951961,-1.,-0.559942890594773));
#53489=CARTESIAN_POINT('Ctrl Pts',(-4.12695329951961,1.,-0.559942890594773));
#53490=CARTESIAN_POINT('Ctrl Pts',(-4.12040666195664,-1.,-0.555673636129977));
#53491=CARTESIAN_POINT('Ctrl Pts',(-4.12040666195664,1.,-0.555673636129977));
#53492=CARTESIAN_POINT('Ctrl Pts',(-4.11384852024721,-1.,-0.551437758497032));
#53493=CARTESIAN_POINT('Ctrl Pts',(-4.11384852024721,1.,-0.551437758497032));
#53494=CARTESIAN_POINT('Ctrl Pts',(-4.10727897027977,-1.,-0.547235539485637));
#53495=CARTESIAN_POINT('Ctrl Pts',(-4.10727897027977,1.,-0.547235539485637));
#53496=CARTESIAN_POINT('Ctrl Pts',(-4.10069810243979,-1.,-0.543067286877757));
#53497=CARTESIAN_POINT('Ctrl Pts',(-4.10069810243979,1.,-0.543067286877757));
#53498=CARTESIAN_POINT('Ctrl Pts',(-4.09410597627,-1.,-0.538933321179756));
#53499=CARTESIAN_POINT('Ctrl Pts',(-4.09410597627,1.,-0.538933321179756));
#53500=CARTESIAN_POINT('Ctrl Pts',(-4.08750259988885,-1.,-0.534833963477273));
#53501=CARTESIAN_POINT('Ctrl Pts',(-4.08750259988885,1.,-0.534833963477273));
#53502=CARTESIAN_POINT('Ctrl Pts',(-4.08088789536836,-1.,-0.530769518728571));
#53503=CARTESIAN_POINT('Ctrl Pts',(-4.08088789536836,1.,-0.530769518728571));
#53504=CARTESIAN_POINT('Ctrl Pts',(-4.07426172299847,-1.,-0.526740277227498));
#53505=CARTESIAN_POINT('Ctrl Pts',(-4.07426172299847,1.,-0.526740277227498));
#53506=CARTESIAN_POINT('Ctrl Pts',(-4.06762394471314,-1.,-0.522746528603107));
#53507=CARTESIAN_POINT('Ctrl Pts',(-4.06762394471314,1.,-0.522746528603107));
#53508=CARTESIAN_POINT('Ctrl Pts',(-4.06097448038013,-1.,-0.518788572336923));
#53509=CARTESIAN_POINT('Ctrl Pts',(-4.06097448038013,1.,-0.518788572336923));
#53510=CARTESIAN_POINT('Ctrl Pts',(-4.05431335771199,-1.,-0.514866728193017));
#53511=CARTESIAN_POINT('Ctrl Pts',(-4.05431335771199,1.,-0.514866728193017));
#53512=CARTESIAN_POINT('Ctrl Pts',(-4.04764078815447,-1.,-0.51098134921897));
#53513=CARTESIAN_POINT('Ctrl Pts',(-4.04764078815447,1.,-0.51098134921897));
#53514=CARTESIAN_POINT('Ctrl Pts',(-4.04095715148915,-1.,-0.507132823288136));
#53515=CARTESIAN_POINT('Ctrl Pts',(-4.04095715148915,1.,-0.507132823288136));
#53516=CARTESIAN_POINT('Ctrl Pts',(-4.03426284174272,-1.,-0.503321556915346));
#53517=CARTESIAN_POINT('Ctrl Pts',(-4.03426284174272,1.,-0.503321556915346));
#53518=CARTESIAN_POINT('Ctrl Pts',(-4.02755813980101,-1.,-0.499547962340821));
#53519=CARTESIAN_POINT('Ctrl Pts',(-4.02755813980101,1.,-0.499547962340821));
#53520=CARTESIAN_POINT('Ctrl Pts',(-4.02084308851832,-1.,-0.495812444326251));
#53521=CARTESIAN_POINT('Ctrl Pts',(-4.02084308851832,1.,-0.495812444326251));
#53522=CARTESIAN_POINT('Ctrl Pts',(-4.01411733503546,-1.,-0.492115383418018));
#53523=CARTESIAN_POINT('Ctrl Pts',(-4.01411733503546,1.,-0.492115383418018));
#53524=CARTESIAN_POINT('Ctrl Pts',(-4.0073800839099,-1.,-0.488457130424633));
#53525=CARTESIAN_POINT('Ctrl Pts',(-4.0073800839099,1.,-0.488457130424633));
#53526=CARTESIAN_POINT('Ctrl Pts',(-4.00063045119288,-1.,-0.484838042421835));
#53527=CARTESIAN_POINT('Ctrl Pts',(-4.00063045119288,1.,-0.484838042421835));
#53528=CARTESIAN_POINT('Ctrl Pts',(-3.99386775880679,-1.,-0.481258512209675));
#53529=CARTESIAN_POINT('Ctrl Pts',(-3.99386775880679,1.,-0.481258512209675));
#53530=CARTESIAN_POINT('Ctrl Pts',(-3.98709184306738,-1.,-0.477718999122027));
#53531=CARTESIAN_POINT('Ctrl Pts',(-3.98709184306738,1.,-0.477718999122027));
#53532=CARTESIAN_POINT('Ctrl Pts',(-3.98030338044409,-1.,-0.47422006101951));
#53533=CARTESIAN_POINT('Ctrl Pts',(-3.98030338044409,1.,-0.47422006101951));
#53534=CARTESIAN_POINT('Ctrl Pts',(-3.97350414289392,-1.,-0.470762379613439));
#53535=CARTESIAN_POINT('Ctrl Pts',(-3.97350414289392,1.,-0.470762379613439));
#53536=CARTESIAN_POINT('Ctrl Pts',(-3.9666962227393,-1.,-0.467346690880643));
#53537=CARTESIAN_POINT('Ctrl Pts',(-3.9666962227393,1.,-0.467346690880643));
#53538=CARTESIAN_POINT('Ctrl Pts',(-3.95988133243538,-1.,-0.463973722115733));
#53539=CARTESIAN_POINT('Ctrl Pts',(-3.95988133243538,1.,-0.463973722115733));
#53540=CARTESIAN_POINT('Ctrl Pts',(-3.95306005817364,-1.,-0.460644124429121));
#53541=CARTESIAN_POINT('Ctrl Pts',(-3.95306005817364,1.,-0.460644124429121));
#53542=CARTESIAN_POINT('Ctrl Pts',(-3.94623117206678,-1.,-0.457358410451683));
#53543=CARTESIAN_POINT('Ctrl Pts',(-3.94623117206678,1.,-0.457358410451683));
#53544=CARTESIAN_POINT('Ctrl Pts',(-3.93939080846298,-1.,-0.454116879027584));
#53545=CARTESIAN_POINT('Ctrl Pts',(-3.93939080846298,1.,-0.454116879027584));
#53546=CARTESIAN_POINT('Ctrl Pts',(-3.93253407403123,-1.,-0.450919768356348));
#53547=CARTESIAN_POINT('Ctrl Pts',(-3.93253407403123,1.,-0.450919768356348));
#53548=CARTESIAN_POINT('Ctrl Pts',(-3.92565674143416,-1.,-0.447767416837292));
#53549=CARTESIAN_POINT('Ctrl Pts',(-3.92565674143416,1.,-0.447767416837292));
#53550=CARTESIAN_POINT('Ctrl Pts',(-3.91875701610719,-1.,-0.444660430230591));
#53551=CARTESIAN_POINT('Ctrl Pts',(-3.91875701610719,1.,-0.444660430230591));
#53552=CARTESIAN_POINT('Ctrl Pts',(-3.91183704069153,-1.,-0.441599824524054));
#53553=CARTESIAN_POINT('Ctrl Pts',(-3.91183704069153,1.,-0.441599824524054));
#53554=CARTESIAN_POINT('Ctrl Pts',(-3.90490512938563,-1.,-0.438587235458249));
#53555=CARTESIAN_POINT('Ctrl Pts',(-3.90490512938563,1.,-0.438587235458249));
#53556=CARTESIAN_POINT('Ctrl Pts',(-3.89797256655462,-1.,-0.435624629433527));
#53557=CARTESIAN_POINT('Ctrl Pts',(-3.89797256655462,1.,-0.435624629433527));
#53558=CARTESIAN_POINT('Ctrl Pts',(-3.89104947940611,-1.,-0.432713929544458));
#53559=CARTESIAN_POINT('Ctrl Pts',(-3.89104947940611,1.,-0.432713929544458));
#53560=CARTESIAN_POINT('Ctrl Pts',(-3.88414070943341,-1.,-0.429856640579741));
#53561=CARTESIAN_POINT('Ctrl Pts',(-3.88414070943341,1.,-0.429856640579741));
#53562=CARTESIAN_POINT('Ctrl Pts',(-3.87724240306597,-1.,-0.427053541173457));
#53563=CARTESIAN_POINT('Ctrl Pts',(-3.87724240306597,1.,-0.427053541173457));
#53564=CARTESIAN_POINT('Ctrl Pts',(-3.87033643487851,-1.,-0.424304173195111));
#53565=CARTESIAN_POINT('Ctrl Pts',(-3.87033643487851,1.,-0.424304173195111));
#53566=CARTESIAN_POINT('Ctrl Pts',(-3.86339652542709,-1.,-0.421607423177534));
#53567=CARTESIAN_POINT('Ctrl Pts',(-3.86339652542709,1.,-0.421607423177534));
#53568=CARTESIAN_POINT('Ctrl Pts',(-3.85639825647996,-1.,-0.418962468086773));
#53569=CARTESIAN_POINT('Ctrl Pts',(-3.85639825647996,1.,-0.418962468086773));
#53570=CARTESIAN_POINT('Ctrl Pts',(-3.84932864157497,-1.,-0.416369678052907));
#53571=CARTESIAN_POINT('Ctrl Pts',(-3.84932864157497,1.,-0.416369678052907));
#53572=CARTESIAN_POINT('Ctrl Pts',(-3.84219403994762,-1.,-0.413831367016748));
#53573=CARTESIAN_POINT('Ctrl Pts',(-3.84219403994762,1.,-0.413831367016748));
#53574=CARTESIAN_POINT('Ctrl Pts',(-3.83503345578698,-1.,-0.411353038798518));
#53575=CARTESIAN_POINT('Ctrl Pts',(-3.83503345578698,1.,-0.411353038798518));
#53576=CARTESIAN_POINT('Ctrl Pts',(-3.82790724256471,-1.,-0.40894237144746));
#53577=CARTESIAN_POINT('Ctrl Pts',(-3.82790724256471,1.,-0.40894237144746));
#53578=CARTESIAN_POINT('Ctrl Pts',(-3.8208730391381,-1.,-0.406607038258985));
#53579=CARTESIAN_POINT('Ctrl Pts',(-3.8208730391381,1.,-0.406607038258985));
#53580=CARTESIAN_POINT('Ctrl Pts',(-3.81396374287793,-1.,-0.404352694628273));
#53581=CARTESIAN_POINT('Ctrl Pts',(-3.81396374287793,1.,-0.404352694628273));
#53582=CARTESIAN_POINT('Ctrl Pts',(-3.80716881962728,-1.,-0.402181320148436));
#53583=CARTESIAN_POINT('Ctrl Pts',(-3.80716881962728,1.,-0.402181320148436));
#53584=CARTESIAN_POINT('Ctrl Pts',(-3.80040370384546,-1.,-0.4000883465046));
#53585=CARTESIAN_POINT('Ctrl Pts',(-3.80040370384546,1.,-0.4000883465046));
#53586=CARTESIAN_POINT('Ctrl Pts',(-3.7935288716329,-1.,-0.398064818683969));
#53587=CARTESIAN_POINT('Ctrl Pts',(-3.7935288716329,1.,-0.398064818683969));
#53588=CARTESIAN_POINT('Ctrl Pts',(-3.78640521279313,-1.,-0.396103205334841));
#53589=CARTESIAN_POINT('Ctrl Pts',(-3.78640521279313,1.,-0.396103205334841));
#53590=CARTESIAN_POINT('Ctrl Pts',(-3.77894173114283,-1.,-0.394202481011499));
#53591=CARTESIAN_POINT('Ctrl Pts',(-3.77894173114283,1.,-0.394202481011499));
#53592=CARTESIAN_POINT('Ctrl Pts',(-3.77114011595967,-1.,-0.392372786223432));
#53593=CARTESIAN_POINT('Ctrl Pts',(-3.77114011595967,1.,-0.392372786223432));
#53594=CARTESIAN_POINT('Ctrl Pts',(-3.76315635033257,-1.,-0.39064207297956));
#53595=CARTESIAN_POINT('Ctrl Pts',(-3.76315635033257,1.,-0.39064207297956));
#53596=CARTESIAN_POINT('Ctrl Pts',(-3.75529302895152,-1.,-0.389054775898702));
#53597=CARTESIAN_POINT('Ctrl Pts',(-3.75529302895152,1.,-0.389054775898702));
#53598=CARTESIAN_POINT('Ctrl Pts',(-3.74792651696654,-1.,-0.387663020050836));
#53599=CARTESIAN_POINT('Ctrl Pts',(-3.74792651696654,1.,-0.387663020050836));
#53600=CARTESIAN_POINT('Ctrl Pts',(-3.74144965781276,-1.,-0.386519576222251));
#53601=CARTESIAN_POINT('Ctrl Pts',(-3.74144965781276,1.,-0.386519576222251));
#53602=CARTESIAN_POINT('Ctrl Pts',(-3.73621371845318,-1.,-0.385670806454566));
#53603=CARTESIAN_POINT('Ctrl Pts',(-3.73621371845318,1.,-0.385670806454566));
#53604=CARTESIAN_POINT('Ctrl Pts',(-3.73245705638843,-1.,-0.385147887988951));
#53605=CARTESIAN_POINT('Ctrl Pts',(-3.73245705638843,1.,-0.385147887988951));
#53606=CARTESIAN_POINT('Ctrl Pts',(-3.73072465900175,-1.,-0.385001870183213));
#53607=CARTESIAN_POINT('Ctrl Pts',(-3.73072465900175,1.,-0.385001870183213));
#53608=CARTESIAN_POINT('Ctrl Pts',(-3.73015851028356,-1.,-0.385047711603462));
#53609=CARTESIAN_POINT('Ctrl Pts',(-3.73015851028356,1.,-0.385047711603462));
#53610=CARTESIAN_POINT('Ctrl Pts',(-3.73010668803042,-1.,-0.385147278814642));
#53611=CARTESIAN_POINT('Ctrl Pts',(-3.73010668803042,1.,-0.385147278814642));
#53612=CARTESIAN_POINT('Ctrl Pts',(-3.73016218570874,-1.,-0.38521431477633));
#53613=CARTESIAN_POINT('Ctrl Pts',(-3.73016218570874,1.,-0.38521431477633));
#53614=CARTESIAN_POINT('',(-4.15950947128175,1.,-0.581791163835815));
#53615=CARTESIAN_POINT('Ctrl Pts',(-4.15950947128175,1.,-0.581791163835815));
#53616=CARTESIAN_POINT('Ctrl Pts',(-4.1582129171283,1.,-0.580901211463535));
#53617=CARTESIAN_POINT('Ctrl Pts',(-4.15561864788576,1.,-0.579124568914235));
#53618=CARTESIAN_POINT('Ctrl Pts',(-4.151723761217,1.,-0.576469391676688));
#53619=CARTESIAN_POINT('Ctrl Pts',(-4.14652361068081,1.,-0.572948736069522));
#53620=CARTESIAN_POINT('Ctrl Pts',(-4.14001179830547,1.,-0.568580610189774));
#53621=CARTESIAN_POINT('Ctrl Pts',(-4.13348835727104,1.,-0.564245279537148));
#53622=CARTESIAN_POINT('Ctrl Pts',(-4.12695329951961,1.,-0.559942890594773));
#53623=CARTESIAN_POINT('Ctrl Pts',(-4.12040666195664,1.,-0.555673636129977));
#53624=CARTESIAN_POINT('Ctrl Pts',(-4.11384852024721,1.,-0.551437758497032));
#53625=CARTESIAN_POINT('Ctrl Pts',(-4.10727897027977,1.,-0.547235539485637));
#53626=CARTESIAN_POINT('Ctrl Pts',(-4.10069810243979,1.,-0.543067286877757));
#53627=CARTESIAN_POINT('Ctrl Pts',(-4.09410597627,1.,-0.538933321179756));
#53628=CARTESIAN_POINT('Ctrl Pts',(-4.08750259988885,1.,-0.534833963477273));
#53629=CARTESIAN_POINT('Ctrl Pts',(-4.08088789536836,1.,-0.530769518728571));
#53630=CARTESIAN_POINT('Ctrl Pts',(-4.07426172299847,1.,-0.526740277227498));
#53631=CARTESIAN_POINT('Ctrl Pts',(-4.06762394471314,1.,-0.522746528603107));
#53632=CARTESIAN_POINT('Ctrl Pts',(-4.06097448038013,1.,-0.518788572336923));
#53633=CARTESIAN_POINT('Ctrl Pts',(-4.05431335771199,1.,-0.514866728193017));
#53634=CARTESIAN_POINT('Ctrl Pts',(-4.04764078815447,1.,-0.51098134921897));
#53635=CARTESIAN_POINT('Ctrl Pts',(-4.04095715148915,1.,-0.507132823288136));
#53636=CARTESIAN_POINT('Ctrl Pts',(-4.03426284174272,1.,-0.503321556915346));
#53637=CARTESIAN_POINT('Ctrl Pts',(-4.02755813980101,1.,-0.499547962340821));
#53638=CARTESIAN_POINT('Ctrl Pts',(-4.02084308851832,1.,-0.495812444326251));
#53639=CARTESIAN_POINT('Ctrl Pts',(-4.01411733503546,1.,-0.492115383418018));
#53640=CARTESIAN_POINT('Ctrl Pts',(-4.0073800839099,1.,-0.488457130424633));
#53641=CARTESIAN_POINT('Ctrl Pts',(-4.00063045119288,1.,-0.484838042421835));
#53642=CARTESIAN_POINT('Ctrl Pts',(-3.99386775880679,1.,-0.481258512209675));
#53643=CARTESIAN_POINT('Ctrl Pts',(-3.98709184306738,1.,-0.477718999122027));
#53644=CARTESIAN_POINT('Ctrl Pts',(-3.98030338044409,1.,-0.47422006101951));
#53645=CARTESIAN_POINT('Ctrl Pts',(-3.97350414289392,1.,-0.470762379613439));
#53646=CARTESIAN_POINT('Ctrl Pts',(-3.9666962227393,1.,-0.467346690880643));
#53647=CARTESIAN_POINT('Ctrl Pts',(-3.95988133243538,1.,-0.463973722115733));
#53648=CARTESIAN_POINT('Ctrl Pts',(-3.95306005817364,1.,-0.460644124429121));
#53649=CARTESIAN_POINT('Ctrl Pts',(-3.94623117206678,1.,-0.457358410451683));
#53650=CARTESIAN_POINT('Ctrl Pts',(-3.93939080846298,1.,-0.454116879027584));
#53651=CARTESIAN_POINT('Ctrl Pts',(-3.93253407403123,1.,-0.450919768356348));
#53652=CARTESIAN_POINT('Ctrl Pts',(-3.92565674143416,1.,-0.447767416837292));
#53653=CARTESIAN_POINT('Ctrl Pts',(-3.91875701610719,1.,-0.444660430230591));
#53654=CARTESIAN_POINT('Ctrl Pts',(-3.91183704069153,1.,-0.441599824524054));
#53655=CARTESIAN_POINT('Ctrl Pts',(-3.90490512938563,1.,-0.438587235458249));
#53656=CARTESIAN_POINT('Ctrl Pts',(-3.89797256655462,1.,-0.435624629433527));
#53657=CARTESIAN_POINT('Ctrl Pts',(-3.89104947940611,1.,-0.432713929544458));
#53658=CARTESIAN_POINT('Ctrl Pts',(-3.88414070943341,1.,-0.429856640579741));
#53659=CARTESIAN_POINT('Ctrl Pts',(-3.87724240306597,1.,-0.427053541173457));
#53660=CARTESIAN_POINT('Ctrl Pts',(-3.87033643487851,1.,-0.424304173195111));
#53661=CARTESIAN_POINT('Ctrl Pts',(-3.86339652542709,1.,-0.421607423177534));
#53662=CARTESIAN_POINT('Ctrl Pts',(-3.85639825647996,1.,-0.418962468086773));
#53663=CARTESIAN_POINT('Ctrl Pts',(-3.84932864157497,1.,-0.416369678052907));
#53664=CARTESIAN_POINT('Ctrl Pts',(-3.84219403994762,1.,-0.413831367016748));
#53665=CARTESIAN_POINT('Ctrl Pts',(-3.83503345578698,1.,-0.411353038798518));
#53666=CARTESIAN_POINT('Ctrl Pts',(-3.82790724256471,1.,-0.40894237144746));
#53667=CARTESIAN_POINT('Ctrl Pts',(-3.8208730391381,1.,-0.406607038258985));
#53668=CARTESIAN_POINT('Ctrl Pts',(-3.81396374287793,1.,-0.404352694628273));
#53669=CARTESIAN_POINT('Ctrl Pts',(-3.80716881962728,1.,-0.402181320148436));
#53670=CARTESIAN_POINT('Ctrl Pts',(-3.80040370384546,1.,-0.4000883465046));
#53671=CARTESIAN_POINT('Ctrl Pts',(-3.7935288716329,1.,-0.398064818683969));
#53672=CARTESIAN_POINT('Ctrl Pts',(-3.78640521279313,1.,-0.396103205334841));
#53673=CARTESIAN_POINT('Ctrl Pts',(-3.77894173114283,1.,-0.394202481011499));
#53674=CARTESIAN_POINT('Ctrl Pts',(-3.77114011595967,1.,-0.392372786223432));
#53675=CARTESIAN_POINT('Ctrl Pts',(-3.76315635033257,1.,-0.39064207297956));
#53676=CARTESIAN_POINT('Ctrl Pts',(-3.75529302895152,1.,-0.389054775898702));
#53677=CARTESIAN_POINT('Ctrl Pts',(-3.74792651696654,1.,-0.387663020050836));
#53678=CARTESIAN_POINT('Ctrl Pts',(-3.74144965781276,1.,-0.386519576222251));
#53679=CARTESIAN_POINT('Ctrl Pts',(-3.73621371845318,1.,-0.385670806454566));
#53680=CARTESIAN_POINT('Ctrl Pts',(-3.73273893363406,1.,-0.385187124634206));
#53681=CARTESIAN_POINT('Ctrl Pts',(-3.73106082862548,1.,-0.385031656499164));
#53682=CARTESIAN_POINT('Ctrl Pts',(-3.73040527621055,1.,-0.385037797881504));
#53683=CARTESIAN_POINT('Ctrl Pts',(-3.73021431755274,1.,-0.385087139000374));
#53684=CARTESIAN_POINT('Ctrl Pts',(-3.73017266276651,1.,-0.385112848330762));
#53685=CARTESIAN_POINT('',(-4.15950947128175,0.,-0.581791163835815));
#53686=CARTESIAN_POINT('Ctrl Pts',(-3.66663282329846,-1.,-0.7863229229206));
#53687=CARTESIAN_POINT('Ctrl Pts',(-3.66663282329846,1.,-0.7863229229206));
#53688=CARTESIAN_POINT('Ctrl Pts',(-3.66655932661986,-1.,-0.786369528183326));
#53689=CARTESIAN_POINT('Ctrl Pts',(-3.66655932661986,1.,-0.786369528183326));
#53690=CARTESIAN_POINT('Ctrl Pts',(-3.66657784455334,-1.,-0.786480236185696));
#53691=CARTESIAN_POINT('Ctrl Pts',(-3.66657784455334,1.,-0.786480236185696));
#53692=CARTESIAN_POINT('Ctrl Pts',(-3.66710211820482,-1.,-0.786698783542764));
#53693=CARTESIAN_POINT('Ctrl Pts',(-3.66710211820482,1.,-0.786698783542764));
#53694=CARTESIAN_POINT('Ctrl Pts',(-3.66879484801113,-1.,-0.787095252590501));
#53695=CARTESIAN_POINT('Ctrl Pts',(-3.66879484801113,1.,-0.787095252590501));
#53696=CARTESIAN_POINT('Ctrl Pts',(-3.67252923663655,-1.,-0.787758799995742));
#53697=CARTESIAN_POINT('Ctrl Pts',(-3.67252923663655,1.,-0.787758799995742));
#53698=CARTESIAN_POINT('Ctrl Pts',(-3.67777119516252,-1.,-0.788569566220285));
#53699=CARTESIAN_POINT('Ctrl Pts',(-3.67777119516252,1.,-0.788569566220285));
#53700=CARTESIAN_POINT('Ctrl Pts',(-3.68428439783905,-1.,-0.789483546064387));
#53701=CARTESIAN_POINT('Ctrl Pts',(-3.68428439783905,1.,-0.789483546064387));
#53702=CARTESIAN_POINT('Ctrl Pts',(-3.69172044327364,-1.,-0.790436284988787));
#53703=CARTESIAN_POINT('Ctrl Pts',(-3.69172044327364,1.,-0.790436284988787));
#53704=CARTESIAN_POINT('Ctrl Pts',(-3.69968940808721,-1.,-0.79135657569598));
#53705=CARTESIAN_POINT('Ctrl Pts',(-3.69968940808721,1.,-0.79135657569598));
#53706=CARTESIAN_POINT('Ctrl Pts',(-3.70781724021806,-1.,-0.792177688845818));
#53707=CARTESIAN_POINT('Ctrl Pts',(-3.70781724021806,1.,-0.792177688845818));
#53708=CARTESIAN_POINT('Ctrl Pts',(-3.71580242396124,-1.,-0.792848377370287));
#53709=CARTESIAN_POINT('Ctrl Pts',(-3.71580242396124,1.,-0.792848377370287));
#53710=CARTESIAN_POINT('Ctrl Pts',(-3.72348797293734,-1.,-0.793347023784205));
#53711=CARTESIAN_POINT('Ctrl Pts',(-3.72348797293734,1.,-0.793347023784205));
#53712=CARTESIAN_POINT('Ctrl Pts',(-3.73086914695805,-1.,-0.793682750269684));
#53713=CARTESIAN_POINT('Ctrl Pts',(-3.73086914695805,1.,-0.793682750269684));
#53714=CARTESIAN_POINT('Ctrl Pts',(-3.73803280541687,-1.,-0.793882700937017));
#53715=CARTESIAN_POINT('Ctrl Pts',(-3.73803280541687,1.,-0.793882700937017));
#53716=CARTESIAN_POINT('Ctrl Pts',(-3.74511357728861,-1.,-0.793982700459952));
#53717=CARTESIAN_POINT('Ctrl Pts',(-3.74511357728861,1.,-0.793982700459952));
#53718=CARTESIAN_POINT('Ctrl Pts',(-3.75224692493864,-1.,-0.794017347371377));
#53719=CARTESIAN_POINT('Ctrl Pts',(-3.75224692493864,1.,-0.794017347371377));
#53720=CARTESIAN_POINT('Ctrl Pts',(-3.75951468666257,-1.,-0.794008429134907));
#53721=CARTESIAN_POINT('Ctrl Pts',(-3.75951468666257,1.,-0.794008429134907));
#53722=CARTESIAN_POINT('Ctrl Pts',(-3.76692626931111,-1.,-0.793961083688991));
#53723=CARTESIAN_POINT('Ctrl Pts',(-3.76692626931111,1.,-0.793961083688991));
#53724=CARTESIAN_POINT('Ctrl Pts',(-3.77444863801212,-1.,-0.793870523787408));
#53725=CARTESIAN_POINT('Ctrl Pts',(-3.77444863801212,1.,-0.793870523787408));
#53726=CARTESIAN_POINT('Ctrl Pts',(-3.78202460377598,-1.,-0.7937262357813));
#53727=CARTESIAN_POINT('Ctrl Pts',(-3.78202460377598,1.,-0.7937262357813));
#53728=CARTESIAN_POINT('Ctrl Pts',(-3.78959439439235,-1.,-0.793516871680993));
#53729=CARTESIAN_POINT('Ctrl Pts',(-3.78959439439235,1.,-0.793516871680993));
#53730=CARTESIAN_POINT('Ctrl Pts',(-3.79711921389897,-1.,-0.793235612973273));
#53731=CARTESIAN_POINT('Ctrl Pts',(-3.79711921389897,1.,-0.793235612973273));
#53732=CARTESIAN_POINT('Ctrl Pts',(-3.80459229925637,-1.,-0.792882695234778));
#53733=CARTESIAN_POINT('Ctrl Pts',(-3.80459229925637,1.,-0.792882695234778));
#53734=CARTESIAN_POINT('Ctrl Pts',(-3.81202588694756,-1.,-0.792462483517634));
#53735=CARTESIAN_POINT('Ctrl Pts',(-3.81202588694756,1.,-0.792462483517634));
#53736=CARTESIAN_POINT('Ctrl Pts',(-3.81944345442249,-1.,-0.791981740718635));
#53737=CARTESIAN_POINT('Ctrl Pts',(-3.81944345442249,1.,-0.791981740718635));
#53738=CARTESIAN_POINT('Ctrl Pts',(-3.82687033899792,-1.,-0.791447528662369));
#53739=CARTESIAN_POINT('Ctrl Pts',(-3.82687033899792,1.,-0.791447528662369));
#53740=CARTESIAN_POINT('Ctrl Pts',(-3.83432392054786,-1.,-0.790865012705301));
#53741=CARTESIAN_POINT('Ctrl Pts',(-3.83432392054786,1.,-0.790865012705301));
#53742=CARTESIAN_POINT('Ctrl Pts',(-3.84180762342454,-1.,-0.790236124191242));
#53743=CARTESIAN_POINT('Ctrl Pts',(-3.84180762342454,1.,-0.790236124191242));
#53744=CARTESIAN_POINT('Ctrl Pts',(-3.84931637808894,-1.,-0.789560798155582));
#53745=CARTESIAN_POINT('Ctrl Pts',(-3.84931637808894,1.,-0.789560798155582));
#53746=CARTESIAN_POINT('Ctrl Pts',(-3.85683995872529,-1.,-0.788837734090672));
#53747=CARTESIAN_POINT('Ctrl Pts',(-3.85683995872529,1.,-0.788837734090672));
#53748=CARTESIAN_POINT('Ctrl Pts',(-3.86436702561345,-1.,-0.788065315093777));
#53749=CARTESIAN_POINT('Ctrl Pts',(-3.86436702561345,1.,-0.788065315093777));
#53750=CARTESIAN_POINT('Ctrl Pts',(-3.87188916600912,-1.,-0.787242527617999));
#53751=CARTESIAN_POINT('Ctrl Pts',(-3.87188916600912,1.,-0.787242527617999));
#53752=CARTESIAN_POINT('Ctrl Pts',(-3.8794040281819,-1.,-0.786369675812608));
#53753=CARTESIAN_POINT('Ctrl Pts',(-3.8794040281819,1.,-0.786369675812608));
#53754=CARTESIAN_POINT('Ctrl Pts',(-3.88691313167398,-1.,-0.78544789034073));
#53755=CARTESIAN_POINT('Ctrl Pts',(-3.88691313167398,1.,-0.78544789034073));
#53756=CARTESIAN_POINT('Ctrl Pts',(-3.89442039235103,-1.,-0.784478799358336));
#53757=CARTESIAN_POINT('Ctrl Pts',(-3.89442039235103,1.,-0.784478799358336));
#53758=CARTESIAN_POINT('Ctrl Pts',(-3.9019303904397,-1.,-0.783464141529081));
#53759=CARTESIAN_POINT('Ctrl Pts',(-3.9019303904397,1.,-0.783464141529081));
#53760=CARTESIAN_POINT('Ctrl Pts',(-3.90944671004542,-1.,-0.782405395622764));
#53761=CARTESIAN_POINT('Ctrl Pts',(-3.90944671004542,1.,-0.782405395622764));
#53762=CARTESIAN_POINT('Ctrl Pts',(-3.91697036054676,-1.,-0.781303428618366));
#53763=CARTESIAN_POINT('Ctrl Pts',(-3.91697036054676,1.,-0.781303428618366));
#53764=CARTESIAN_POINT('Ctrl Pts',(-3.92450058323823,-1.,-0.780158678615542));
#53765=CARTESIAN_POINT('Ctrl Pts',(-3.92450058323823,1.,-0.780158678615542));
#53766=CARTESIAN_POINT('Ctrl Pts',(-3.93203552473174,-1.,-0.778971308134821));
#53767=CARTESIAN_POINT('Ctrl Pts',(-3.93203552473174,1.,-0.778971308134821));
#53768=CARTESIAN_POINT('Ctrl Pts',(-3.93957296768103,-1.,-0.777741370568558));
#53769=CARTESIAN_POINT('Ctrl Pts',(-3.93957296768103,1.,-0.777741370568558));
#53770=CARTESIAN_POINT('Ctrl Pts',(-3.94711101619447,-1.,-0.776468966697921));
#53771=CARTESIAN_POINT('Ctrl Pts',(-3.94711101619447,1.,-0.776468966697921));
#53772=CARTESIAN_POINT('Ctrl Pts',(-3.9546488545231,-1.,-0.775154418039351));
#53773=CARTESIAN_POINT('Ctrl Pts',(-3.9546488545231,1.,-0.775154418039351));
#53774=CARTESIAN_POINT('Ctrl Pts',(-3.96218649639807,-1.,-0.773798212026565));
#53775=CARTESIAN_POINT('Ctrl Pts',(-3.96218649639807,1.,-0.773798212026565));
#53776=CARTESIAN_POINT('Ctrl Pts',(-3.96972446532772,-1.,-0.772400931772136));
#53777=CARTESIAN_POINT('Ctrl Pts',(-3.96972446532772,1.,-0.772400931772136));
#53778=CARTESIAN_POINT('Ctrl Pts',(-3.97726349165488,-1.,-0.770963190030471));
#53779=CARTESIAN_POINT('Ctrl Pts',(-3.97726349165488,1.,-0.770963190030471));
#53780=CARTESIAN_POINT('Ctrl Pts',(-3.98480422348451,-1.,-0.769485566245544));
#53781=CARTESIAN_POINT('Ctrl Pts',(-3.98480422348451,1.,-0.769485566245544));
#53782=CARTESIAN_POINT('Ctrl Pts',(-3.9923468788101,-1.,-0.767968531377915));
#53783=CARTESIAN_POINT('Ctrl Pts',(-3.9923468788101,1.,-0.767968531377915));
#53784=CARTESIAN_POINT('Ctrl Pts',(-3.99989129179622,-1.,-0.766412457136064));
#53785=CARTESIAN_POINT('Ctrl Pts',(-3.99989129179622,1.,-0.766412457136064));
#53786=CARTESIAN_POINT('Ctrl Pts',(-4.00743706791509,-1.,-0.764817648785197));
#53787=CARTESIAN_POINT('Ctrl Pts',(-4.00743706791509,1.,-0.764817648785197));
#53788=CARTESIAN_POINT('Ctrl Pts',(-4.01498370680496,-1.,-0.763184371182935));
#53789=CARTESIAN_POINT('Ctrl Pts',(-4.01498370680496,1.,-0.763184371182935));
#53790=CARTESIAN_POINT('Ctrl Pts',(-4.02253072741268,-1.,-0.761512875859804));
#53791=CARTESIAN_POINT('Ctrl Pts',(-4.02253072741268,1.,-0.761512875859804));
#53792=CARTESIAN_POINT('Ctrl Pts',(-4.03007781954412,-1.,-0.759803433243752));
#53793=CARTESIAN_POINT('Ctrl Pts',(-4.03007781954412,1.,-0.759803433243752));
#53794=CARTESIAN_POINT('Ctrl Pts',(-4.03762485803119,-1.,-0.758056338884944));
#53795=CARTESIAN_POINT('Ctrl Pts',(-4.03762485803119,1.,-0.758056338884944));
#53796=CARTESIAN_POINT('Ctrl Pts',(-4.04517182653997,-1.,-0.756271902369581));
#53797=CARTESIAN_POINT('Ctrl Pts',(-4.04517182653997,1.,-0.756271902369581));
#53798=CARTESIAN_POINT('Ctrl Pts',(-4.05271876687915,-1.,-0.754450441816078));
#53799=CARTESIAN_POINT('Ctrl Pts',(-4.05271876687915,1.,-0.754450441816078));
#53800=CARTESIAN_POINT('Ctrl Pts',(-4.06026572221515,-1.,-0.752592276483072));
#53801=CARTESIAN_POINT('Ctrl Pts',(-4.06026572221515,1.,-0.752592276483072));
#53802=CARTESIAN_POINT('Ctrl Pts',(-4.06781267242378,-1.,-0.750697720484036));
#53803=CARTESIAN_POINT('Ctrl Pts',(-4.06781267242378,1.,-0.750697720484036));
#53804=CARTESIAN_POINT('Ctrl Pts',(-4.07535951056152,-1.,-0.748767076680557));
#53805=CARTESIAN_POINT('Ctrl Pts',(-4.07535951056152,1.,-0.748767076680557));
#53806=CARTESIAN_POINT('Ctrl Pts',(-4.08290608095642,-1.,-0.746800631492315));
#53807=CARTESIAN_POINT('Ctrl Pts',(-4.08290608095642,1.,-0.746800631492315));
#53808=CARTESIAN_POINT('Ctrl Pts',(-4.09045220253573,-1.,-0.7447986497065));
#53809=CARTESIAN_POINT('Ctrl Pts',(-4.09045220253573,1.,-0.7447986497065));
#53810=CARTESIAN_POINT('Ctrl Pts',(-4.09799769702611,-1.,-0.742761369689841));
#53811=CARTESIAN_POINT('Ctrl Pts',(-4.09799769702611,1.,-0.742761369689841));
#53812=CARTESIAN_POINT('Ctrl Pts',(-4.10554241757547,-1.,-0.740688998553377));
#53813=CARTESIAN_POINT('Ctrl Pts',(-4.10554241757547,1.,-0.740688998553377));
#53814=CARTESIAN_POINT('Ctrl Pts',(-4.11308626951927,-1.,-0.738581708225844));
#53815=CARTESIAN_POINT('Ctrl Pts',(-4.11308626951927,1.,-0.738581708225844));
#53816=CARTESIAN_POINT('Ctrl Pts',(-4.120629196238,-1.,-0.736439634331345));
#53817=CARTESIAN_POINT('Ctrl Pts',(-4.120629196238,1.,-0.736439634331345));
#53818=CARTESIAN_POINT('Ctrl Pts',(-4.12666277570844,-1.,-0.734698226764092));
#53819=CARTESIAN_POINT('Ctrl Pts',(-4.12666277570844,1.,-0.734698226764092));
#53820=CARTESIAN_POINT('Ctrl Pts',(-4.13118752795207,-1.,-0.733376589323546));
#53821=CARTESIAN_POINT('Ctrl Pts',(-4.13118752795207,1.,-0.733376589323546));
#53822=CARTESIAN_POINT('Ctrl Pts',(-4.1342038373684,-1.,-0.732488575135159));
#53823=CARTESIAN_POINT('Ctrl Pts',(-4.1342038373684,1.,-0.732488575135159));
#53824=CARTESIAN_POINT('Ctrl Pts',(-4.13571194405636,-1.,-0.73204283740062));
#53825=CARTESIAN_POINT('Ctrl Pts',(-4.13571194405636,1.,-0.73204283740062));
#53826=CARTESIAN_POINT('',(-3.66661143271685,1.,-0.786422660831985));
#53827=CARTESIAN_POINT('Ctrl Pts',(-3.66661143271685,-1.,-0.786422660831985));
#53828=CARTESIAN_POINT('Ctrl Pts',(-3.66661143271685,-0.666666666666667,
-0.786422660831985));
#53829=CARTESIAN_POINT('Ctrl Pts',(-3.66661143271685,-0.333333333333333,
-0.786422660831985));
#53830=CARTESIAN_POINT('Ctrl Pts',(-3.66661143271685,0.333333333333333,
-0.786422660831985));
#53831=CARTESIAN_POINT('Ctrl Pts',(-3.66661143271685,0.666666666666667,
-0.786422660831985));
#53832=CARTESIAN_POINT('Ctrl Pts',(-3.66661143271685,1.,-0.786422660831985));
#53833=CARTESIAN_POINT('',(-4.13571194405636,1.,-0.73204283740062));
#53834=CARTESIAN_POINT('',(-4.13571194405636,0.,-0.73204283740062));
#53835=CARTESIAN_POINT('Ctrl Pts',(-3.66661143271685,1.,-0.786422660831985));
#53836=CARTESIAN_POINT('Ctrl Pts',(-3.6666431041522,1.,-0.786459983895432));
#53837=CARTESIAN_POINT('Ctrl Pts',(-3.66680946938292,1.,-0.786565919558984));
#53838=CARTESIAN_POINT('Ctrl Pts',(-3.66743103898702,1.,-0.786774337198062));
#53839=CARTESIAN_POINT('Ctrl Pts',(-3.66907505398677,1.,-0.787145041181545));
#53840=CARTESIAN_POINT('Ctrl Pts',(-3.67252923663655,1.,-0.787758799995742));
#53841=CARTESIAN_POINT('Ctrl Pts',(-3.67777119516252,1.,-0.788569566220285));
#53842=CARTESIAN_POINT('Ctrl Pts',(-3.68428439783905,1.,-0.789483546064387));
#53843=CARTESIAN_POINT('Ctrl Pts',(-3.69172044327364,1.,-0.790436284988787));
#53844=CARTESIAN_POINT('Ctrl Pts',(-3.69968940808721,1.,-0.79135657569598));
#53845=CARTESIAN_POINT('Ctrl Pts',(-3.70781724021806,1.,-0.792177688845818));
#53846=CARTESIAN_POINT('Ctrl Pts',(-3.71580242396124,1.,-0.792848377370287));
#53847=CARTESIAN_POINT('Ctrl Pts',(-3.72348797293734,1.,-0.793347023784205));
#53848=CARTESIAN_POINT('Ctrl Pts',(-3.73086914695805,1.,-0.793682750269684));
#53849=CARTESIAN_POINT('Ctrl Pts',(-3.73803280541687,1.,-0.793882700937017));
#53850=CARTESIAN_POINT('Ctrl Pts',(-3.74511357728861,1.,-0.793982700459952));
#53851=CARTESIAN_POINT('Ctrl Pts',(-3.75224692493864,1.,-0.794017347371377));
#53852=CARTESIAN_POINT('Ctrl Pts',(-3.75951468666257,1.,-0.794008429134907));
#53853=CARTESIAN_POINT('Ctrl Pts',(-3.76692626931111,1.,-0.793961083688991));
#53854=CARTESIAN_POINT('Ctrl Pts',(-3.77444863801212,1.,-0.793870523787408));
#53855=CARTESIAN_POINT('Ctrl Pts',(-3.78202460377598,1.,-0.7937262357813));
#53856=CARTESIAN_POINT('Ctrl Pts',(-3.78959439439235,1.,-0.793516871680993));
#53857=CARTESIAN_POINT('Ctrl Pts',(-3.79711921389897,1.,-0.793235612973273));
#53858=CARTESIAN_POINT('Ctrl Pts',(-3.80459229925637,1.,-0.792882695234778));
#53859=CARTESIAN_POINT('Ctrl Pts',(-3.81202588694756,1.,-0.792462483517634));
#53860=CARTESIAN_POINT('Ctrl Pts',(-3.81944345442249,1.,-0.791981740718635));
#53861=CARTESIAN_POINT('Ctrl Pts',(-3.82687033899792,1.,-0.791447528662369));
#53862=CARTESIAN_POINT('Ctrl Pts',(-3.83432392054786,1.,-0.790865012705301));
#53863=CARTESIAN_POINT('Ctrl Pts',(-3.84180762342454,1.,-0.790236124191242));
#53864=CARTESIAN_POINT('Ctrl Pts',(-3.84931637808894,1.,-0.789560798155582));
#53865=CARTESIAN_POINT('Ctrl Pts',(-3.85683995872529,1.,-0.788837734090672));
#53866=CARTESIAN_POINT('Ctrl Pts',(-3.86436702561345,1.,-0.788065315093777));
#53867=CARTESIAN_POINT('Ctrl Pts',(-3.87188916600912,1.,-0.787242527617999));
#53868=CARTESIAN_POINT('Ctrl Pts',(-3.8794040281819,1.,-0.786369675812608));
#53869=CARTESIAN_POINT('Ctrl Pts',(-3.88691313167398,1.,-0.78544789034073));
#53870=CARTESIAN_POINT('Ctrl Pts',(-3.89442039235103,1.,-0.784478799358336));
#53871=CARTESIAN_POINT('Ctrl Pts',(-3.9019303904397,1.,-0.783464141529081));
#53872=CARTESIAN_POINT('Ctrl Pts',(-3.90944671004542,1.,-0.782405395622764));
#53873=CARTESIAN_POINT('Ctrl Pts',(-3.91697036054676,1.,-0.781303428618366));
#53874=CARTESIAN_POINT('Ctrl Pts',(-3.92450058323823,1.,-0.780158678615542));
#53875=CARTESIAN_POINT('Ctrl Pts',(-3.93203552473174,1.,-0.778971308134821));
#53876=CARTESIAN_POINT('Ctrl Pts',(-3.93957296768103,1.,-0.777741370568558));
#53877=CARTESIAN_POINT('Ctrl Pts',(-3.94711101619447,1.,-0.776468966697921));
#53878=CARTESIAN_POINT('Ctrl Pts',(-3.9546488545231,1.,-0.775154418039351));
#53879=CARTESIAN_POINT('Ctrl Pts',(-3.96218649639807,1.,-0.773798212026565));
#53880=CARTESIAN_POINT('Ctrl Pts',(-3.96972446532772,1.,-0.772400931772136));
#53881=CARTESIAN_POINT('Ctrl Pts',(-3.97726349165488,1.,-0.770963190030471));
#53882=CARTESIAN_POINT('Ctrl Pts',(-3.98480422348451,1.,-0.769485566245544));
#53883=CARTESIAN_POINT('Ctrl Pts',(-3.9923468788101,1.,-0.767968531377915));
#53884=CARTESIAN_POINT('Ctrl Pts',(-3.99989129179622,1.,-0.766412457136064));
#53885=CARTESIAN_POINT('Ctrl Pts',(-4.00743706791509,1.,-0.764817648785197));
#53886=CARTESIAN_POINT('Ctrl Pts',(-4.01498370680496,1.,-0.763184371182935));
#53887=CARTESIAN_POINT('Ctrl Pts',(-4.02253072741268,1.,-0.761512875859804));
#53888=CARTESIAN_POINT('Ctrl Pts',(-4.03007781954412,1.,-0.759803433243752));
#53889=CARTESIAN_POINT('Ctrl Pts',(-4.03762485803119,1.,-0.758056338884944));
#53890=CARTESIAN_POINT('Ctrl Pts',(-4.04517182653997,1.,-0.756271902369581));
#53891=CARTESIAN_POINT('Ctrl Pts',(-4.05271876687915,1.,-0.754450441816078));
#53892=CARTESIAN_POINT('Ctrl Pts',(-4.06026572221515,1.,-0.752592276483072));
#53893=CARTESIAN_POINT('Ctrl Pts',(-4.06781267242378,1.,-0.750697720484036));
#53894=CARTESIAN_POINT('Ctrl Pts',(-4.07535951056152,1.,-0.748767076680557));
#53895=CARTESIAN_POINT('Ctrl Pts',(-4.08290608095642,1.,-0.746800631492315));
#53896=CARTESIAN_POINT('Ctrl Pts',(-4.09045220253573,1.,-0.7447986497065));
#53897=CARTESIAN_POINT('Ctrl Pts',(-4.09799769702611,1.,-0.742761369689841));
#53898=CARTESIAN_POINT('Ctrl Pts',(-4.10554241757547,1.,-0.740688998553377));
#53899=CARTESIAN_POINT('Ctrl Pts',(-4.11308626951927,1.,-0.738581708225844));
#53900=CARTESIAN_POINT('Ctrl Pts',(-4.120629196238,1.,-0.736439634331345));
#53901=CARTESIAN_POINT('Ctrl Pts',(-4.12666277570844,1.,-0.734698226764092));
#53902=CARTESIAN_POINT('Ctrl Pts',(-4.13118752795207,1.,-0.733376589323546));
#53903=CARTESIAN_POINT('Ctrl Pts',(-4.1342038373684,1.,-0.732488575135159));
#53904=CARTESIAN_POINT('Ctrl Pts',(-4.13571194405636,1.,-0.73204283740062));
#53905=CARTESIAN_POINT('Origin',(-4.13571194405636,0.,-0.73204283740062));
#53906=CARTESIAN_POINT('',(-4.15950947128175,1.,-0.581791163835815));
#53907=CARTESIAN_POINT('Origin',(0.,0.,0.));
#53908=CARTESIAN_POINT('',(-3.62400312501245,1.,-0.963899035117248));
#53909=CARTESIAN_POINT('Origin',(0.,1.,0.));
#53910=CARTESIAN_POINT('Ctrl Pts',(-3.62400312501245,1.,-0.963899035117249));
#53911=CARTESIAN_POINT('Ctrl Pts',(-3.62400312501245,0.666666666666667,
-0.963899035117249));
#53912=CARTESIAN_POINT('Ctrl Pts',(-3.62400312501245,0.333333333333333,
-0.963899035117249));
#53913=CARTESIAN_POINT('Ctrl Pts',(-3.62400312501245,-0.333333333333333,
-0.963899035117249));
#53914=CARTESIAN_POINT('Ctrl Pts',(-3.62400312501246,-0.666666666666667,
-0.963899035117249));
#53915=CARTESIAN_POINT('Ctrl Pts',(-3.62400312501246,-1.,-0.963899035117249));
#53916=CARTESIAN_POINT('Ctrl Pts',(-4.01728681790024,-1.,-1.22531898815164));
#53917=CARTESIAN_POINT('Ctrl Pts',(-4.01728681790024,1.,-1.22531898815164));
#53918=CARTESIAN_POINT('Ctrl Pts',(-4.0161454457032,-1.,-1.22423716681447));
#53919=CARTESIAN_POINT('Ctrl Pts',(-4.0161454457032,1.,-1.22423716681447));
#53920=CARTESIAN_POINT('Ctrl Pts',(-4.01386104434674,-1.,-1.22207656456199));
#53921=CARTESIAN_POINT('Ctrl Pts',(-4.01386104434674,1.,-1.22207656456199));
#53922=CARTESIAN_POINT('Ctrl Pts',(-4.01042947142681,-1.,-1.21884478244983));
#53923=CARTESIAN_POINT('Ctrl Pts',(-4.01042947142681,1.,-1.21884478244983));
#53924=CARTESIAN_POINT('Ctrl Pts',(-4.00584409524937,-1.,-1.21455398918813));
#53925=CARTESIAN_POINT('Ctrl Pts',(-4.00584409524937,1.,-1.21455398918813));
#53926=CARTESIAN_POINT('Ctrl Pts',(-4.00009577952534,-1.,-1.20922097030107));
#53927=CARTESIAN_POINT('Ctrl Pts',(-4.00009577952534,1.,-1.20922097030107));
#53928=CARTESIAN_POINT('Ctrl Pts',(-3.99433084800649,-1.,-1.2039185237544));
#53929=CARTESIAN_POINT('Ctrl Pts',(-3.99433084800649,1.,-1.2039185237544));
#53930=CARTESIAN_POINT('Ctrl Pts',(-3.98854928957287,-1.,-1.19864679609596));
#53931=CARTESIAN_POINT('Ctrl Pts',(-3.98854928957287,1.,-1.19864679609596));
#53932=CARTESIAN_POINT('Ctrl Pts',(-3.98275111052015,-1.,-1.19340598349307));
#53933=CARTESIAN_POINT('Ctrl Pts',(-3.98275111052015,1.,-1.19340598349307));
#53934=CARTESIAN_POINT('Ctrl Pts',(-3.97693634766926,-1.,-1.18819633715285));
#53935=CARTESIAN_POINT('Ctrl Pts',(-3.97693634766926,1.,-1.18819633715285));
#53936=CARTESIAN_POINT('Ctrl Pts',(-3.9711050516465,-1.,-1.18301815039596));
#53937=CARTESIAN_POINT('Ctrl Pts',(-3.9711050516465,1.,-1.18301815039596));
#53938=CARTESIAN_POINT('Ctrl Pts',(-3.96525726357682,-1.,-1.17787174135445));
#53939=CARTESIAN_POINT('Ctrl Pts',(-3.96525726357682,1.,-1.17787174135445));
#53940=CARTESIAN_POINT('Ctrl Pts',(-3.95939299213164,-1.,-1.17275743590327));
#53941=CARTESIAN_POINT('Ctrl Pts',(-3.95939299213164,1.,-1.17275743590327));
#53942=CARTESIAN_POINT('Ctrl Pts',(-3.95351219510062,-1.,-1.16767555244495));
#53943=CARTESIAN_POINT('Ctrl Pts',(-3.95351219510062,1.,-1.16767555244495));
#53944=CARTESIAN_POINT('Ctrl Pts',(-3.9476147478092,-1.,-1.16262637999261));
#53945=CARTESIAN_POINT('Ctrl Pts',(-3.9476147478092,1.,-1.16262637999261));
#53946=CARTESIAN_POINT('Ctrl Pts',(-3.94170046685542,-1.,-1.1576101834106));
#53947=CARTESIAN_POINT('Ctrl Pts',(-3.94170046685542,1.,-1.1576101834106));
#53948=CARTESIAN_POINT('Ctrl Pts',(-3.9357691705651,-1.,-1.1526272271639));
#53949=CARTESIAN_POINT('Ctrl Pts',(-3.9357691705651,1.,-1.1526272271639));
#53950=CARTESIAN_POINT('Ctrl Pts',(-3.92982073294334,-1.,-1.14767779451147));
#53951=CARTESIAN_POINT('Ctrl Pts',(-3.92982073294334,1.,-1.14767779451147));
#53952=CARTESIAN_POINT('Ctrl Pts',(-3.92385513133937,-1.,-1.14276220561575));
#53953=CARTESIAN_POINT('Ctrl Pts',(-3.92385513133937,1.,-1.14276220561575));
#53954=CARTESIAN_POINT('Ctrl Pts',(-3.91787251936688,-1.,-1.13788084225511));
#53955=CARTESIAN_POINT('Ctrl Pts',(-3.91787251936688,1.,-1.13788084225511));
#53956=CARTESIAN_POINT('Ctrl Pts',(-3.91187321145495,-1.,-1.13303414693849));
#53957=CARTESIAN_POINT('Ctrl Pts',(-3.91187321145495,1.,-1.13303414693849));
#53958=CARTESIAN_POINT('Ctrl Pts',(-3.90585753318622,-1.,-1.12822258281518));
#53959=CARTESIAN_POINT('Ctrl Pts',(-3.90585753318622,1.,-1.12822258281518));
#53960=CARTESIAN_POINT('Ctrl Pts',(-3.89982569749978,-1.,-1.12344660099029));
#53961=CARTESIAN_POINT('Ctrl Pts',(-3.89982569749978,1.,-1.12344660099029));
#53962=CARTESIAN_POINT('Ctrl Pts',(-3.89377768340362,-1.,-1.11870660794609));
#53963=CARTESIAN_POINT('Ctrl Pts',(-3.89377768340362,1.,-1.11870660794609));
#53964=CARTESIAN_POINT('Ctrl Pts',(-3.88771308285229,-1.,-1.11400292434447));
#53965=CARTESIAN_POINT('Ctrl Pts',(-3.88771308285229,1.,-1.11400292434447));
#53966=CARTESIAN_POINT('Ctrl Pts',(-3.88163105531791,-1.,-1.10933577224029));
#53967=CARTESIAN_POINT('Ctrl Pts',(-3.88163105531791,1.,-1.10933577224029));
#53968=CARTESIAN_POINT('Ctrl Pts',(-3.87553067187566,-1.,-1.10470536603303));
#53969=CARTESIAN_POINT('Ctrl Pts',(-3.87553067187566,1.,-1.10470536603303));
#53970=CARTESIAN_POINT('Ctrl Pts',(-3.86941120134872,-1.,-1.10011198761202));
#53971=CARTESIAN_POINT('Ctrl Pts',(-3.86941120134872,1.,-1.10011198761202));
#53972=CARTESIAN_POINT('Ctrl Pts',(-3.86327241021242,-1.,-1.09555606505012));
#53973=CARTESIAN_POINT('Ctrl Pts',(-3.86327241021242,1.,-1.09555606505012));
#53974=CARTESIAN_POINT('Ctrl Pts',(-3.85711487933911,-1.,-1.09103825516288));
#53975=CARTESIAN_POINT('Ctrl Pts',(-3.85711487933911,1.,-1.09103825516288));
#53976=CARTESIAN_POINT('Ctrl Pts',(-3.8509402522269,-1.,-1.08655950846377));
#53977=CARTESIAN_POINT('Ctrl Pts',(-3.8509402522269,1.,-1.08655950846377));
#53978=CARTESIAN_POINT('Ctrl Pts',(-3.84475048030615,-1.,-1.08212087917986));
#53979=CARTESIAN_POINT('Ctrl Pts',(-3.84475048030615,1.,-1.08212087917986));
#53980=CARTESIAN_POINT('Ctrl Pts',(-3.83854714117486,-1.,-1.07772335353856));
#53981=CARTESIAN_POINT('Ctrl Pts',(-3.83854714117486,1.,-1.07772335353856));
#53982=CARTESIAN_POINT('Ctrl Pts',(-3.83233071195145,-1.,-1.0733676663346));
#53983=CARTESIAN_POINT('Ctrl Pts',(-3.83233071195145,1.,-1.0733676663346));
#53984=CARTESIAN_POINT('Ctrl Pts',(-3.82609989967278,-1.,-1.0690541318036));
#53985=CARTESIAN_POINT('Ctrl Pts',(-3.82609989967278,1.,-1.0690541318036));
#53986=CARTESIAN_POINT('Ctrl Pts',(-3.81985083953012,-1.,-1.06478244038931));
#53987=CARTESIAN_POINT('Ctrl Pts',(-3.81985083953012,1.,-1.06478244038931));
#53988=CARTESIAN_POINT('Ctrl Pts',(-3.81357866117485,-1.,-1.06055206187298));
#53989=CARTESIAN_POINT('Ctrl Pts',(-3.81357866117485,1.,-1.06055206187298));
#53990=CARTESIAN_POINT('Ctrl Pts',(-3.80727913637784,-1.,-1.05636266918643));
#53991=CARTESIAN_POINT('Ctrl Pts',(-3.80727913637784,1.,-1.05636266918643));
#53992=CARTESIAN_POINT('Ctrl Pts',(-3.80095039790678,-1.,-1.05221457990015));
#53993=CARTESIAN_POINT('Ctrl Pts',(-3.80095039790678,1.,-1.05221457990015));
#53994=CARTESIAN_POINT('Ctrl Pts',(-3.79459440308793,-1.,-1.04810913267641));
#53995=CARTESIAN_POINT('Ctrl Pts',(-3.79459440308793,1.,-1.04810913267641));
#53996=CARTESIAN_POINT('Ctrl Pts',(-3.78821910787195,-1.,-1.04404924374426));
#53997=CARTESIAN_POINT('Ctrl Pts',(-3.78821910787195,1.,-1.04404924374426));
#53998=CARTESIAN_POINT('Ctrl Pts',(-3.78183535008192,-1.,-1.04003862055804));
#53999=CARTESIAN_POINT('Ctrl Pts',(-3.78183535008192,1.,-1.04003862055804));
#54000=CARTESIAN_POINT('Ctrl Pts',(-3.77545283140445,-1.,-1.03608074678013));
#54001=CARTESIAN_POINT('Ctrl Pts',(-3.77545283140445,1.,-1.03608074678013));
#54002=CARTESIAN_POINT('Ctrl Pts',(-3.76907609832522,-1.,-1.0321778660492));
#54003=CARTESIAN_POINT('Ctrl Pts',(-3.76907609832522,1.,-1.0321778660492));
#54004=CARTESIAN_POINT('Ctrl Pts',(-3.76270122291232,-1.,-1.02833014458181));
#54005=CARTESIAN_POINT('Ctrl Pts',(-3.76270122291232,1.,-1.02833014458181));
#54006=CARTESIAN_POINT('Ctrl Pts',(-3.75631037456194,-1.,-1.0245342944466));
#54007=CARTESIAN_POINT('Ctrl Pts',(-3.75631037456194,1.,-1.0245342944466));
#54008=CARTESIAN_POINT('Ctrl Pts',(-3.74987777155834,-1.,-1.02078510487428));
#54009=CARTESIAN_POINT('Ctrl Pts',(-3.74987777155834,1.,-1.02078510487428));
#54010=CARTESIAN_POINT('Ctrl Pts',(-3.74337942504959,-1.,-1.01707794311079));
#54011=CARTESIAN_POINT('Ctrl Pts',(-3.74337942504959,1.,-1.01707794311079));
#54012=CARTESIAN_POINT('Ctrl Pts',(-3.73680245055734,-1.,-1.01341114319903));
#54013=CARTESIAN_POINT('Ctrl Pts',(-3.73680245055734,1.,-1.01341114319903));
#54014=CARTESIAN_POINT('Ctrl Pts',(-3.73015276704426,-1.,-1.00978798539496));
#54015=CARTESIAN_POINT('Ctrl Pts',(-3.73015276704426,1.,-1.00978798539496));
#54016=CARTESIAN_POINT('Ctrl Pts',(-3.72346803750595,-1.,-1.0062200073571));
#54017=CARTESIAN_POINT('Ctrl Pts',(-3.72346803750595,1.,-1.0062200073571));
#54018=CARTESIAN_POINT('Ctrl Pts',(-3.71680667125118,-1.,-1.00272423396822));
#54019=CARTESIAN_POINT('Ctrl Pts',(-3.71680667125118,1.,-1.00272423396822));
#54020=CARTESIAN_POINT('Ctrl Pts',(-3.71022439713938,-1.,-0.99931726075653));
#54021=CARTESIAN_POINT('Ctrl Pts',(-3.71022439713938,1.,-0.99931726075653));
#54022=CARTESIAN_POINT('Ctrl Pts',(-3.70375282282138,-1.,-0.996009819772518));
#54023=CARTESIAN_POINT('Ctrl Pts',(-3.70375282282138,1.,-0.996009819772518));
#54024=CARTESIAN_POINT('Ctrl Pts',(-3.69738123415662,-1.,-0.99280221833201));
#54025=CARTESIAN_POINT('Ctrl Pts',(-3.69738123415662,1.,-0.99280221833201));
#54026=CARTESIAN_POINT('Ctrl Pts',(-3.69102682138846,-1.,-0.989676715398558));
#54027=CARTESIAN_POINT('Ctrl Pts',(-3.69102682138846,1.,-0.989676715398558));
#54028=CARTESIAN_POINT('Ctrl Pts',(-3.68455317926068,-1.,-0.986602639863837));
#54029=CARTESIAN_POINT('Ctrl Pts',(-3.68455317926068,1.,-0.986602639863837));
#54030=CARTESIAN_POINT('Ctrl Pts',(-3.67782408841715,-1.,-0.983550791470419));
#54031=CARTESIAN_POINT('Ctrl Pts',(-3.67782408841715,1.,-0.983550791470419));
#54032=CARTESIAN_POINT('Ctrl Pts',(-3.67074983340361,-1.,-0.980505922458267));
#54033=CARTESIAN_POINT('Ctrl Pts',(-3.67074983340361,1.,-0.980505922458267));
#54034=CARTESIAN_POINT('Ctrl Pts',(-3.66333049637475,-1.,-0.977478312751618));
#54035=CARTESIAN_POINT('Ctrl Pts',(-3.66333049637475,1.,-0.977478312751618));
#54036=CARTESIAN_POINT('Ctrl Pts',(-3.65571576735126,-1.,-0.974519971354848));
#54037=CARTESIAN_POINT('Ctrl Pts',(-3.65571576735126,1.,-0.974519971354848));
#54038=CARTESIAN_POINT('Ctrl Pts',(-3.64819756447455,-1.,-0.971722122061341));
#54039=CARTESIAN_POINT('Ctrl Pts',(-3.64819756447455,1.,-0.971722122061341));
#54040=CARTESIAN_POINT('Ctrl Pts',(-3.64113946505766,-1.,-0.969195124675865));
#54041=CARTESIAN_POINT('Ctrl Pts',(-3.64113946505766,1.,-0.969195124675865));
#54042=CARTESIAN_POINT('Ctrl Pts',(-3.63492122081143,-1.,-0.967052554541385));
#54043=CARTESIAN_POINT('Ctrl Pts',(-3.63492122081143,1.,-0.967052554541385));
#54044=CARTESIAN_POINT('Ctrl Pts',(-3.62988252139846,-1.,-0.965395153165293));
#54045=CARTESIAN_POINT('Ctrl Pts',(-3.62988252139846,1.,-0.965395153165293));
#54046=CARTESIAN_POINT('Ctrl Pts',(-3.62625391254797,-1.,-0.964291001273287));
#54047=CARTESIAN_POINT('Ctrl Pts',(-3.62625391254797,1.,-0.964291001273287));
#54048=CARTESIAN_POINT('Ctrl Pts',(-3.6245656860652,-1.,-0.963875774530619));
#54049=CARTESIAN_POINT('Ctrl Pts',(-3.6245656860652,1.,-0.963875774530619));
#54050=CARTESIAN_POINT('Ctrl Pts',(-3.62399933639914,-1.,-0.963832486395051));
#54051=CARTESIAN_POINT('Ctrl Pts',(-3.62399933639914,1.,-0.963832486395051));
#54052=CARTESIAN_POINT('Ctrl Pts',(-3.62393257642052,-1.,-0.963922720982193));
#54053=CARTESIAN_POINT('Ctrl Pts',(-3.62393257642052,1.,-0.963922720982193));
#54054=CARTESIAN_POINT('Ctrl Pts',(-3.62397690409552,-1.,-0.963997613369571));
#54055=CARTESIAN_POINT('Ctrl Pts',(-3.62397690409552,1.,-0.963997613369571));
#54056=CARTESIAN_POINT('',(-4.01728681790024,1.,-1.22531898815164));
#54057=CARTESIAN_POINT('Ctrl Pts',(-4.01728681790024,1.,-1.22531898815164));
#54058=CARTESIAN_POINT('Ctrl Pts',(-4.0161454457032,1.,-1.22423716681447));
#54059=CARTESIAN_POINT('Ctrl Pts',(-4.01386104434674,1.,-1.22207656456199));
#54060=CARTESIAN_POINT('Ctrl Pts',(-4.01042947142681,1.,-1.21884478244983));
#54061=CARTESIAN_POINT('Ctrl Pts',(-4.00584409524937,1.,-1.21455398918813));
#54062=CARTESIAN_POINT('Ctrl Pts',(-4.00009577952534,1.,-1.20922097030107));
#54063=CARTESIAN_POINT('Ctrl Pts',(-3.99433084800649,1.,-1.2039185237544));
#54064=CARTESIAN_POINT('Ctrl Pts',(-3.98854928957287,1.,-1.19864679609596));
#54065=CARTESIAN_POINT('Ctrl Pts',(-3.98275111052015,1.,-1.19340598349307));
#54066=CARTESIAN_POINT('Ctrl Pts',(-3.97693634766926,1.,-1.18819633715285));
#54067=CARTESIAN_POINT('Ctrl Pts',(-3.9711050516465,1.,-1.18301815039596));
#54068=CARTESIAN_POINT('Ctrl Pts',(-3.96525726357682,1.,-1.17787174135445));
#54069=CARTESIAN_POINT('Ctrl Pts',(-3.95939299213164,1.,-1.17275743590327));
#54070=CARTESIAN_POINT('Ctrl Pts',(-3.95351219510062,1.,-1.16767555244495));
#54071=CARTESIAN_POINT('Ctrl Pts',(-3.9476147478092,1.,-1.16262637999261));
#54072=CARTESIAN_POINT('Ctrl Pts',(-3.94170046685542,1.,-1.1576101834106));
#54073=CARTESIAN_POINT('Ctrl Pts',(-3.9357691705651,1.,-1.1526272271639));
#54074=CARTESIAN_POINT('Ctrl Pts',(-3.92982073294334,1.,-1.14767779451147));
#54075=CARTESIAN_POINT('Ctrl Pts',(-3.92385513133937,1.,-1.14276220561575));
#54076=CARTESIAN_POINT('Ctrl Pts',(-3.91787251936688,1.,-1.13788084225511));
#54077=CARTESIAN_POINT('Ctrl Pts',(-3.91187321145495,1.,-1.13303414693849));
#54078=CARTESIAN_POINT('Ctrl Pts',(-3.90585753318622,1.,-1.12822258281518));
#54079=CARTESIAN_POINT('Ctrl Pts',(-3.89982569749978,1.,-1.12344660099029));
#54080=CARTESIAN_POINT('Ctrl Pts',(-3.89377768340362,1.,-1.11870660794609));
#54081=CARTESIAN_POINT('Ctrl Pts',(-3.88771308285229,1.,-1.11400292434447));
#54082=CARTESIAN_POINT('Ctrl Pts',(-3.88163105531791,1.,-1.10933577224029));
#54083=CARTESIAN_POINT('Ctrl Pts',(-3.87553067187566,1.,-1.10470536603303));
#54084=CARTESIAN_POINT('Ctrl Pts',(-3.86941120134872,1.,-1.10011198761202));
#54085=CARTESIAN_POINT('Ctrl Pts',(-3.86327241021242,1.,-1.09555606505012));
#54086=CARTESIAN_POINT('Ctrl Pts',(-3.85711487933911,1.,-1.09103825516288));
#54087=CARTESIAN_POINT('Ctrl Pts',(-3.8509402522269,1.,-1.08655950846377));
#54088=CARTESIAN_POINT('Ctrl Pts',(-3.84475048030615,1.,-1.08212087917986));
#54089=CARTESIAN_POINT('Ctrl Pts',(-3.83854714117486,1.,-1.07772335353856));
#54090=CARTESIAN_POINT('Ctrl Pts',(-3.83233071195145,1.,-1.0733676663346));
#54091=CARTESIAN_POINT('Ctrl Pts',(-3.82609989967278,1.,-1.0690541318036));
#54092=CARTESIAN_POINT('Ctrl Pts',(-3.81985083953012,1.,-1.06478244038931));
#54093=CARTESIAN_POINT('Ctrl Pts',(-3.81357866117485,1.,-1.06055206187298));
#54094=CARTESIAN_POINT('Ctrl Pts',(-3.80727913637784,1.,-1.05636266918643));
#54095=CARTESIAN_POINT('Ctrl Pts',(-3.80095039790678,1.,-1.05221457990015));
#54096=CARTESIAN_POINT('Ctrl Pts',(-3.79459440308793,1.,-1.04810913267641));
#54097=CARTESIAN_POINT('Ctrl Pts',(-3.78821910787195,1.,-1.04404924374426));
#54098=CARTESIAN_POINT('Ctrl Pts',(-3.78183535008192,1.,-1.04003862055804));
#54099=CARTESIAN_POINT('Ctrl Pts',(-3.77545283140445,1.,-1.03608074678013));
#54100=CARTESIAN_POINT('Ctrl Pts',(-3.76907609832522,1.,-1.0321778660492));
#54101=CARTESIAN_POINT('Ctrl Pts',(-3.76270122291232,1.,-1.02833014458181));
#54102=CARTESIAN_POINT('Ctrl Pts',(-3.75631037456194,1.,-1.0245342944466));
#54103=CARTESIAN_POINT('Ctrl Pts',(-3.74987777155834,1.,-1.02078510487428));
#54104=CARTESIAN_POINT('Ctrl Pts',(-3.74337942504959,1.,-1.01707794311079));
#54105=CARTESIAN_POINT('Ctrl Pts',(-3.73680245055734,1.,-1.01341114319903));
#54106=CARTESIAN_POINT('Ctrl Pts',(-3.73015276704426,1.,-1.00978798539496));
#54107=CARTESIAN_POINT('Ctrl Pts',(-3.72346803750595,1.,-1.0062200073571));
#54108=CARTESIAN_POINT('Ctrl Pts',(-3.71680667125118,1.,-1.00272423396822));
#54109=CARTESIAN_POINT('Ctrl Pts',(-3.71022439713938,1.,-0.99931726075653));
#54110=CARTESIAN_POINT('Ctrl Pts',(-3.70375282282138,1.,-0.996009819772518));
#54111=CARTESIAN_POINT('Ctrl Pts',(-3.69738123415662,1.,-0.99280221833201));
#54112=CARTESIAN_POINT('Ctrl Pts',(-3.69102682138846,1.,-0.989676715398558));
#54113=CARTESIAN_POINT('Ctrl Pts',(-3.68455317926068,1.,-0.986602639863837));
#54114=CARTESIAN_POINT('Ctrl Pts',(-3.67782408841715,1.,-0.983550791470419));
#54115=CARTESIAN_POINT('Ctrl Pts',(-3.67074983340361,1.,-0.980505922458267));
#54116=CARTESIAN_POINT('Ctrl Pts',(-3.66333049637475,1.,-0.977478312751618));
#54117=CARTESIAN_POINT('Ctrl Pts',(-3.65571576735126,1.,-0.974519971354848));
#54118=CARTESIAN_POINT('Ctrl Pts',(-3.64819756447455,1.,-0.971722122061341));
#54119=CARTESIAN_POINT('Ctrl Pts',(-3.64113946505766,1.,-0.969195124675865));
#54120=CARTESIAN_POINT('Ctrl Pts',(-3.63492122081143,1.,-0.967052554541385));
#54121=CARTESIAN_POINT('Ctrl Pts',(-3.62988252139846,1.,-0.965395153165293));
#54122=CARTESIAN_POINT('Ctrl Pts',(-3.62652618145335,1.,-0.964373850166458));
#54123=CARTESIAN_POINT('Ctrl Pts',(-3.62489305727662,1.,-0.963957782642843));
#54124=CARTESIAN_POINT('Ctrl Pts',(-3.62424461507588,1.,-0.963861297423241));
#54125=CARTESIAN_POINT('Ctrl Pts',(-3.6240482887845,1.,-0.963880158555582));
#54126=CARTESIAN_POINT('Ctrl Pts',(-3.62400312501245,1.,-0.963899035117249));
#54127=CARTESIAN_POINT('',(-4.01728681790024,0.,-1.22531898815164));
#54128=CARTESIAN_POINT('Ctrl Pts',(-3.49848248301936,-1.,-1.35022972712301));
#54129=CARTESIAN_POINT('Ctrl Pts',(-3.49848248301936,1.,-1.35022972712301));
#54130=CARTESIAN_POINT('Ctrl Pts',(-3.4984026005375,-1.,-1.35026426118402));
#54131=CARTESIAN_POINT('Ctrl Pts',(-3.4984026005375,1.,-1.35026426118402));
#54132=CARTESIAN_POINT('Ctrl Pts',(-3.49840357193736,-1.,-1.35037650303019));
#54133=CARTESIAN_POINT('Ctrl Pts',(-3.49840357193736,1.,-1.35037650303019));
#54134=CARTESIAN_POINT('Ctrl Pts',(-3.49888720257132,-1.,-1.35067437417483));
#54135=CARTESIAN_POINT('Ctrl Pts',(-3.49888720257132,1.,-1.35067437417483));
#54136=CARTESIAN_POINT('Ctrl Pts',(-3.5004970706414,-1.,-1.3513307633124));
#54137=CARTESIAN_POINT('Ctrl Pts',(-3.5004970706414,1.,-1.3513307633124));
#54138=CARTESIAN_POINT('Ctrl Pts',(-3.50408168106261,-1.,-1.35257032843486));
#54139=CARTESIAN_POINT('Ctrl Pts',(-3.50408168106261,1.,-1.35257032843486));
#54140=CARTESIAN_POINT('Ctrl Pts',(-3.50913227059999,-1.,-1.35419113575956));
#54141=CARTESIAN_POINT('Ctrl Pts',(-3.50913227059999,1.,-1.35419113575956));
#54142=CARTESIAN_POINT('Ctrl Pts',(-3.51542230699556,-1.,-1.35611275237152));
#54143=CARTESIAN_POINT('Ctrl Pts',(-3.51542230699556,1.,-1.35611275237152));
#54144=CARTESIAN_POINT('Ctrl Pts',(-3.52261776116748,-1.,-1.35821701528836));
#54145=CARTESIAN_POINT('Ctrl Pts',(-3.52261776116748,1.,-1.35821701528836));
#54146=CARTESIAN_POINT('Ctrl Pts',(-3.530344649616,-1.,-1.36037259643734));
#54147=CARTESIAN_POINT('Ctrl Pts',(-3.530344649616,1.,-1.36037259643734));
#54148=CARTESIAN_POINT('Ctrl Pts',(-3.53824396424961,-1.,-1.36245507339307));
#54149=CARTESIAN_POINT('Ctrl Pts',(-3.53824396424961,1.,-1.36245507339307));
#54150=CARTESIAN_POINT('Ctrl Pts',(-3.54602591832973,-1.,-1.36436666257597));
#54151=CARTESIAN_POINT('Ctrl Pts',(-3.54602591832973,1.,-1.36436666257597));
#54152=CARTESIAN_POINT('Ctrl Pts',(-3.55353883995949,-1.,-1.3660614545677));
#54153=CARTESIAN_POINT('Ctrl Pts',(-3.55353883995949,1.,-1.3660614545677));
#54154=CARTESIAN_POINT('Ctrl Pts',(-3.56077662028649,-1.,-1.36754771771233));
#54155=CARTESIAN_POINT('Ctrl Pts',(-3.56077662028649,1.,-1.36754771771233));
#54156=CARTESIAN_POINT('Ctrl Pts',(-3.5678208030466,-1.,-1.36886584973389));
#54157=CARTESIAN_POINT('Ctrl Pts',(-3.5678208030466,1.,-1.36886584973389));
#54158=CARTESIAN_POINT('Ctrl Pts',(-3.57479875549486,-1.,-1.37007229485659));
#54159=CARTESIAN_POINT('Ctrl Pts',(-3.57479875549486,1.,-1.37007229485659));
#54160=CARTESIAN_POINT('Ctrl Pts',(-3.58183885982715,-1.,-1.37122241663062));
#54161=CARTESIAN_POINT('Ctrl Pts',(-3.58183885982715,1.,-1.37122241663062));
#54162=CARTESIAN_POINT('Ctrl Pts',(-3.58901853846365,-1.,-1.37235053660976));
#54163=CARTESIAN_POINT('Ctrl Pts',(-3.58901853846365,1.,-1.37235053660976));
#54164=CARTESIAN_POINT('Ctrl Pts',(-3.59634627869048,-1.,-1.37346320103157));
#54165=CARTESIAN_POINT('Ctrl Pts',(-3.59634627869048,1.,-1.37346320103157));
#54166=CARTESIAN_POINT('Ctrl Pts',(-3.60379020123988,-1.,-1.37455051379623));
#54167=CARTESIAN_POINT('Ctrl Pts',(-3.60379020123988,1.,-1.37455051379623));
#54168=CARTESIAN_POINT('Ctrl Pts',(-3.61129546591064,-1.,-1.37559314436634));
#54169=CARTESIAN_POINT('Ctrl Pts',(-3.61129546591064,1.,-1.37559314436634));
#54170=CARTESIAN_POINT('Ctrl Pts',(-3.6188048116042,-1.,-1.37657053403107));
#54171=CARTESIAN_POINT('Ctrl Pts',(-3.6188048116042,1.,-1.37657053403107));
#54172=CARTESIAN_POINT('Ctrl Pts',(-3.62628098665145,-1.,-1.37746987919881));
#54173=CARTESIAN_POINT('Ctrl Pts',(-3.62628098665145,1.,-1.37746987919881));
#54174=CARTESIAN_POINT('Ctrl Pts',(-3.63371727442486,-1.,-1.37829035457339));
#54175=CARTESIAN_POINT('Ctrl Pts',(-3.63371727442486,1.,-1.37829035457339));
#54176=CARTESIAN_POINT('Ctrl Pts',(-3.64112507791141,-1.,-1.37903818567359));
#54177=CARTESIAN_POINT('Ctrl Pts',(-3.64112507791141,1.,-1.37903818567359));
#54178=CARTESIAN_POINT('Ctrl Pts',(-3.64852652756456,-1.,-1.37972372481603));
#54179=CARTESIAN_POINT('Ctrl Pts',(-3.64852652756456,1.,-1.37972372481603));
#54180=CARTESIAN_POINT('Ctrl Pts',(-3.6559455440439,-1.,-1.38035791051212));
#54181=CARTESIAN_POINT('Ctrl Pts',(-3.6559455440439,1.,-1.38035791051212));
#54182=CARTESIAN_POINT('Ctrl Pts',(-3.66339848520857,-1.,-1.38094856333552));
#54183=CARTESIAN_POINT('Ctrl Pts',(-3.66339848520857,1.,-1.38094856333552));
#54184=CARTESIAN_POINT('Ctrl Pts',(-3.67088843112262,-1.,-1.38149812653868));
#54185=CARTESIAN_POINT('Ctrl Pts',(-3.67088843112262,1.,-1.38149812653868));
#54186=CARTESIAN_POINT('Ctrl Pts',(-3.67841038482414,-1.,-1.3820057429062));
#54187=CARTESIAN_POINT('Ctrl Pts',(-3.67841038482414,1.,-1.3820057429062));
#54188=CARTESIAN_POINT('Ctrl Pts',(-3.68595444983837,-1.,-1.38246852827182));
#54189=CARTESIAN_POINT('Ctrl Pts',(-3.68595444983837,1.,-1.38246852827182));
#54190=CARTESIAN_POINT('Ctrl Pts',(-3.69350967899526,-1.,-1.3828831117165));
#54191=CARTESIAN_POINT('Ctrl Pts',(-3.69350967899526,1.,-1.3828831117165));
#54192=CARTESIAN_POINT('Ctrl Pts',(-3.701067921679,-1.,-1.38324717612865));
#54193=CARTESIAN_POINT('Ctrl Pts',(-3.701067921679,1.,-1.38324717612865));
#54194=CARTESIAN_POINT('Ctrl Pts',(-3.70862680753347,-1.,-1.38356065402124));
#54195=CARTESIAN_POINT('Ctrl Pts',(-3.70862680753347,1.,-1.38356065402124));
#54196=CARTESIAN_POINT('Ctrl Pts',(-3.7161876605181,-1.,-1.38382489984586));
#54197=CARTESIAN_POINT('Ctrl Pts',(-3.7161876605181,1.,-1.38382489984586));
#54198=CARTESIAN_POINT('Ctrl Pts',(-3.72375409358803,-1.,-1.3840421342895));
#54199=CARTESIAN_POINT('Ctrl Pts',(-3.72375409358803,1.,-1.3840421342895));
#54200=CARTESIAN_POINT('Ctrl Pts',(-3.73133035859282,-1.,-1.38421479111531));
#54201=CARTESIAN_POINT('Ctrl Pts',(-3.73133035859282,1.,-1.38421479111531));
#54202=CARTESIAN_POINT('Ctrl Pts',(-3.73891976418104,-1.,-1.38434489156458));
#54203=CARTESIAN_POINT('Ctrl Pts',(-3.73891976418104,1.,-1.38434489156458));
#54204=CARTESIAN_POINT('Ctrl Pts',(-3.74652317167876,-1.,-1.38443344984394));
#54205=CARTESIAN_POINT('Ctrl Pts',(-3.74652317167876,1.,-1.38443344984394));
#54206=CARTESIAN_POINT('Ctrl Pts',(-3.7541397631875,-1.,-1.38448077997163));
#54207=CARTESIAN_POINT('Ctrl Pts',(-3.7541397631875,1.,-1.38448077997163));
#54208=CARTESIAN_POINT('Ctrl Pts',(-3.76176768271367,-1.,-1.3844867525335));
#54209=CARTESIAN_POINT('Ctrl Pts',(-3.76176768271367,1.,-1.3844867525335));
#54210=CARTESIAN_POINT('Ctrl Pts',(-3.76940473185779,-1.,-1.38445107339518));
#54211=CARTESIAN_POINT('Ctrl Pts',(-3.76940473185779,1.,-1.38445107339518));
#54212=CARTESIAN_POINT('Ctrl Pts',(-3.77704902230418,-1.,-1.38437354551428));
#54213=CARTESIAN_POINT('Ctrl Pts',(-3.77704902230418,1.,-1.38437354551428));
#54214=CARTESIAN_POINT('Ctrl Pts',(-3.78469969805082,-1.,-1.38425435883756));
#54215=CARTESIAN_POINT('Ctrl Pts',(-3.78469969805082,1.,-1.38425435883756));
#54216=CARTESIAN_POINT('Ctrl Pts',(-3.79235669640841,-1.,-1.38409399694566));
#54217=CARTESIAN_POINT('Ctrl Pts',(-3.79235669640841,1.,-1.38409399694566));
#54218=CARTESIAN_POINT('Ctrl Pts',(-3.80002044322111,-1.,-1.38389311766682));
#54219=CARTESIAN_POINT('Ctrl Pts',(-3.80002044322111,1.,-1.38389311766682));
#54220=CARTESIAN_POINT('Ctrl Pts',(-3.80769156398411,-1.,-1.3836524404622));
#54221=CARTESIAN_POINT('Ctrl Pts',(-3.80769156398411,1.,-1.3836524404622));
#54222=CARTESIAN_POINT('Ctrl Pts',(-3.81537060817811,-1.,-1.38337263902782));
#54223=CARTESIAN_POINT('Ctrl Pts',(-3.81537060817811,1.,-1.38337263902782));
#54224=CARTESIAN_POINT('Ctrl Pts',(-3.82305771743829,-1.,-1.38305421262763));
#54225=CARTESIAN_POINT('Ctrl Pts',(-3.82305771743829,1.,-1.38305421262763));
#54226=CARTESIAN_POINT('Ctrl Pts',(-3.8307526698229,-1.,-1.38269750245138));
#54227=CARTESIAN_POINT('Ctrl Pts',(-3.8307526698229,1.,-1.38269750245138));
#54228=CARTESIAN_POINT('Ctrl Pts',(-3.83845502790746,-1.,-1.38230274828821));
#54229=CARTESIAN_POINT('Ctrl Pts',(-3.83845502790746,1.,-1.38230274828821));
#54230=CARTESIAN_POINT('Ctrl Pts',(-3.84616425605764,-1.,-1.38187013346109));
#54231=CARTESIAN_POINT('Ctrl Pts',(-3.84616425605764,1.,-1.38187013346109));
#54232=CARTESIAN_POINT('Ctrl Pts',(-3.85387983979481,-1.,-1.38139983115049));
#54233=CARTESIAN_POINT('Ctrl Pts',(-3.85387983979481,1.,-1.38139983115049));
#54234=CARTESIAN_POINT('Ctrl Pts',(-3.86160143043959,-1.,-1.38089205992989));
#54235=CARTESIAN_POINT('Ctrl Pts',(-3.86160143043959,1.,-1.38089205992989));
#54236=CARTESIAN_POINT('Ctrl Pts',(-3.86932885813068,-1.,-1.38034709213014));
#54237=CARTESIAN_POINT('Ctrl Pts',(-3.86932885813068,1.,-1.38034709213014));
#54238=CARTESIAN_POINT('Ctrl Pts',(-3.87706205830532,-1.,-1.37976523097073));
#54239=CARTESIAN_POINT('Ctrl Pts',(-3.87706205830532,1.,-1.37976523097073));
#54240=CARTESIAN_POINT('Ctrl Pts',(-3.88480102249277,-1.,-1.37914679719383));
#54241=CARTESIAN_POINT('Ctrl Pts',(-3.88480102249277,1.,-1.37914679719383));
#54242=CARTESIAN_POINT('Ctrl Pts',(-3.89254574338496,-1.,-1.3784921128802));
#54243=CARTESIAN_POINT('Ctrl Pts',(-3.89254574338496,1.,-1.3784921128802));
#54244=CARTESIAN_POINT('Ctrl Pts',(-3.90029615196727,-1.,-1.37780148512792));
#54245=CARTESIAN_POINT('Ctrl Pts',(-3.90029615196727,1.,-1.37780148512792));
#54246=CARTESIAN_POINT('Ctrl Pts',(-3.90805209523486,-1.,-1.3770751963402));
#54247=CARTESIAN_POINT('Ctrl Pts',(-3.90805209523486,1.,-1.3770751963402));
#54248=CARTESIAN_POINT('Ctrl Pts',(-3.91581337462644,-1.,-1.37631350505797));
#54249=CARTESIAN_POINT('Ctrl Pts',(-3.91581337462644,1.,-1.37631350505797));
#54250=CARTESIAN_POINT('Ctrl Pts',(-3.92357976987672,-1.,-1.37551664448242));
#54251=CARTESIAN_POINT('Ctrl Pts',(-3.92357976987672,1.,-1.37551664448242));
#54252=CARTESIAN_POINT('Ctrl Pts',(-3.93135106761844,-1.,-1.37468482215751));
#54253=CARTESIAN_POINT('Ctrl Pts',(-3.93135106761844,1.,-1.37468482215751));
#54254=CARTESIAN_POINT('Ctrl Pts',(-3.93912709040818,-1.,-1.37381821967165));
#54255=CARTESIAN_POINT('Ctrl Pts',(-3.93912709040818,1.,-1.37381821967165));
#54256=CARTESIAN_POINT('Ctrl Pts',(-3.94690771785133,-1.,-1.37291699202807));
#54257=CARTESIAN_POINT('Ctrl Pts',(-3.94690771785133,1.,-1.37291699202807));
#54258=CARTESIAN_POINT('Ctrl Pts',(-3.95469287280914,-1.,-1.37198126432386));
#54259=CARTESIAN_POINT('Ctrl Pts',(-3.95469287280914,1.,-1.37198126432386));
#54260=CARTESIAN_POINT('Ctrl Pts',(-3.96092458506535,-1.,-1.3712051561502));
#54261=CARTESIAN_POINT('Ctrl Pts',(-3.96092458506535,1.,-1.3712051561502));
#54262=CARTESIAN_POINT('Ctrl Pts',(-3.96560037974645,-1.,-1.37060761745635));
#54263=CARTESIAN_POINT('Ctrl Pts',(-3.96560037974645,1.,-1.37060761745635));
#54264=CARTESIAN_POINT('Ctrl Pts',(-3.9687184694131,-1.,-1.37020239094614));
#54265=CARTESIAN_POINT('Ctrl Pts',(-3.9687184694131,1.,-1.37020239094614));
#54266=CARTESIAN_POINT('Ctrl Pts',(-3.97027773754922,-1.,-1.36999806084572));
#54267=CARTESIAN_POINT('Ctrl Pts',(-3.97027773754922,1.,-1.36999806084572));
#54268=CARTESIAN_POINT('',(-3.4984457533445,1.,-1.35032489087101));
#54269=CARTESIAN_POINT('Ctrl Pts',(-3.4984457533445,-1.,-1.35032489087101));
#54270=CARTESIAN_POINT('Ctrl Pts',(-3.4984457533445,-0.666666666666667,
-1.35032489087101));
#54271=CARTESIAN_POINT('Ctrl Pts',(-3.4984457533445,-0.333333333333333,
-1.35032489087101));
#54272=CARTESIAN_POINT('Ctrl Pts',(-3.4984457533445,0.333333333333333,-1.35032489087101));
#54273=CARTESIAN_POINT('Ctrl Pts',(-3.4984457533445,0.666666666666667,-1.35032489087101));
#54274=CARTESIAN_POINT('Ctrl Pts',(-3.4984457533445,1.,-1.35032489087101));
#54275=CARTESIAN_POINT('',(-3.97027773754922,1.,-1.36999806084572));
#54276=CARTESIAN_POINT('',(-3.97027773754922,0.,-1.36999806084572));
#54277=CARTESIAN_POINT('Ctrl Pts',(-3.4984457533445,1.,-1.35032489087101));
#54278=CARTESIAN_POINT('Ctrl Pts',(-3.49847119623846,1.,-1.35036670892966));
#54279=CARTESIAN_POINT('Ctrl Pts',(-3.49861894124827,1.,-1.35049736560527));
#54280=CARTESIAN_POINT('Ctrl Pts',(-3.49920025459723,1.,-1.35080045218587));
#54281=CARTESIAN_POINT('Ctrl Pts',(-3.5007660381649,1.,-1.35142377279517));
#54282=CARTESIAN_POINT('Ctrl Pts',(-3.50408168106261,1.,-1.35257032843486));
#54283=CARTESIAN_POINT('Ctrl Pts',(-3.50913227059999,1.,-1.35419113575956));
#54284=CARTESIAN_POINT('Ctrl Pts',(-3.51542230699556,1.,-1.35611275237152));
#54285=CARTESIAN_POINT('Ctrl Pts',(-3.52261776116748,1.,-1.35821701528836));
#54286=CARTESIAN_POINT('Ctrl Pts',(-3.530344649616,1.,-1.36037259643734));
#54287=CARTESIAN_POINT('Ctrl Pts',(-3.53824396424961,1.,-1.36245507339307));
#54288=CARTESIAN_POINT('Ctrl Pts',(-3.54602591832973,1.,-1.36436666257597));
#54289=CARTESIAN_POINT('Ctrl Pts',(-3.55353883995949,1.,-1.3660614545677));
#54290=CARTESIAN_POINT('Ctrl Pts',(-3.56077662028649,1.,-1.36754771771233));
#54291=CARTESIAN_POINT('Ctrl Pts',(-3.5678208030466,1.,-1.36886584973389));
#54292=CARTESIAN_POINT('Ctrl Pts',(-3.57479875549486,1.,-1.37007229485659));
#54293=CARTESIAN_POINT('Ctrl Pts',(-3.58183885982715,1.,-1.37122241663062));
#54294=CARTESIAN_POINT('Ctrl Pts',(-3.58901853846365,1.,-1.37235053660976));
#54295=CARTESIAN_POINT('Ctrl Pts',(-3.59634627869048,1.,-1.37346320103157));
#54296=CARTESIAN_POINT('Ctrl Pts',(-3.60379020123988,1.,-1.37455051379623));
#54297=CARTESIAN_POINT('Ctrl Pts',(-3.61129546591064,1.,-1.37559314436634));
#54298=CARTESIAN_POINT('Ctrl Pts',(-3.6188048116042,1.,-1.37657053403107));
#54299=CARTESIAN_POINT('Ctrl Pts',(-3.62628098665145,1.,-1.37746987919881));
#54300=CARTESIAN_POINT('Ctrl Pts',(-3.63371727442486,1.,-1.37829035457339));
#54301=CARTESIAN_POINT('Ctrl Pts',(-3.64112507791141,1.,-1.37903818567359));
#54302=CARTESIAN_POINT('Ctrl Pts',(-3.64852652756456,1.,-1.37972372481603));
#54303=CARTESIAN_POINT('Ctrl Pts',(-3.6559455440439,1.,-1.38035791051212));
#54304=CARTESIAN_POINT('Ctrl Pts',(-3.66339848520857,1.,-1.38094856333552));
#54305=CARTESIAN_POINT('Ctrl Pts',(-3.67088843112262,1.,-1.38149812653868));
#54306=CARTESIAN_POINT('Ctrl Pts',(-3.67841038482414,1.,-1.3820057429062));
#54307=CARTESIAN_POINT('Ctrl Pts',(-3.68595444983837,1.,-1.38246852827182));
#54308=CARTESIAN_POINT('Ctrl Pts',(-3.69350967899526,1.,-1.3828831117165));
#54309=CARTESIAN_POINT('Ctrl Pts',(-3.701067921679,1.,-1.38324717612865));
#54310=CARTESIAN_POINT('Ctrl Pts',(-3.70862680753347,1.,-1.38356065402124));
#54311=CARTESIAN_POINT('Ctrl Pts',(-3.7161876605181,1.,-1.38382489984586));
#54312=CARTESIAN_POINT('Ctrl Pts',(-3.72375409358803,1.,-1.3840421342895));
#54313=CARTESIAN_POINT('Ctrl Pts',(-3.73133035859282,1.,-1.38421479111531));
#54314=CARTESIAN_POINT('Ctrl Pts',(-3.73891976418104,1.,-1.38434489156458));
#54315=CARTESIAN_POINT('Ctrl Pts',(-3.74652317167876,1.,-1.38443344984394));
#54316=CARTESIAN_POINT('Ctrl Pts',(-3.7541397631875,1.,-1.38448077997163));
#54317=CARTESIAN_POINT('Ctrl Pts',(-3.76176768271367,1.,-1.3844867525335));
#54318=CARTESIAN_POINT('Ctrl Pts',(-3.76940473185779,1.,-1.38445107339518));
#54319=CARTESIAN_POINT('Ctrl Pts',(-3.77704902230418,1.,-1.38437354551428));
#54320=CARTESIAN_POINT('Ctrl Pts',(-3.78469969805082,1.,-1.38425435883756));
#54321=CARTESIAN_POINT('Ctrl Pts',(-3.79235669640841,1.,-1.38409399694566));
#54322=CARTESIAN_POINT('Ctrl Pts',(-3.80002044322111,1.,-1.38389311766682));
#54323=CARTESIAN_POINT('Ctrl Pts',(-3.80769156398411,1.,-1.3836524404622));
#54324=CARTESIAN_POINT('Ctrl Pts',(-3.81537060817811,1.,-1.38337263902782));
#54325=CARTESIAN_POINT('Ctrl Pts',(-3.82305771743829,1.,-1.38305421262763));
#54326=CARTESIAN_POINT('Ctrl Pts',(-3.8307526698229,1.,-1.38269750245138));
#54327=CARTESIAN_POINT('Ctrl Pts',(-3.83845502790746,1.,-1.38230274828821));
#54328=CARTESIAN_POINT('Ctrl Pts',(-3.84616425605764,1.,-1.38187013346109));
#54329=CARTESIAN_POINT('Ctrl Pts',(-3.85387983979481,1.,-1.38139983115049));
#54330=CARTESIAN_POINT('Ctrl Pts',(-3.86160143043959,1.,-1.38089205992989));
#54331=CARTESIAN_POINT('Ctrl Pts',(-3.86932885813068,1.,-1.38034709213014));
#54332=CARTESIAN_POINT('Ctrl Pts',(-3.87706205830532,1.,-1.37976523097073));
#54333=CARTESIAN_POINT('Ctrl Pts',(-3.88480102249277,1.,-1.37914679719383));
#54334=CARTESIAN_POINT('Ctrl Pts',(-3.89254574338496,1.,-1.3784921128802));
#54335=CARTESIAN_POINT('Ctrl Pts',(-3.90029615196727,1.,-1.37780148512792));
#54336=CARTESIAN_POINT('Ctrl Pts',(-3.90805209523486,1.,-1.3770751963402));
#54337=CARTESIAN_POINT('Ctrl Pts',(-3.91581337462644,1.,-1.37631350505797));
#54338=CARTESIAN_POINT('Ctrl Pts',(-3.92357976987672,1.,-1.37551664448242));
#54339=CARTESIAN_POINT('Ctrl Pts',(-3.93135106761844,1.,-1.37468482215751));
#54340=CARTESIAN_POINT('Ctrl Pts',(-3.93912709040818,1.,-1.37381821967165));
#54341=CARTESIAN_POINT('Ctrl Pts',(-3.94690771785133,1.,-1.37291699202807));
#54342=CARTESIAN_POINT('Ctrl Pts',(-3.95469287280914,1.,-1.37198126432386));
#54343=CARTESIAN_POINT('Ctrl Pts',(-3.96092458506535,1.,-1.3712051561502));
#54344=CARTESIAN_POINT('Ctrl Pts',(-3.96560037974645,1.,-1.37060761745635));
#54345=CARTESIAN_POINT('Ctrl Pts',(-3.9687184694131,1.,-1.37020239094614));
#54346=CARTESIAN_POINT('Ctrl Pts',(-3.97027773754922,1.,-1.36999806084572));
#54347=CARTESIAN_POINT('Origin',(-3.97027773754922,0.,-1.36999806084572));
#54348=CARTESIAN_POINT('',(-4.01728681790024,1.,-1.22531898815164));
#54349=CARTESIAN_POINT('Origin',(0.,0.,0.));
#54350=CARTESIAN_POINT('',(-3.42859860294378,1.,-1.51895082866166));
#54351=CARTESIAN_POINT('Origin',(0.,1.,0.));
#54352=CARTESIAN_POINT('Ctrl Pts',(-3.42859860294378,1.,-1.51895082866166));
#54353=CARTESIAN_POINT('Ctrl Pts',(-3.42859860294378,0.666666666666667,
-1.51895082866166));
#54354=CARTESIAN_POINT('Ctrl Pts',(-3.42859860294378,0.333333333333333,
-1.51895082866166));
#54355=CARTESIAN_POINT('Ctrl Pts',(-3.42859860294378,-0.333333333333333,
-1.51895082866166));
#54356=CARTESIAN_POINT('Ctrl Pts',(-3.42859860294378,-0.666666666666667,
-1.51895082866166));
#54357=CARTESIAN_POINT('Ctrl Pts',(-3.42859860294378,-1.,-1.51895082866166));
#54358=CARTESIAN_POINT('Ctrl Pts',(-3.77614523045147,-1.,-1.83867539237861));
#54359=CARTESIAN_POINT('Ctrl Pts',(-3.77614523045147,1.,-1.83867539237861));
#54360=CARTESIAN_POINT('Ctrl Pts',(-3.77518714458232,-1.,-1.83742834010821));
#54361=CARTESIAN_POINT('Ctrl Pts',(-3.77518714458232,1.,-1.83742834010821));
#54362=CARTESIAN_POINT('Ctrl Pts',(-3.77326886065484,-1.,-1.83493697935064));
#54363=CARTESIAN_POINT('Ctrl Pts',(-3.77326886065484,1.,-1.83493697935064));
#54364=CARTESIAN_POINT('Ctrl Pts',(-3.77038509819777,-1.,-1.83120816956515));
#54365=CARTESIAN_POINT('Ctrl Pts',(-3.77038509819777,1.,-1.83120816956515));
#54366=CARTESIAN_POINT('Ctrl Pts',(-3.76652740355856,-1.,-1.82625289221933));
#54367=CARTESIAN_POINT('Ctrl Pts',(-3.76652740355856,1.,-1.82625289221933));
#54368=CARTESIAN_POINT('Ctrl Pts',(-3.76168412709652,-1.,-1.82008629694924));
#54369=CARTESIAN_POINT('Ctrl Pts',(-3.76168412709652,1.,-1.82008629694924));
#54370=CARTESIAN_POINT('Ctrl Pts',(-3.75681965683995,-1.,-1.81394729834032));
#54371=CARTESIAN_POINT('Ctrl Pts',(-3.75681965683995,1.,-1.81394729834032));
#54372=CARTESIAN_POINT('Ctrl Pts',(-3.75193395888069,-1.,-1.80783603939662));
#54373=CARTESIAN_POINT('Ctrl Pts',(-3.75193395888069,1.,-1.80783603939662));
#54374=CARTESIAN_POINT('Ctrl Pts',(-3.74702700874954,-1.,-1.80175271485519));
#54375=CARTESIAN_POINT('Ctrl Pts',(-3.74702700874954,1.,-1.80175271485519));
#54376=CARTESIAN_POINT('Ctrl Pts',(-3.74209880351667,-1.,-1.79569757859041));
#54377=CARTESIAN_POINT('Ctrl Pts',(-3.74209880351667,1.,-1.79569757859041));
#54378=CARTESIAN_POINT('Ctrl Pts',(-3.73714934729962,-1.,-1.78967092823139));
#54379=CARTESIAN_POINT('Ctrl Pts',(-3.73714934729962,1.,-1.78967092823139));
#54380=CARTESIAN_POINT('Ctrl Pts',(-3.73217863095022,-1.,-1.78367308442682));
#54381=CARTESIAN_POINT('Ctrl Pts',(-3.73217863095022,1.,-1.78367308442682));
#54382=CARTESIAN_POINT('Ctrl Pts',(-3.72718661205504,-1.,-1.77770437039606));
#54383=CARTESIAN_POINT('Ctrl Pts',(-3.72718661205504,1.,-1.77770437039606));
#54384=CARTESIAN_POINT('Ctrl Pts',(-3.72217319911429,-1.,-1.77176509401846));
#54385=CARTESIAN_POINT('Ctrl Pts',(-3.72217319911429,1.,-1.77176509401846));
#54386=CARTESIAN_POINT('Ctrl Pts',(-3.71713822377675,-1.,-1.76585552124549));
#54387=CARTESIAN_POINT('Ctrl Pts',(-3.71713822377675,1.,-1.76585552124549));
#54388=CARTESIAN_POINT('Ctrl Pts',(-3.71208146346454,-1.,-1.75997588499021));
#54389=CARTESIAN_POINT('Ctrl Pts',(-3.71208146346454,1.,-1.75997588499021));
#54390=CARTESIAN_POINT('Ctrl Pts',(-3.70700269736876,-1.,-1.75412641804148));
#54391=CARTESIAN_POINT('Ctrl Pts',(-3.70700269736876,1.,-1.75412641804148));
#54392=CARTESIAN_POINT('Ctrl Pts',(-3.70190175673422,-1.,-1.74830738046092));
#54393=CARTESIAN_POINT('Ctrl Pts',(-3.70190175673422,1.,-1.74830738046092));
#54394=CARTESIAN_POINT('Ctrl Pts',(-3.6967785691046,-1.,-1.74251908492589));
#54395=CARTESIAN_POINT('Ctrl Pts',(-3.6967785691046,1.,-1.74251908492589));
#54396=CARTESIAN_POINT('Ctrl Pts',(-3.69163322647906,-1.,-1.73676193254493));
#54397=CARTESIAN_POINT('Ctrl Pts',(-3.69163322647906,1.,-1.73676193254493));
#54398=CARTESIAN_POINT('Ctrl Pts',(-3.68646597019188,-1.,-1.73103640956647));
#54399=CARTESIAN_POINT('Ctrl Pts',(-3.68646597019188,1.,-1.73103640956647));
#54400=CARTESIAN_POINT('Ctrl Pts',(-3.68127704936472,-1.,-1.72534302437003));
#54401=CARTESIAN_POINT('Ctrl Pts',(-3.68127704936472,1.,-1.72534302437003));
#54402=CARTESIAN_POINT('Ctrl Pts',(-3.67606660374665,-1.,-1.71968225581787));
#54403=CARTESIAN_POINT('Ctrl Pts',(-3.67606660374665,1.,-1.71968225581787));
#54404=CARTESIAN_POINT('Ctrl Pts',(-3.67083454901629,-1.,-1.71405450210392));
#54405=CARTESIAN_POINT('Ctrl Pts',(-3.67083454901629,1.,-1.71405450210392));
#54406=CARTESIAN_POINT('Ctrl Pts',(-3.6655804319893,-1.,-1.70846001610983));
#54407=CARTESIAN_POINT('Ctrl Pts',(-3.6655804319893,1.,-1.70846001610983));
#54408=CARTESIAN_POINT('Ctrl Pts',(-3.6603033877491,-1.,-1.70289888566904));
#54409=CARTESIAN_POINT('Ctrl Pts',(-3.6603033877491,1.,-1.70289888566904));
#54410=CARTESIAN_POINT('Ctrl Pts',(-3.65500246526798,-1.,-1.69737117722558));
#54411=CARTESIAN_POINT('Ctrl Pts',(-3.65500246526798,1.,-1.69737117722558));
#54412=CARTESIAN_POINT('Ctrl Pts',(-3.64967689827393,-1.,-1.691877054817));
#54413=CARTESIAN_POINT('Ctrl Pts',(-3.64967689827393,1.,-1.691877054817));
#54414=CARTESIAN_POINT('Ctrl Pts',(-3.64432638915199,-1.,-1.68641690471455));
#54415=CARTESIAN_POINT('Ctrl Pts',(-3.64432638915199,1.,-1.68641690471455));
#54416=CARTESIAN_POINT('Ctrl Pts',(-3.63895140887443,-1.,-1.68099146651577));
#54417=CARTESIAN_POINT('Ctrl Pts',(-3.63895140887443,1.,-1.68099146651577));
#54418=CARTESIAN_POINT('Ctrl Pts',(-3.63355343201211,-1.,-1.67560193613145));
#54419=CARTESIAN_POINT('Ctrl Pts',(-3.63355343201211,1.,-1.67560193613145));
#54420=CARTESIAN_POINT('Ctrl Pts',(-3.62813422105257,-1.,-1.67024966008037));
#54421=CARTESIAN_POINT('Ctrl Pts',(-3.62813422105257,1.,-1.67024966008037));
#54422=CARTESIAN_POINT('Ctrl Pts',(-3.62269517989104,-1.,-1.66493585923853));
#54423=CARTESIAN_POINT('Ctrl Pts',(-3.62269517989104,1.,-1.66493585923853));
#54424=CARTESIAN_POINT('Ctrl Pts',(-3.61723666482457,-1.,-1.65966133399186));
#54425=CARTESIAN_POINT('Ctrl Pts',(-3.61723666482457,1.,-1.65966133399186));
#54426=CARTESIAN_POINT('Ctrl Pts',(-3.61175734965129,-1.,-1.65442619244327));
#54427=CARTESIAN_POINT('Ctrl Pts',(-3.61175734965129,1.,-1.65442619244327));
#54428=CARTESIAN_POINT('Ctrl Pts',(-3.60625346556992,-1.,-1.64922952425833));
#54429=CARTESIAN_POINT('Ctrl Pts',(-3.60625346556992,1.,-1.64922952425833));
#54430=CARTESIAN_POINT('Ctrl Pts',(-3.6007202851384,-1.,-1.6440700438558));
#54431=CARTESIAN_POINT('Ctrl Pts',(-3.6007202851384,1.,-1.6440700438558));
#54432=CARTESIAN_POINT('Ctrl Pts',(-3.59515368334887,-1.,-1.63894676675349));
#54433=CARTESIAN_POINT('Ctrl Pts',(-3.59515368334887,1.,-1.63894676675349));
#54434=CARTESIAN_POINT('Ctrl Pts',(-3.58955176627876,-1.,-1.63385971451259));
#54435=CARTESIAN_POINT('Ctrl Pts',(-3.58955176627876,1.,-1.63385971451259));
#54436=CARTESIAN_POINT('Ctrl Pts',(-3.5839162577435,-1.,-1.62881051550748));
#54437=CARTESIAN_POINT('Ctrl Pts',(-3.5839162577435,1.,-1.62881051550748));
#54438=CARTESIAN_POINT('Ctrl Pts',(-3.57825455954405,-1.,-1.62380329464851));
#54439=CARTESIAN_POINT('Ctrl Pts',(-3.57825455954405,1.,-1.62380329464851));
#54440=CARTESIAN_POINT('Ctrl Pts',(-3.57257679609826,-1.,-1.61884340915412));
#54441=CARTESIAN_POINT('Ctrl Pts',(-3.57257679609826,1.,-1.61884340915412));
#54442=CARTESIAN_POINT('Ctrl Pts',(-3.56689200468404,-1.,-1.61393581747522));
#54443=CARTESIAN_POINT('Ctrl Pts',(-3.56689200468404,1.,-1.61393581747522));
#54444=CARTESIAN_POINT('Ctrl Pts',(-3.56120432482986,-1.,-1.60908344685459));
#54445=CARTESIAN_POINT('Ctrl Pts',(-3.56120432482986,1.,-1.60908344685459));
#54446=CARTESIAN_POINT('Ctrl Pts',(-3.55550985096117,-1.,-1.60428584699848));
#54447=CARTESIAN_POINT('Ctrl Pts',(-3.55550985096117,1.,-1.60428584699848));
#54448=CARTESIAN_POINT('Ctrl Pts',(-3.54979148634426,-1.,-1.59953698113444));
#54449=CARTESIAN_POINT('Ctrl Pts',(-3.54979148634426,1.,-1.59953698113444));
#54450=CARTESIAN_POINT('Ctrl Pts',(-3.544024581823,-1.,-1.5948276694975));
#54451=CARTESIAN_POINT('Ctrl Pts',(-3.544024581823,1.,-1.5948276694975));
#54452=CARTESIAN_POINT('Ctrl Pts',(-3.53818616861045,-1.,-1.59014958368725));
#54453=CARTESIAN_POINT('Ctrl Pts',(-3.53818616861045,1.,-1.59014958368725));
#54454=CARTESIAN_POINT('Ctrl Pts',(-3.53226378147068,-1.,-1.58549906268083));
#54455=CARTESIAN_POINT('Ctrl Pts',(-3.53226378147068,1.,-1.58549906268083));
#54456=CARTESIAN_POINT('Ctrl Pts',(-3.52626275334899,-1.,-1.58088027227856));
#54457=CARTESIAN_POINT('Ctrl Pts',(-3.52626275334899,1.,-1.58088027227856));
#54458=CARTESIAN_POINT('Ctrl Pts',(-3.52021847865961,-1.,-1.5763104998818));
#54459=CARTESIAN_POINT('Ctrl Pts',(-3.52021847865961,1.,-1.5763104998818));
#54460=CARTESIAN_POINT('Ctrl Pts',(-3.51418598431733,-1.,-1.57181569799774));
#54461=CARTESIAN_POINT('Ctrl Pts',(-3.51418598431733,1.,-1.57181569799774));
#54462=CARTESIAN_POINT('Ctrl Pts',(-3.50821771695427,-1.,-1.56742097575041));
#54463=CARTESIAN_POINT('Ctrl Pts',(-3.50821771695427,1.,-1.56742097575041));
#54464=CARTESIAN_POINT('Ctrl Pts',(-3.50234321621607,-1.,-1.56314187758689));
#54465=CARTESIAN_POINT('Ctrl Pts',(-3.50234321621607,1.,-1.56314187758689));
#54466=CARTESIAN_POINT('Ctrl Pts',(-3.49655185179623,-1.,-1.55897703097859));
#54467=CARTESIAN_POINT('Ctrl Pts',(-3.49655185179623,1.,-1.55897703097859));
#54468=CARTESIAN_POINT('Ctrl Pts',(-3.49076460877317,-1.,-1.5548959590107));
#54469=CARTESIAN_POINT('Ctrl Pts',(-3.49076460877317,1.,-1.5548959590107));
#54470=CARTESIAN_POINT('Ctrl Pts',(-3.48485155928414,-1.,-1.55084702970382));
#54471=CARTESIAN_POINT('Ctrl Pts',(-3.48485155928414,1.,-1.55084702970382));
#54472=CARTESIAN_POINT('Ctrl Pts',(-3.47868272898599,-1.,-1.54678009290206));
#54473=CARTESIAN_POINT('Ctrl Pts',(-3.47868272898599,1.,-1.54678009290206));
#54474=CARTESIAN_POINT('Ctrl Pts',(-3.47217189224576,-1.,-1.54266605398152));
#54475=CARTESIAN_POINT('Ctrl Pts',(-3.47217189224576,1.,-1.54266605398152));
#54476=CARTESIAN_POINT('Ctrl Pts',(-3.46531752207222,-1.,-1.53851507915533));
#54477=CARTESIAN_POINT('Ctrl Pts',(-3.46531752207222,1.,-1.53851507915533));
#54478=CARTESIAN_POINT('Ctrl Pts',(-3.45825932955273,-1.,-1.53440195378902));
#54479=CARTESIAN_POINT('Ctrl Pts',(-3.45825932955273,1.,-1.53440195378902));
#54480=CARTESIAN_POINT('Ctrl Pts',(-3.45127136828667,-1.,-1.530462444618));
#54481=CARTESIAN_POINT('Ctrl Pts',(-3.45127136828667,1.,-1.530462444618));
#54482=CARTESIAN_POINT('Ctrl Pts',(-3.44469547527,-1.,-1.52686242875717));
#54483=CARTESIAN_POINT('Ctrl Pts',(-3.44469547527,1.,-1.52686242875717));
#54484=CARTESIAN_POINT('Ctrl Pts',(-3.43888895974182,-1.,-1.52377348950429));
#54485=CARTESIAN_POINT('Ctrl Pts',(-3.43888895974182,1.,-1.52377348950429));
#54486=CARTESIAN_POINT('Ctrl Pts',(-3.43417156977749,-1.,-1.52134826724227));
#54487=CARTESIAN_POINT('Ctrl Pts',(-3.43417156977749,1.,-1.52134826724227));
#54488=CARTESIAN_POINT('Ctrl Pts',(-3.43076036253384,-1.,-1.51969006980792));
#54489=CARTESIAN_POINT('Ctrl Pts',(-3.43076036253384,1.,-1.51969006980792));
#54490=CARTESIAN_POINT('Ctrl Pts',(-3.42915787669388,-1.,-1.51901585838879));
#54491=CARTESIAN_POINT('Ctrl Pts',(-3.42915787669388,1.,-1.51901585838879));
#54492=CARTESIAN_POINT('Ctrl Pts',(-3.42860527148835,-1.,-1.51888450659497));
#54493=CARTESIAN_POINT('Ctrl Pts',(-3.42860527148835,1.,-1.51888450659497));
#54494=CARTESIAN_POINT('Ctrl Pts',(-3.42852521763648,-1.,-1.51896318668306));
#54495=CARTESIAN_POINT('Ctrl Pts',(-3.42852521763648,1.,-1.51896318668306));
#54496=CARTESIAN_POINT('Ctrl Pts',(-3.42855728381368,-1.,-1.519044091397));
#54497=CARTESIAN_POINT('Ctrl Pts',(-3.42855728381368,1.,-1.519044091397));
#54498=CARTESIAN_POINT('',(-3.77614523045147,1.,-1.83867539237861));
#54499=CARTESIAN_POINT('Ctrl Pts',(-3.77614523045147,1.,-1.83867539237861));
#54500=CARTESIAN_POINT('Ctrl Pts',(-3.77518714458232,1.,-1.83742834010821));
#54501=CARTESIAN_POINT('Ctrl Pts',(-3.77326886065484,1.,-1.83493697935064));
#54502=CARTESIAN_POINT('Ctrl Pts',(-3.77038509819777,1.,-1.83120816956515));
#54503=CARTESIAN_POINT('Ctrl Pts',(-3.76652740355856,1.,-1.82625289221933));
#54504=CARTESIAN_POINT('Ctrl Pts',(-3.76168412709652,1.,-1.82008629694924));
#54505=CARTESIAN_POINT('Ctrl Pts',(-3.75681965683995,1.,-1.81394729834032));
#54506=CARTESIAN_POINT('Ctrl Pts',(-3.75193395888069,1.,-1.80783603939662));
#54507=CARTESIAN_POINT('Ctrl Pts',(-3.74702700874954,1.,-1.80175271485519));
#54508=CARTESIAN_POINT('Ctrl Pts',(-3.74209880351667,1.,-1.79569757859041));
#54509=CARTESIAN_POINT('Ctrl Pts',(-3.73714934729962,1.,-1.78967092823139));
#54510=CARTESIAN_POINT('Ctrl Pts',(-3.73217863095022,1.,-1.78367308442682));
#54511=CARTESIAN_POINT('Ctrl Pts',(-3.72718661205504,1.,-1.77770437039606));
#54512=CARTESIAN_POINT('Ctrl Pts',(-3.72217319911429,1.,-1.77176509401846));
#54513=CARTESIAN_POINT('Ctrl Pts',(-3.71713822377675,1.,-1.76585552124549));
#54514=CARTESIAN_POINT('Ctrl Pts',(-3.71208146346454,1.,-1.75997588499021));
#54515=CARTESIAN_POINT('Ctrl Pts',(-3.70700269736876,1.,-1.75412641804148));
#54516=CARTESIAN_POINT('Ctrl Pts',(-3.70190175673422,1.,-1.74830738046092));
#54517=CARTESIAN_POINT('Ctrl Pts',(-3.6967785691046,1.,-1.74251908492589));
#54518=CARTESIAN_POINT('Ctrl Pts',(-3.69163322647906,1.,-1.73676193254493));
#54519=CARTESIAN_POINT('Ctrl Pts',(-3.68646597019188,1.,-1.73103640956647));
#54520=CARTESIAN_POINT('Ctrl Pts',(-3.68127704936472,1.,-1.72534302437003));
#54521=CARTESIAN_POINT('Ctrl Pts',(-3.67606660374665,1.,-1.71968225581787));
#54522=CARTESIAN_POINT('Ctrl Pts',(-3.67083454901629,1.,-1.71405450210392));
#54523=CARTESIAN_POINT('Ctrl Pts',(-3.6655804319893,1.,-1.70846001610983));
#54524=CARTESIAN_POINT('Ctrl Pts',(-3.6603033877491,1.,-1.70289888566904));
#54525=CARTESIAN_POINT('Ctrl Pts',(-3.65500246526798,1.,-1.69737117722558));
#54526=CARTESIAN_POINT('Ctrl Pts',(-3.64967689827393,1.,-1.691877054817));
#54527=CARTESIAN_POINT('Ctrl Pts',(-3.64432638915199,1.,-1.68641690471455));
#54528=CARTESIAN_POINT('Ctrl Pts',(-3.63895140887443,1.,-1.68099146651577));
#54529=CARTESIAN_POINT('Ctrl Pts',(-3.63355343201211,1.,-1.67560193613145));
#54530=CARTESIAN_POINT('Ctrl Pts',(-3.62813422105257,1.,-1.67024966008037));
#54531=CARTESIAN_POINT('Ctrl Pts',(-3.62269517989104,1.,-1.66493585923853));
#54532=CARTESIAN_POINT('Ctrl Pts',(-3.61723666482457,1.,-1.65966133399186));
#54533=CARTESIAN_POINT('Ctrl Pts',(-3.61175734965129,1.,-1.65442619244327));
#54534=CARTESIAN_POINT('Ctrl Pts',(-3.60625346556992,1.,-1.64922952425833));
#54535=CARTESIAN_POINT('Ctrl Pts',(-3.6007202851384,1.,-1.6440700438558));
#54536=CARTESIAN_POINT('Ctrl Pts',(-3.59515368334887,1.,-1.63894676675349));
#54537=CARTESIAN_POINT('Ctrl Pts',(-3.58955176627876,1.,-1.63385971451259));
#54538=CARTESIAN_POINT('Ctrl Pts',(-3.5839162577435,1.,-1.62881051550748));
#54539=CARTESIAN_POINT('Ctrl Pts',(-3.57825455954405,1.,-1.62380329464851));
#54540=CARTESIAN_POINT('Ctrl Pts',(-3.57257679609826,1.,-1.61884340915412));
#54541=CARTESIAN_POINT('Ctrl Pts',(-3.56689200468404,1.,-1.61393581747522));
#54542=CARTESIAN_POINT('Ctrl Pts',(-3.56120432482986,1.,-1.60908344685459));
#54543=CARTESIAN_POINT('Ctrl Pts',(-3.55550985096117,1.,-1.60428584699848));
#54544=CARTESIAN_POINT('Ctrl Pts',(-3.54979148634426,1.,-1.59953698113444));
#54545=CARTESIAN_POINT('Ctrl Pts',(-3.544024581823,1.,-1.5948276694975));
#54546=CARTESIAN_POINT('Ctrl Pts',(-3.53818616861045,1.,-1.59014958368725));
#54547=CARTESIAN_POINT('Ctrl Pts',(-3.53226378147068,1.,-1.58549906268083));
#54548=CARTESIAN_POINT('Ctrl Pts',(-3.52626275334899,1.,-1.58088027227856));
#54549=CARTESIAN_POINT('Ctrl Pts',(-3.52021847865961,1.,-1.5763104998818));
#54550=CARTESIAN_POINT('Ctrl Pts',(-3.51418598431733,1.,-1.57181569799774));
#54551=CARTESIAN_POINT('Ctrl Pts',(-3.50821771695427,1.,-1.56742097575041));
#54552=CARTESIAN_POINT('Ctrl Pts',(-3.50234321621607,1.,-1.56314187758689));
#54553=CARTESIAN_POINT('Ctrl Pts',(-3.49655185179623,1.,-1.55897703097859));
#54554=CARTESIAN_POINT('Ctrl Pts',(-3.49076460877317,1.,-1.5548959590107));
#54555=CARTESIAN_POINT('Ctrl Pts',(-3.48485155928414,1.,-1.55084702970382));
#54556=CARTESIAN_POINT('Ctrl Pts',(-3.47868272898599,1.,-1.54678009290206));
#54557=CARTESIAN_POINT('Ctrl Pts',(-3.47217189224576,1.,-1.54266605398152));
#54558=CARTESIAN_POINT('Ctrl Pts',(-3.46531752207222,1.,-1.53851507915533));
#54559=CARTESIAN_POINT('Ctrl Pts',(-3.45825932955273,1.,-1.53440195378902));
#54560=CARTESIAN_POINT('Ctrl Pts',(-3.45127136828667,1.,-1.530462444618));
#54561=CARTESIAN_POINT('Ctrl Pts',(-3.44469547527,1.,-1.52686242875717));
#54562=CARTESIAN_POINT('Ctrl Pts',(-3.43888895974182,1.,-1.52377348950429));
#54563=CARTESIAN_POINT('Ctrl Pts',(-3.43417156977749,1.,-1.52134826724227));
#54564=CARTESIAN_POINT('Ctrl Pts',(-3.43101631893491,1.,-1.5198144909343));
#54565=CARTESIAN_POINT('Ctrl Pts',(-3.42946838852728,1.,-1.51914806898539));
#54566=CARTESIAN_POINT('Ctrl Pts',(-3.42884302333978,1.,-1.51895133295017));
#54567=CARTESIAN_POINT('Ctrl Pts',(-3.42864616361967,1.,-1.51893924967231));
#54568=CARTESIAN_POINT('Ctrl Pts',(-3.42859860294378,1.,-1.51895082866166));
#54569=CARTESIAN_POINT('',(-3.77614523045147,0.,-1.83867539237861));
#54570=CARTESIAN_POINT('Ctrl Pts',(-3.24418789321065,-1.,-1.8808893942881));
#54571=CARTESIAN_POINT('Ctrl Pts',(-3.24418789321065,1.,-1.8808893942881));
#54572=CARTESIAN_POINT('Ctrl Pts',(-3.24410359189733,-1.,-1.8809110068042));
#54573=CARTESIAN_POINT('Ctrl Pts',(-3.24410359189733,1.,-1.8809110068042));
#54574=CARTESIAN_POINT('Ctrl Pts',(-3.24408699284449,-1.,-1.8810220187274));
#54575=CARTESIAN_POINT('Ctrl Pts',(-3.24408699284449,1.,-1.8810220187274));
#54576=CARTESIAN_POINT('Ctrl Pts',(-3.24451807186964,-1.,-1.88139187908347));
#54577=CARTESIAN_POINT('Ctrl Pts',(-3.24451807186964,1.,-1.88139187908347));
#54578=CARTESIAN_POINT('Ctrl Pts',(-3.24600543790876,-1.,-1.88229202583187));
#54579=CARTESIAN_POINT('Ctrl Pts',(-3.24600543790876,1.,-1.88229202583187));
#54580=CARTESIAN_POINT('Ctrl Pts',(-3.24935200512055,-1.,-1.88407708646435));
#54581=CARTESIAN_POINT('Ctrl Pts',(-3.24935200512055,1.,-1.88407708646435));
#54582=CARTESIAN_POINT('Ctrl Pts',(-3.25408686339298,-1.,-1.88646802523372));
#54583=CARTESIAN_POINT('Ctrl Pts',(-3.25408686339298,1.,-1.88646802523372));
#54584=CARTESIAN_POINT('Ctrl Pts',(-3.2599988519361,-1.,-1.88934996203508));
#54585=CARTESIAN_POINT('Ctrl Pts',(-3.2599988519361,1.,-1.88934996203508));
#54586=CARTESIAN_POINT('Ctrl Pts',(-3.2667765388833,-1.,-1.89255393500769));
#54587=CARTESIAN_POINT('Ctrl Pts',(-3.2667765388833,1.,-1.89255393500769));
#54588=CARTESIAN_POINT('Ctrl Pts',(-3.27407108932908,-1.,-1.89589172903662));
#54589=CARTESIAN_POINT('Ctrl Pts',(-3.27407108932908,1.,-1.89589172903662));
#54590=CARTESIAN_POINT('Ctrl Pts',(-3.28154737912287,-1.,-1.89918429230424));
#54591=CARTESIAN_POINT('Ctrl Pts',(-3.28154737912287,1.,-1.89918429230424));
#54592=CARTESIAN_POINT('Ctrl Pts',(-3.28893448600364,-1.,-1.9022897124757));
#54593=CARTESIAN_POINT('Ctrl Pts',(-3.28893448600364,1.,-1.9022897124757));
#54594=CARTESIAN_POINT('Ctrl Pts',(-3.29608978722258,-1.,-1.9051389186417));
#54595=CARTESIAN_POINT('Ctrl Pts',(-3.29608978722258,1.,-1.9051389186417));
#54596=CARTESIAN_POINT('Ctrl Pts',(-3.30300595568341,-1.,-1.90773912171424));
#54597=CARTESIAN_POINT('Ctrl Pts',(-3.30300595568341,1.,-1.90773912171424));
#54598=CARTESIAN_POINT('Ctrl Pts',(-3.30975721158694,-1.,-1.91014297830502));
#54599=CARTESIAN_POINT('Ctrl Pts',(-3.30975721158694,1.,-1.91014297830502));
#54600=CARTESIAN_POINT('Ctrl Pts',(-3.31646052426395,-1.,-1.91242616234459));
#54601=CARTESIAN_POINT('Ctrl Pts',(-3.31646052426395,1.,-1.91242616234459));
#54602=CARTESIAN_POINT('Ctrl Pts',(-3.32323403454507,-1.,-1.91466343916612));
#54603=CARTESIAN_POINT('Ctrl Pts',(-3.32323403454507,1.,-1.91466343916612));
#54604=CARTESIAN_POINT('Ctrl Pts',(-3.33014884257812,-1.,-1.91690081930297));
#54605=CARTESIAN_POINT('Ctrl Pts',(-3.33014884257812,1.,-1.91690081930297));
#54606=CARTESIAN_POINT('Ctrl Pts',(-3.33721230709948,-1.,-1.91914609610173));
#54607=CARTESIAN_POINT('Ctrl Pts',(-3.33721230709948,1.,-1.91914609610173));
#54608=CARTESIAN_POINT('Ctrl Pts',(-3.34439448941915,-1.,-1.92138450828378));
#54609=CARTESIAN_POINT('Ctrl Pts',(-3.34439448941915,1.,-1.92138450828378));
#54610=CARTESIAN_POINT('Ctrl Pts',(-3.35164424847206,-1.,-1.92358838440518));
#54611=CARTESIAN_POINT('Ctrl Pts',(-3.35164424847206,1.,-1.92358838440518));
#54612=CARTESIAN_POINT('Ctrl Pts',(-3.35890824422976,-1.,-1.92572846125763));
#54613=CARTESIAN_POINT('Ctrl Pts',(-3.35890824422976,1.,-1.92572846125763));
#54614=CARTESIAN_POINT('Ctrl Pts',(-3.36615168657597,-1.,-1.92778626543803));
#54615=CARTESIAN_POINT('Ctrl Pts',(-3.36615168657597,1.,-1.92778626543803));
#54616=CARTESIAN_POINT('Ctrl Pts',(-3.37336807068078,-1.,-1.92975993109897));
#54617=CARTESIAN_POINT('Ctrl Pts',(-3.37336807068078,1.,-1.92975993109897));
#54618=CARTESIAN_POINT('Ctrl Pts',(-3.38056768525577,-1.,-1.93165739093292));
#54619=CARTESIAN_POINT('Ctrl Pts',(-3.38056768525577,1.,-1.93165739093292));
#54620=CARTESIAN_POINT('Ctrl Pts',(-3.38777076883267,-1.,-1.93349233176794));
#54621=CARTESIAN_POINT('Ctrl Pts',(-3.38777076883267,1.,-1.93349233176794));
#54622=CARTESIAN_POINT('Ctrl Pts',(-3.39499923640789,-1.,-1.93527929945982));
#54623=CARTESIAN_POINT('Ctrl Pts',(-3.39499923640789,1.,-1.93527929945982));
#54624=CARTESIAN_POINT('Ctrl Pts',(-3.40226802104093,-1.,-1.93702857723089));
#54625=CARTESIAN_POINT('Ctrl Pts',(-3.40226802104093,1.,-1.93702857723089));
#54626=CARTESIAN_POINT('Ctrl Pts',(-3.40957978266622,-1.,-1.93874306008132));
#54627=CARTESIAN_POINT('Ctrl Pts',(-3.40957978266622,1.,-1.93874306008132));
#54628=CARTESIAN_POINT('Ctrl Pts',(-3.41692971994082,-1.,-1.94042111965237));
#54629=CARTESIAN_POINT('Ctrl Pts',(-3.41692971994082,1.,-1.94042111965237));
#54630=CARTESIAN_POINT('Ctrl Pts',(-3.42430850941497,-1.,-1.94205835913692));
#54631=CARTESIAN_POINT('Ctrl Pts',(-3.42430850941497,1.,-1.94205835913692));
#54632=CARTESIAN_POINT('Ctrl Pts',(-3.43170586602436,-1.,-1.94364973660285));
#54633=CARTESIAN_POINT('Ctrl Pts',(-3.43170586602436,1.,-1.94364973660285));
#54634=CARTESIAN_POINT('Ctrl Pts',(-3.43911410197693,-1.,-1.94519168842883));
#54635=CARTESIAN_POINT('Ctrl Pts',(-3.43911410197693,1.,-1.94519168842883));
#54636=CARTESIAN_POINT('Ctrl Pts',(-3.44653088665685,-1.,-1.94668377715332));
#54637=CARTESIAN_POINT('Ctrl Pts',(-3.44653088665685,1.,-1.94668377715332));
#54638=CARTESIAN_POINT('Ctrl Pts',(-3.45395731584051,-1.,-1.94812754766524));
#54639=CARTESIAN_POINT('Ctrl Pts',(-3.45395731584051,1.,-1.94812754766524));
#54640=CARTESIAN_POINT('Ctrl Pts',(-3.46139661060959,-1.,-1.94952575850196));
#54641=CARTESIAN_POINT('Ctrl Pts',(-3.46139661060959,1.,-1.94952575850196));
#54642=CARTESIAN_POINT('Ctrl Pts',(-3.4688525897419,-1.,-1.95088147859876));
#54643=CARTESIAN_POINT('Ctrl Pts',(-3.4688525897419,1.,-1.95088147859876));
#54644=CARTESIAN_POINT('Ctrl Pts',(-3.47632820495926,-1.,-1.95219722189878));
#54645=CARTESIAN_POINT('Ctrl Pts',(-3.47632820495926,1.,-1.95219722189878));
#54646=CARTESIAN_POINT('Ctrl Pts',(-3.48382414832648,-1.,-1.95347412486316));
#54647=CARTESIAN_POINT('Ctrl Pts',(-3.48382414832648,1.,-1.95347412486316));
#54648=CARTESIAN_POINT('Ctrl Pts',(-3.49133956289154,-1.,-1.95471236969653));
#54649=CARTESIAN_POINT('Ctrl Pts',(-3.49133956289154,1.,-1.95471236969653));
#54650=CARTESIAN_POINT('Ctrl Pts',(-3.49887263575602,-1.,-1.9559115382367));
#54651=CARTESIAN_POINT('Ctrl Pts',(-3.49887263575602,1.,-1.9559115382367));
#54652=CARTESIAN_POINT('Ctrl Pts',(-3.50642124159913,-1.,-1.95707099606513));
#54653=CARTESIAN_POINT('Ctrl Pts',(-3.50642124159913,1.,-1.95707099606513));
#54654=CARTESIAN_POINT('Ctrl Pts',(-3.51398354617772,-1.,-1.95819025316768));
#54655=CARTESIAN_POINT('Ctrl Pts',(-3.51398354617772,1.,-1.95819025316768));
#54656=CARTESIAN_POINT('Ctrl Pts',(-3.52155867431438,-1.,-1.95926936324436));
#54657=CARTESIAN_POINT('Ctrl Pts',(-3.52155867431438,1.,-1.95926936324436));
#54658=CARTESIAN_POINT('Ctrl Pts',(-3.52914648844289,-1.,-1.96030879411534));
#54659=CARTESIAN_POINT('Ctrl Pts',(-3.52914648844289,1.,-1.96030879411534));
#54660=CARTESIAN_POINT('Ctrl Pts',(-3.53674730625759,-1.,-1.96130926212661));
#54661=CARTESIAN_POINT('Ctrl Pts',(-3.53674730625759,1.,-1.96130926212661));
#54662=CARTESIAN_POINT('Ctrl Pts',(-3.54436163300425,-1.,-1.96227157573058));
#54663=CARTESIAN_POINT('Ctrl Pts',(-3.54436163300425,1.,-1.96227157573058));
#54664=CARTESIAN_POINT('Ctrl Pts',(-3.55198990600929,-1.,-1.96319648628667));
#54665=CARTESIAN_POINT('Ctrl Pts',(-3.55198990600929,1.,-1.96319648628667));
#54666=CARTESIAN_POINT('Ctrl Pts',(-3.55963218706201,-1.,-1.96408450906868));
#54667=CARTESIAN_POINT('Ctrl Pts',(-3.55963218706201,1.,-1.96408450906868));
#54668=CARTESIAN_POINT('Ctrl Pts',(-3.56728820357933,-1.,-1.96493594634643));
#54669=CARTESIAN_POINT('Ctrl Pts',(-3.56728820357933,1.,-1.96493594634643));
#54670=CARTESIAN_POINT('Ctrl Pts',(-3.57495748601088,-1.,-1.96575096652857));
#54671=CARTESIAN_POINT('Ctrl Pts',(-3.57495748601088,1.,-1.96575096652857));
#54672=CARTESIAN_POINT('Ctrl Pts',(-3.58263947663884,-1.,-1.9665296668894));
#54673=CARTESIAN_POINT('Ctrl Pts',(-3.58263947663884,1.,-1.9665296668894));
#54674=CARTESIAN_POINT('Ctrl Pts',(-3.5903336402273,-1.,-1.96727213799507));
#54675=CARTESIAN_POINT('Ctrl Pts',(-3.5903336402273,1.,-1.96727213799507));
#54676=CARTESIAN_POINT('Ctrl Pts',(-3.59803959819725,-1.,-1.96797854118257));
#54677=CARTESIAN_POINT('Ctrl Pts',(-3.59803959819725,1.,-1.96797854118257));
#54678=CARTESIAN_POINT('Ctrl Pts',(-3.60575714017676,-1.,-1.96864911885775));
#54679=CARTESIAN_POINT('Ctrl Pts',(-3.60575714017676,1.,-1.96864911885775));
#54680=CARTESIAN_POINT('Ctrl Pts',(-3.61348615496393,-1.,-1.96928416040712));
#54681=CARTESIAN_POINT('Ctrl Pts',(-3.61348615496393,1.,-1.96928416040712));
#54682=CARTESIAN_POINT('Ctrl Pts',(-3.62122658401722,-1.,-1.96988398129888));
#54683=CARTESIAN_POINT('Ctrl Pts',(-3.62122658401722,1.,-1.96988398129888));
#54684=CARTESIAN_POINT('Ctrl Pts',(-3.62897836973397,-1.,-1.97044889850518));
#54685=CARTESIAN_POINT('Ctrl Pts',(-3.62897836973397,1.,-1.97044889850518));
#54686=CARTESIAN_POINT('Ctrl Pts',(-3.63674139590853,-1.,-1.97097920454698));
#54687=CARTESIAN_POINT('Ctrl Pts',(-3.63674139590853,1.,-1.97097920454698));
#54688=CARTESIAN_POINT('Ctrl Pts',(-3.64451546724221,-1.,-1.97147515441539));
#54689=CARTESIAN_POINT('Ctrl Pts',(-3.64451546724221,1.,-1.97147515441539));
#54690=CARTESIAN_POINT('Ctrl Pts',(-3.65230034717364,-1.,-1.97193697240645));
#54691=CARTESIAN_POINT('Ctrl Pts',(-3.65230034717364,1.,-1.97193697240645));
#54692=CARTESIAN_POINT('Ctrl Pts',(-3.66009578166865,-1.,-1.97236485439317));
#54693=CARTESIAN_POINT('Ctrl Pts',(-3.66009578166865,1.,-1.97236485439317));
#54694=CARTESIAN_POINT('Ctrl Pts',(-3.66790152751984,-1.,-1.9727589719863));
#54695=CARTESIAN_POINT('Ctrl Pts',(-3.66790152751984,1.,-1.9727589719863));
#54696=CARTESIAN_POINT('Ctrl Pts',(-3.67571738106175,-1.,-1.97311947678035));
#54697=CARTESIAN_POINT('Ctrl Pts',(-3.67571738106175,1.,-1.97311947678035));
#54698=CARTESIAN_POINT('Ctrl Pts',(-3.68354319913416,-1.,-1.9734465030363));
#54699=CARTESIAN_POINT('Ctrl Pts',(-3.68354319913416,1.,-1.9734465030363));
#54700=CARTESIAN_POINT('Ctrl Pts',(-3.69137888597855,-1.,-1.97374016224397));
#54701=CARTESIAN_POINT('Ctrl Pts',(-3.69137888597855,1.,-1.97374016224397));
#54702=CARTESIAN_POINT('Ctrl Pts',(-3.69765528558292,-1.,-1.97394846382288));
#54703=CARTESIAN_POINT('Ctrl Pts',(-3.69765528558292,1.,-1.97394846382288));
#54704=CARTESIAN_POINT('Ctrl Pts',(-3.70236698911837,-1.,-1.97408973726149));
#54705=CARTESIAN_POINT('Ctrl Pts',(-3.70236698911837,1.,-1.97408973726149));
#54706=CARTESIAN_POINT('Ctrl Pts',(-3.7055100813194,-1.,-1.974177276451));
#54707=CARTESIAN_POINT('Ctrl Pts',(-3.7055100813194,1.,-1.974177276451));
#54708=CARTESIAN_POINT('Ctrl Pts',(-3.70708211654725,-1.,-1.97421938526992));
#54709=CARTESIAN_POINT('Ctrl Pts',(-3.70708211654725,1.,-1.97421938526992));
#54710=CARTESIAN_POINT('',(-3.24413672884902,1.,-1.88097764062542));
#54711=CARTESIAN_POINT('Ctrl Pts',(-3.24413672884902,-1.,-1.88097764062542));
#54712=CARTESIAN_POINT('Ctrl Pts',(-3.24413672884902,-0.666666666666667,
-1.88097764062542));
#54713=CARTESIAN_POINT('Ctrl Pts',(-3.24413672884902,-0.333333333333333,
-1.88097764062542));
#54714=CARTESIAN_POINT('Ctrl Pts',(-3.24413672884902,0.333333333333333,
-1.88097764062542));
#54715=CARTESIAN_POINT('Ctrl Pts',(-3.24413672884902,0.666666666666667,
-1.88097764062542));
#54716=CARTESIAN_POINT('Ctrl Pts',(-3.24413672884902,1.,-1.88097764062542));
#54717=CARTESIAN_POINT('',(-3.70708211654725,1.,-1.97421938526992));
#54718=CARTESIAN_POINT('',(-3.70708211654725,0.,-1.97421938526992));
#54719=CARTESIAN_POINT('Ctrl Pts',(-3.24413672884902,1.,-1.88097764062542));
#54720=CARTESIAN_POINT('Ctrl Pts',(-3.24415531671311,1.,-1.88102292397987));
#54721=CARTESIAN_POINT('Ctrl Pts',(-3.24428080352952,1.,-1.88117508446657));
#54722=CARTESIAN_POINT('Ctrl Pts',(-3.24480754675942,1.,-1.88156537699118));
#54723=CARTESIAN_POINT('Ctrl Pts',(-3.24625654410705,1.,-1.88242596600422));
#54724=CARTESIAN_POINT('Ctrl Pts',(-3.24935200512055,1.,-1.88407708646435));
#54725=CARTESIAN_POINT('Ctrl Pts',(-3.25408686339298,1.,-1.88646802523372));
#54726=CARTESIAN_POINT('Ctrl Pts',(-3.2599988519361,1.,-1.88934996203508));
#54727=CARTESIAN_POINT('Ctrl Pts',(-3.2667765388833,1.,-1.89255393500769));
#54728=CARTESIAN_POINT('Ctrl Pts',(-3.27407108932908,1.,-1.89589172903662));
#54729=CARTESIAN_POINT('Ctrl Pts',(-3.28154737912287,1.,-1.89918429230424));
#54730=CARTESIAN_POINT('Ctrl Pts',(-3.28893448600364,1.,-1.9022897124757));
#54731=CARTESIAN_POINT('Ctrl Pts',(-3.29608978722258,1.,-1.9051389186417));
#54732=CARTESIAN_POINT('Ctrl Pts',(-3.30300595568341,1.,-1.90773912171424));
#54733=CARTESIAN_POINT('Ctrl Pts',(-3.30975721158694,1.,-1.91014297830502));
#54734=CARTESIAN_POINT('Ctrl Pts',(-3.31646052426395,1.,-1.91242616234459));
#54735=CARTESIAN_POINT('Ctrl Pts',(-3.32323403454507,1.,-1.91466343916612));
#54736=CARTESIAN_POINT('Ctrl Pts',(-3.33014884257812,1.,-1.91690081930297));
#54737=CARTESIAN_POINT('Ctrl Pts',(-3.33721230709948,1.,-1.91914609610173));
#54738=CARTESIAN_POINT('Ctrl Pts',(-3.34439448941915,1.,-1.92138450828378));
#54739=CARTESIAN_POINT('Ctrl Pts',(-3.35164424847206,1.,-1.92358838440518));
#54740=CARTESIAN_POINT('Ctrl Pts',(-3.35890824422976,1.,-1.92572846125763));
#54741=CARTESIAN_POINT('Ctrl Pts',(-3.36615168657597,1.,-1.92778626543803));
#54742=CARTESIAN_POINT('Ctrl Pts',(-3.37336807068078,1.,-1.92975993109897));
#54743=CARTESIAN_POINT('Ctrl Pts',(-3.38056768525577,1.,-1.93165739093292));
#54744=CARTESIAN_POINT('Ctrl Pts',(-3.38777076883267,1.,-1.93349233176794));
#54745=CARTESIAN_POINT('Ctrl Pts',(-3.39499923640789,1.,-1.93527929945982));
#54746=CARTESIAN_POINT('Ctrl Pts',(-3.40226802104093,1.,-1.93702857723089));
#54747=CARTESIAN_POINT('Ctrl Pts',(-3.40957978266622,1.,-1.93874306008132));
#54748=CARTESIAN_POINT('Ctrl Pts',(-3.41692971994082,1.,-1.94042111965237));
#54749=CARTESIAN_POINT('Ctrl Pts',(-3.42430850941497,1.,-1.94205835913692));
#54750=CARTESIAN_POINT('Ctrl Pts',(-3.43170586602436,1.,-1.94364973660285));
#54751=CARTESIAN_POINT('Ctrl Pts',(-3.43911410197693,1.,-1.94519168842883));
#54752=CARTESIAN_POINT('Ctrl Pts',(-3.44653088665685,1.,-1.94668377715332));
#54753=CARTESIAN_POINT('Ctrl Pts',(-3.45395731584051,1.,-1.94812754766524));
#54754=CARTESIAN_POINT('Ctrl Pts',(-3.46139661060959,1.,-1.94952575850196));
#54755=CARTESIAN_POINT('Ctrl Pts',(-3.4688525897419,1.,-1.95088147859876));
#54756=CARTESIAN_POINT('Ctrl Pts',(-3.47632820495926,1.,-1.95219722189878));
#54757=CARTESIAN_POINT('Ctrl Pts',(-3.48382414832648,1.,-1.95347412486316));
#54758=CARTESIAN_POINT('Ctrl Pts',(-3.49133956289154,1.,-1.95471236969653));
#54759=CARTESIAN_POINT('Ctrl Pts',(-3.49887263575602,1.,-1.9559115382367));
#54760=CARTESIAN_POINT('Ctrl Pts',(-3.50642124159913,1.,-1.95707099606513));
#54761=CARTESIAN_POINT('Ctrl Pts',(-3.51398354617772,1.,-1.95819025316768));
#54762=CARTESIAN_POINT('Ctrl Pts',(-3.52155867431438,1.,-1.95926936324436));
#54763=CARTESIAN_POINT('Ctrl Pts',(-3.52914648844289,1.,-1.96030879411534));
#54764=CARTESIAN_POINT('Ctrl Pts',(-3.53674730625759,1.,-1.96130926212661));
#54765=CARTESIAN_POINT('Ctrl Pts',(-3.54436163300425,1.,-1.96227157573058));
#54766=CARTESIAN_POINT('Ctrl Pts',(-3.55198990600929,1.,-1.96319648628667));
#54767=CARTESIAN_POINT('Ctrl Pts',(-3.55963218706201,1.,-1.96408450906868));
#54768=CARTESIAN_POINT('Ctrl Pts',(-3.56728820357933,1.,-1.96493594634643));
#54769=CARTESIAN_POINT('Ctrl Pts',(-3.57495748601088,1.,-1.96575096652857));
#54770=CARTESIAN_POINT('Ctrl Pts',(-3.58263947663884,1.,-1.9665296668894));
#54771=CARTESIAN_POINT('Ctrl Pts',(-3.5903336402273,1.,-1.96727213799507));
#54772=CARTESIAN_POINT('Ctrl Pts',(-3.59803959819725,1.,-1.96797854118257));
#54773=CARTESIAN_POINT('Ctrl Pts',(-3.60575714017676,1.,-1.96864911885775));
#54774=CARTESIAN_POINT('Ctrl Pts',(-3.61348615496393,1.,-1.96928416040712));
#54775=CARTESIAN_POINT('Ctrl Pts',(-3.62122658401722,1.,-1.96988398129888));
#54776=CARTESIAN_POINT('Ctrl Pts',(-3.62897836973397,1.,-1.97044889850518));
#54777=CARTESIAN_POINT('Ctrl Pts',(-3.63674139590853,1.,-1.97097920454698));
#54778=CARTESIAN_POINT('Ctrl Pts',(-3.64451546724221,1.,-1.97147515441539));
#54779=CARTESIAN_POINT('Ctrl Pts',(-3.65230034717364,1.,-1.97193697240645));
#54780=CARTESIAN_POINT('Ctrl Pts',(-3.66009578166865,1.,-1.97236485439317));
#54781=CARTESIAN_POINT('Ctrl Pts',(-3.66790152751984,1.,-1.9727589719863));
#54782=CARTESIAN_POINT('Ctrl Pts',(-3.67571738106175,1.,-1.97311947678035));
#54783=CARTESIAN_POINT('Ctrl Pts',(-3.68354319913416,1.,-1.9734465030363));
#54784=CARTESIAN_POINT('Ctrl Pts',(-3.69137888597855,1.,-1.97374016224397));
#54785=CARTESIAN_POINT('Ctrl Pts',(-3.69765528558292,1.,-1.97394846382288));
#54786=CARTESIAN_POINT('Ctrl Pts',(-3.70236698911837,1.,-1.97408973726149));
#54787=CARTESIAN_POINT('Ctrl Pts',(-3.7055100813194,1.,-1.974177276451));
#54788=CARTESIAN_POINT('Ctrl Pts',(-3.70708211654725,1.,-1.97421938526992));
#54789=CARTESIAN_POINT('Origin',(-3.70708211654725,0.,-1.97421938526992));
#54790=CARTESIAN_POINT('',(-3.77614523045147,1.,-1.83867539237861));
#54791=CARTESIAN_POINT('Origin',(0.,0.,0.));
#54792=CARTESIAN_POINT('',(-3.14877060440425,1.,-2.03660101169564));
#54793=CARTESIAN_POINT('Origin',(0.,1.,0.));
#54794=CARTESIAN_POINT('Ctrl Pts',(-3.14877060440425,1.,-2.03660101169564));
#54795=CARTESIAN_POINT('Ctrl Pts',(-3.14877060440425,0.666666666666667,
-2.03660101169564));
#54796=CARTESIAN_POINT('Ctrl Pts',(-3.14877060440425,0.333333333333333,
-2.03660101169564));
#54797=CARTESIAN_POINT('Ctrl Pts',(-3.14877060440425,-0.333333333333333,
-2.03660101169564));
#54798=CARTESIAN_POINT('Ctrl Pts',(-3.14877060440425,-0.666666666666667,
-2.03660101169564));
#54799=CARTESIAN_POINT('Ctrl Pts',(-3.14877060440425,-1.,-2.03660101169564));
#54800=CARTESIAN_POINT('Ctrl Pts',(-3.44202241512147,-1.,-2.40675750623143));
#54801=CARTESIAN_POINT('Ctrl Pts',(-3.44202241512147,1.,-2.40675750623143));
#54802=CARTESIAN_POINT('Ctrl Pts',(-3.44127120683402,-1.,-2.40537592959345));
#54803=CARTESIAN_POINT('Ctrl Pts',(-3.44127120683402,1.,-2.40537592959345));
#54804=CARTESIAN_POINT('Ctrl Pts',(-3.43976627485223,-1.,-2.40261515590099));
#54805=CARTESIAN_POINT('Ctrl Pts',(-3.43976627485223,1.,-2.40261515590099));
#54806=CARTESIAN_POINT('Ctrl Pts',(-3.43750133066036,-1.,-2.39848113411429));
#54807=CARTESIAN_POINT('Ctrl Pts',(-3.43750133066036,1.,-2.39848113411429));
#54808=CARTESIAN_POINT('Ctrl Pts',(-3.43446630680436,-1.,-2.39298338805823));
#54809=CARTESIAN_POINT('Ctrl Pts',(-3.43446630680436,1.,-2.39298338805823));
#54810=CARTESIAN_POINT('Ctrl Pts',(-3.43064732714472,-1.,-2.38613505844641));
#54811=CARTESIAN_POINT('Ctrl Pts',(-3.43064732714472,1.,-2.38613505844641));
#54812=CARTESIAN_POINT('Ctrl Pts',(-3.42680309755241,-1.,-2.37931067029517));
#54813=CARTESIAN_POINT('Ctrl Pts',(-3.42680309755241,1.,-2.37931067029517));
#54814=CARTESIAN_POINT('Ctrl Pts',(-3.42293356216595,-1.,-2.37251035954351));
#54815=CARTESIAN_POINT('Ctrl Pts',(-3.42293356216595,1.,-2.37251035954351));
#54816=CARTESIAN_POINT('Ctrl Pts',(-3.41903866635384,-1.,-2.36573431470314));
#54817=CARTESIAN_POINT('Ctrl Pts',(-3.41903866635384,1.,-2.36573431470314));
#54818=CARTESIAN_POINT('Ctrl Pts',(-3.4151183675076,-1.,-2.35898278606449));
#54819=CARTESIAN_POINT('Ctrl Pts',(-3.4151183675076,1.,-2.35898278606449));
#54820=CARTESIAN_POINT('Ctrl Pts',(-3.41117262313464,-1.,-2.35225606823649));
#54821=CARTESIAN_POINT('Ctrl Pts',(-3.41117262313464,1.,-2.35225606823649));
#54822=CARTESIAN_POINT('Ctrl Pts',(-3.40720137403888,-1.,-2.34555447648901));
#54823=CARTESIAN_POINT('Ctrl Pts',(-3.40720137403888,1.,-2.34555447648901));
#54824=CARTESIAN_POINT('Ctrl Pts',(-3.40320452776646,-1.,-2.33887832342715));
#54825=CARTESIAN_POINT('Ctrl Pts',(-3.40320452776646,1.,-2.33887832342715));
#54826=CARTESIAN_POINT('Ctrl Pts',(-3.39918194578115,-1.,-2.33222789882601));
#54827=CARTESIAN_POINT('Ctrl Pts',(-3.39918194578115,1.,-2.33222789882601));
#54828=CARTESIAN_POINT('Ctrl Pts',(-3.39513342020045,-1.,-2.32560343902683));
#54829=CARTESIAN_POINT('Ctrl Pts',(-3.39513342020045,1.,-2.32560343902683));
#54830=CARTESIAN_POINT('Ctrl Pts',(-3.39105869475112,-1.,-2.31900513925627));
#54831=CARTESIAN_POINT('Ctrl Pts',(-3.39105869475112,1.,-2.31900513925627));
#54832=CARTESIAN_POINT('Ctrl Pts',(-3.38695751492659,-1.,-2.31243319489505));
#54833=CARTESIAN_POINT('Ctrl Pts',(-3.38695751492659,1.,-2.31243319489505));
#54834=CARTESIAN_POINT('Ctrl Pts',(-3.38282967336676,-1.,-2.30588783640389));
#54835=CARTESIAN_POINT('Ctrl Pts',(-3.38282967336676,1.,-2.30588783640389));
#54836=CARTESIAN_POINT('Ctrl Pts',(-3.37867504959382,-1.,-2.29936936127588));
#54837=CARTESIAN_POINT('Ctrl Pts',(-3.37867504959382,1.,-2.29936936127588));
#54838=CARTESIAN_POINT('Ctrl Pts',(-3.37449367172707,-1.,-2.2928781800731));
#54839=CARTESIAN_POINT('Ctrl Pts',(-3.37449367172707,1.,-2.2928781800731));
#54840=CARTESIAN_POINT('Ctrl Pts',(-3.37028570206357,-1.,-2.28641481081045));
#54841=CARTESIAN_POINT('Ctrl Pts',(-3.37028570206357,1.,-2.28641481081045));
#54842=CARTESIAN_POINT('Ctrl Pts',(-3.36605130712978,-1.,-2.27997979457968));
#54843=CARTESIAN_POINT('Ctrl Pts',(-3.36605130712978,1.,-2.27997979457968));
#54844=CARTESIAN_POINT('Ctrl Pts',(-3.36179055004369,-1.,-2.27357362620902));
#54845=CARTESIAN_POINT('Ctrl Pts',(-3.36179055004369,1.,-2.27357362620902));
#54846=CARTESIAN_POINT('Ctrl Pts',(-3.35750328523077,-1.,-2.26719668579921));
#54847=CARTESIAN_POINT('Ctrl Pts',(-3.35750328523077,1.,-2.26719668579921));
#54848=CARTESIAN_POINT('Ctrl Pts',(-3.35318902552676,-1.,-2.26084915222484));
#54849=CARTESIAN_POINT('Ctrl Pts',(-3.35318902552676,1.,-2.26084915222484));
#54850=CARTESIAN_POINT('Ctrl Pts',(-3.34884690292342,-1.,-2.25453097693524));
#54851=CARTESIAN_POINT('Ctrl Pts',(-3.34884690292342,1.,-2.25453097693524));
#54852=CARTESIAN_POINT('Ctrl Pts',(-3.34447596770768,-1.,-2.24824207678288));
#54853=CARTESIAN_POINT('Ctrl Pts',(-3.34447596770768,1.,-2.24824207678288));
#54854=CARTESIAN_POINT('Ctrl Pts',(-3.34007543738044,-1.,-2.24198249391437));
#54855=CARTESIAN_POINT('Ctrl Pts',(-3.34007543738044,1.,-2.24198249391437));
#54856=CARTESIAN_POINT('Ctrl Pts',(-3.33564495756478,-1.,-2.2357525632881));
#54857=CARTESIAN_POINT('Ctrl Pts',(-3.33564495756478,1.,-2.2357525632881));
#54858=CARTESIAN_POINT('Ctrl Pts',(-3.33118487773593,-1.,-2.22955308907221));
#54859=CARTESIAN_POINT('Ctrl Pts',(-3.33118487773593,1.,-2.22955308907221));
#54860=CARTESIAN_POINT('Ctrl Pts',(-3.32669646722871,-1.,-2.22338548312758));
#54861=CARTESIAN_POINT('Ctrl Pts',(-3.32669646722871,1.,-2.22338548312758));
#54862=CARTESIAN_POINT('Ctrl Pts',(-3.32218125618955,-1.,-2.21725135110889));
#54863=CARTESIAN_POINT('Ctrl Pts',(-3.32218125618955,1.,-2.21725135110889));
#54864=CARTESIAN_POINT('Ctrl Pts',(-3.31764044024231,-1.,-2.21115211847872));
#54865=CARTESIAN_POINT('Ctrl Pts',(-3.31764044024231,1.,-2.21115211847872));
#54866=CARTESIAN_POINT('Ctrl Pts',(-3.3130742460895,-1.,-2.20508863150608));
#54867=CARTESIAN_POINT('Ctrl Pts',(-3.3130742460895,1.,-2.20508863150608));
#54868=CARTESIAN_POINT('Ctrl Pts',(-3.30848134694596,-1.,-2.19906078949924));
#54869=CARTESIAN_POINT('Ctrl Pts',(-3.30848134694596,1.,-2.19906078949924));
#54870=CARTESIAN_POINT('Ctrl Pts',(-3.30385816281831,-1.,-2.19306710376112));
#54871=CARTESIAN_POINT('Ctrl Pts',(-3.30385816281831,1.,-2.19306710376112));
#54872=CARTESIAN_POINT('Ctrl Pts',(-3.29920022557635,-1.,-2.18710556500325));
#54873=CARTESIAN_POINT('Ctrl Pts',(-3.29920022557635,1.,-2.18710556500325));
#54874=CARTESIAN_POINT('Ctrl Pts',(-3.29450361500484,-1.,-2.18117455557062));
#54875=CARTESIAN_POINT('Ctrl Pts',(-3.29450361500484,1.,-2.18117455557062));
#54876=CARTESIAN_POINT('Ctrl Pts',(-3.28976645712566,-1.,-2.17527380048422));
#54877=CARTESIAN_POINT('Ctrl Pts',(-3.28976645712566,1.,-2.17527380048422));
#54878=CARTESIAN_POINT('Ctrl Pts',(-3.2849901997973,-1.,-2.16940517773459));
#54879=CARTESIAN_POINT('Ctrl Pts',(-3.2849901997973,1.,-2.16940517773459));
#54880=CARTESIAN_POINT('Ctrl Pts',(-3.28018150841414,-1.,-2.16357391934434));
#54881=CARTESIAN_POINT('Ctrl Pts',(-3.28018150841414,1.,-2.16357391934434));
#54882=CARTESIAN_POINT('Ctrl Pts',(-3.27534954469206,-1.,-2.15778690038359));
#54883=CARTESIAN_POINT('Ctrl Pts',(-3.27534954469206,1.,-2.15778690038359));
#54884=CARTESIAN_POINT('Ctrl Pts',(-3.27050245897244,-1.,-2.15205043199818));
#54885=CARTESIAN_POINT('Ctrl Pts',(-3.27050245897244,1.,-2.15205043199818));
#54886=CARTESIAN_POINT('Ctrl Pts',(-3.26564388189764,-1.,-2.14636805295663));
#54887=CARTESIAN_POINT('Ctrl Pts',(-3.26564388189764,1.,-2.14636805295663));
#54888=CARTESIAN_POINT('Ctrl Pts',(-3.26077002641868,-1.,-2.14073870754257));
#54889=CARTESIAN_POINT('Ctrl Pts',(-3.26077002641868,1.,-2.14073870754257));
#54890=CARTESIAN_POINT('Ctrl Pts',(-3.25586495065027,-1.,-2.13515375878786));
#54891=CARTESIAN_POINT('Ctrl Pts',(-3.25586495065027,1.,-2.13515375878786));
#54892=CARTESIAN_POINT('Ctrl Pts',(-3.25090574493994,-1.,-2.1296002839681));
#54893=CARTESIAN_POINT('Ctrl Pts',(-3.25090574493994,1.,-2.1296002839681));
#54894=CARTESIAN_POINT('Ctrl Pts',(-3.24587102613347,-1.,-2.12406646410943));
#54895=CARTESIAN_POINT('Ctrl Pts',(-3.24587102613347,1.,-2.12406646410943));
#54896=CARTESIAN_POINT('Ctrl Pts',(-3.24074905517282,-1.,-2.11854673326972));
#54897=CARTESIAN_POINT('Ctrl Pts',(-3.24074905517282,1.,-2.11854673326972));
#54898=CARTESIAN_POINT('Ctrl Pts',(-3.23554444767115,-1.,-2.11304604021784));
#54899=CARTESIAN_POINT('Ctrl Pts',(-3.23554444767115,1.,-2.11304604021784));
#54900=CARTESIAN_POINT('Ctrl Pts',(-3.23028945793334,-1.,-2.1075869964248));
#54901=CARTESIAN_POINT('Ctrl Pts',(-3.23028945793334,1.,-2.1075869964248));
#54902=CARTESIAN_POINT('Ctrl Pts',(-3.22503437553496,-1.,-2.10220384298533));
#54903=CARTESIAN_POINT('Ctrl Pts',(-3.22503437553496,1.,-2.10220384298533));
#54904=CARTESIAN_POINT('Ctrl Pts',(-3.21982707347067,-1.,-2.09692958434933));
#54905=CARTESIAN_POINT('Ctrl Pts',(-3.21982707347067,1.,-2.09692958434933));
#54906=CARTESIAN_POINT('Ctrl Pts',(-3.2146942960168,-1.,-2.0917841946046));
#54907=CARTESIAN_POINT('Ctrl Pts',(-3.2146942960168,1.,-2.0917841946046));
#54908=CARTESIAN_POINT('Ctrl Pts',(-3.20962575845433,-1.,-2.08676465517435));
#54909=CARTESIAN_POINT('Ctrl Pts',(-3.20962575845433,1.,-2.08676465517435));
#54910=CARTESIAN_POINT('Ctrl Pts',(-3.20454818630635,-1.,-2.08182850370816));
#54911=CARTESIAN_POINT('Ctrl Pts',(-3.20454818630635,1.,-2.08182850370816));
#54912=CARTESIAN_POINT('Ctrl Pts',(-3.19934132835879,-1.,-2.0769044187063));
#54913=CARTESIAN_POINT('Ctrl Pts',(-3.19934132835879,1.,-2.0769044187063));
#54914=CARTESIAN_POINT('Ctrl Pts',(-3.19388465568113,-1.,-2.07192253497765));
#54915=CARTESIAN_POINT('Ctrl Pts',(-3.19388465568113,1.,-2.07192253497765));
#54916=CARTESIAN_POINT('Ctrl Pts',(-3.18809755562297,-1.,-2.06684062744065));
#54917=CARTESIAN_POINT('Ctrl Pts',(-3.18809755562297,1.,-2.06684062744065));
#54918=CARTESIAN_POINT('Ctrl Pts',(-3.18197692964677,-1.,-2.06166849827143));
#54919=CARTESIAN_POINT('Ctrl Pts',(-3.18197692964677,1.,-2.06166849827143));
#54920=CARTESIAN_POINT('Ctrl Pts',(-3.17564906975592,-1.,-2.05650186773279));
#54921=CARTESIAN_POINT('Ctrl Pts',(-3.17564906975592,1.,-2.05650186773279));
#54922=CARTESIAN_POINT('Ctrl Pts',(-3.16936341689859,-1.,-2.05151770247452));
#54923=CARTESIAN_POINT('Ctrl Pts',(-3.16936341689859,1.,-2.05151770247452));
#54924=CARTESIAN_POINT('Ctrl Pts',(-3.16343165059235,-1.,-2.0469333124766));
#54925=CARTESIAN_POINT('Ctrl Pts',(-3.16343165059235,1.,-2.0469333124766));
#54926=CARTESIAN_POINT('Ctrl Pts',(-3.15817983946525,-1.,-2.04297406404132));
#54927=CARTESIAN_POINT('Ctrl Pts',(-3.15817983946525,1.,-2.04297406404132));
#54928=CARTESIAN_POINT('Ctrl Pts',(-3.1538999167466,-1.,-2.03984073791432));
#54929=CARTESIAN_POINT('Ctrl Pts',(-3.1538999167466,1.,-2.03984073791432));
#54930=CARTESIAN_POINT('Ctrl Pts',(-3.15079010635326,-1.,-2.03766932526171));
#54931=CARTESIAN_POINT('Ctrl Pts',(-3.15079010635326,1.,-2.03766932526171));
#54932=CARTESIAN_POINT('Ctrl Pts',(-3.14931281967585,-1.,-2.03675273048882));
#54933=CARTESIAN_POINT('Ctrl Pts',(-3.14931281967585,1.,-2.03675273048882));
#54934=CARTESIAN_POINT('Ctrl Pts',(-3.14878756590499,-1.,-2.03653654935384));
#54935=CARTESIAN_POINT('Ctrl Pts',(-3.14878756590499,1.,-2.03653654935384));
#54936=CARTESIAN_POINT('Ctrl Pts',(-3.14869618937138,-1.,-2.036601737578));
#54937=CARTESIAN_POINT('Ctrl Pts',(-3.14869618937138,1.,-2.036601737578));
#54938=CARTESIAN_POINT('Ctrl Pts',(-3.1487152044751,-1.,-2.03668666247593));
#54939=CARTESIAN_POINT('Ctrl Pts',(-3.1487152044751,1.,-2.03668666247593));
#54940=CARTESIAN_POINT('',(-3.44202241512147,1.,-2.40675750623143));
#54941=CARTESIAN_POINT('Ctrl Pts',(-3.44202241512147,1.,-2.40675750623143));
#54942=CARTESIAN_POINT('Ctrl Pts',(-3.44127120683402,1.,-2.40537592959345));
#54943=CARTESIAN_POINT('Ctrl Pts',(-3.43976627485223,1.,-2.40261515590099));
#54944=CARTESIAN_POINT('Ctrl Pts',(-3.43750133066036,1.,-2.39848113411429));
#54945=CARTESIAN_POINT('Ctrl Pts',(-3.43446630680436,1.,-2.39298338805823));
#54946=CARTESIAN_POINT('Ctrl Pts',(-3.43064732714472,1.,-2.38613505844641));
#54947=CARTESIAN_POINT('Ctrl Pts',(-3.42680309755241,1.,-2.37931067029517));
#54948=CARTESIAN_POINT('Ctrl Pts',(-3.42293356216595,1.,-2.37251035954351));
#54949=CARTESIAN_POINT('Ctrl Pts',(-3.41903866635384,1.,-2.36573431470314));
#54950=CARTESIAN_POINT('Ctrl Pts',(-3.4151183675076,1.,-2.35898278606449));
#54951=CARTESIAN_POINT('Ctrl Pts',(-3.41117262313464,1.,-2.35225606823649));
#54952=CARTESIAN_POINT('Ctrl Pts',(-3.40720137403888,1.,-2.34555447648901));
#54953=CARTESIAN_POINT('Ctrl Pts',(-3.40320452776646,1.,-2.33887832342715));
#54954=CARTESIAN_POINT('Ctrl Pts',(-3.39918194578115,1.,-2.33222789882601));
#54955=CARTESIAN_POINT('Ctrl Pts',(-3.39513342020045,1.,-2.32560343902683));
#54956=CARTESIAN_POINT('Ctrl Pts',(-3.39105869475112,1.,-2.31900513925627));
#54957=CARTESIAN_POINT('Ctrl Pts',(-3.38695751492659,1.,-2.31243319489505));
#54958=CARTESIAN_POINT('Ctrl Pts',(-3.38282967336676,1.,-2.30588783640389));
#54959=CARTESIAN_POINT('Ctrl Pts',(-3.37867504959382,1.,-2.29936936127588));
#54960=CARTESIAN_POINT('Ctrl Pts',(-3.37449367172707,1.,-2.2928781800731));
#54961=CARTESIAN_POINT('Ctrl Pts',(-3.37028570206357,1.,-2.28641481081045));
#54962=CARTESIAN_POINT('Ctrl Pts',(-3.36605130712978,1.,-2.27997979457968));
#54963=CARTESIAN_POINT('Ctrl Pts',(-3.36179055004369,1.,-2.27357362620902));
#54964=CARTESIAN_POINT('Ctrl Pts',(-3.35750328523077,1.,-2.26719668579921));
#54965=CARTESIAN_POINT('Ctrl Pts',(-3.35318902552676,1.,-2.26084915222484));
#54966=CARTESIAN_POINT('Ctrl Pts',(-3.34884690292342,1.,-2.25453097693524));
#54967=CARTESIAN_POINT('Ctrl Pts',(-3.34447596770768,1.,-2.24824207678288));
#54968=CARTESIAN_POINT('Ctrl Pts',(-3.34007543738044,1.,-2.24198249391437));
#54969=CARTESIAN_POINT('Ctrl Pts',(-3.33564495756478,1.,-2.2357525632881));
#54970=CARTESIAN_POINT('Ctrl Pts',(-3.33118487773593,1.,-2.22955308907221));
#54971=CARTESIAN_POINT('Ctrl Pts',(-3.32669646722871,1.,-2.22338548312758));
#54972=CARTESIAN_POINT('Ctrl Pts',(-3.32218125618955,1.,-2.21725135110889));
#54973=CARTESIAN_POINT('Ctrl Pts',(-3.31764044024231,1.,-2.21115211847872));
#54974=CARTESIAN_POINT('Ctrl Pts',(-3.3130742460895,1.,-2.20508863150608));
#54975=CARTESIAN_POINT('Ctrl Pts',(-3.30848134694596,1.,-2.19906078949924));
#54976=CARTESIAN_POINT('Ctrl Pts',(-3.30385816281831,1.,-2.19306710376112));
#54977=CARTESIAN_POINT('Ctrl Pts',(-3.29920022557635,1.,-2.18710556500325));
#54978=CARTESIAN_POINT('Ctrl Pts',(-3.29450361500484,1.,-2.18117455557062));
#54979=CARTESIAN_POINT('Ctrl Pts',(-3.28976645712566,1.,-2.17527380048422));
#54980=CARTESIAN_POINT('Ctrl Pts',(-3.2849901997973,1.,-2.16940517773459));
#54981=CARTESIAN_POINT('Ctrl Pts',(-3.28018150841414,1.,-2.16357391934434));
#54982=CARTESIAN_POINT('Ctrl Pts',(-3.27534954469206,1.,-2.15778690038359));
#54983=CARTESIAN_POINT('Ctrl Pts',(-3.27050245897244,1.,-2.15205043199818));
#54984=CARTESIAN_POINT('Ctrl Pts',(-3.26564388189764,1.,-2.14636805295663));
#54985=CARTESIAN_POINT('Ctrl Pts',(-3.26077002641868,1.,-2.14073870754257));
#54986=CARTESIAN_POINT('Ctrl Pts',(-3.25586495065027,1.,-2.13515375878786));
#54987=CARTESIAN_POINT('Ctrl Pts',(-3.25090574493994,1.,-2.1296002839681));
#54988=CARTESIAN_POINT('Ctrl Pts',(-3.24587102613347,1.,-2.12406646410943));
#54989=CARTESIAN_POINT('Ctrl Pts',(-3.24074905517282,1.,-2.11854673326972));
#54990=CARTESIAN_POINT('Ctrl Pts',(-3.23554444767115,1.,-2.11304604021784));
#54991=CARTESIAN_POINT('Ctrl Pts',(-3.23028945793334,1.,-2.1075869964248));
#54992=CARTESIAN_POINT('Ctrl Pts',(-3.22503437553496,1.,-2.10220384298533));
#54993=CARTESIAN_POINT('Ctrl Pts',(-3.21982707347067,1.,-2.09692958434933));
#54994=CARTESIAN_POINT('Ctrl Pts',(-3.2146942960168,1.,-2.0917841946046));
#54995=CARTESIAN_POINT('Ctrl Pts',(-3.20962575845433,1.,-2.08676465517435));
#54996=CARTESIAN_POINT('Ctrl Pts',(-3.20454818630635,1.,-2.08182850370816));
#54997=CARTESIAN_POINT('Ctrl Pts',(-3.19934132835879,1.,-2.0769044187063));
#54998=CARTESIAN_POINT('Ctrl Pts',(-3.19388465568113,1.,-2.07192253497765));
#54999=CARTESIAN_POINT('Ctrl Pts',(-3.18809755562297,1.,-2.06684062744065));
#55000=CARTESIAN_POINT('Ctrl Pts',(-3.18197692964677,1.,-2.06166849827143));
#55001=CARTESIAN_POINT('Ctrl Pts',(-3.17564906975592,1.,-2.05650186773279));
#55002=CARTESIAN_POINT('Ctrl Pts',(-3.16936341689859,1.,-2.05151770247452));
#55003=CARTESIAN_POINT('Ctrl Pts',(-3.16343165059235,1.,-2.0469333124766));
#55004=CARTESIAN_POINT('Ctrl Pts',(-3.15817983946525,1.,-2.04297406404132));
#55005=CARTESIAN_POINT('Ctrl Pts',(-3.1538999167466,1.,-2.03984073791432));
#55006=CARTESIAN_POINT('Ctrl Pts',(-3.15102344775396,1.,-2.03783225496023));
#55007=CARTESIAN_POINT('Ctrl Pts',(-3.14959882629936,1.,-2.03693188810614));
#55008=CARTESIAN_POINT('Ctrl Pts',(-3.14901193669147,1.,-2.03663974554941));
#55009=CARTESIAN_POINT('Ctrl Pts',(-3.1488193908823,1.,-2.03659701539175));
#55010=CARTESIAN_POINT('Ctrl Pts',(-3.14877060440425,1.,-2.03660101169564));
#55011=CARTESIAN_POINT('',(-3.44202241512147,0.,-2.40675750623143));
#55012=CARTESIAN_POINT('Ctrl Pts',(-2.91001063062876,-1.,-2.36523532225181));
#55013=CARTESIAN_POINT('Ctrl Pts',(-2.91001063062876,1.,-2.36523532225181));
#55014=CARTESIAN_POINT('Ctrl Pts',(-2.90992398626211,-1.,-2.36524348105112));
#55015=CARTESIAN_POINT('Ctrl Pts',(-2.90992398626211,1.,-2.36524348105112));
#55016=CARTESIAN_POINT('Ctrl Pts',(-2.90989022548032,-1.,-2.36535052956938));
#55017=CARTESIAN_POINT('Ctrl Pts',(-2.90989022548032,1.,-2.36535052956938));
#55018=CARTESIAN_POINT('Ctrl Pts',(-2.91025813830041,-1.,-2.36578327194741));
#55019=CARTESIAN_POINT('Ctrl Pts',(-2.91025813830041,1.,-2.36578327194741));
#55020=CARTESIAN_POINT('Ctrl Pts',(-2.9115863784204,-1.,-2.36690501170627));
#55021=CARTESIAN_POINT('Ctrl Pts',(-2.9115863784204,1.,-2.36690501170627));
#55022=CARTESIAN_POINT('Ctrl Pts',(-2.9146124988314,-1.,-2.36919161373173));
#55023=CARTESIAN_POINT('Ctrl Pts',(-2.9146124988314,1.,-2.36919161373173));
#55024=CARTESIAN_POINT('Ctrl Pts',(-2.91891503791411,-1.,-2.37229381109821));
#55025=CARTESIAN_POINT('Ctrl Pts',(-2.91891503791411,1.,-2.37229381109821));
#55026=CARTESIAN_POINT('Ctrl Pts',(-2.92430340582608,-1.,-2.3760651052403));
#55027=CARTESIAN_POINT('Ctrl Pts',(-2.92430340582608,1.,-2.3760651052403));
#55028=CARTESIAN_POINT('Ctrl Pts',(-2.93049643640206,-1.,-2.38028989582073));
#55029=CARTESIAN_POINT('Ctrl Pts',(-2.93049643640206,1.,-2.38028989582073));
#55030=CARTESIAN_POINT('Ctrl Pts',(-2.93717903280391,-1.,-2.38472771516311));
#55031=CARTESIAN_POINT('Ctrl Pts',(-2.93717903280391,1.,-2.38472771516311));
#55032=CARTESIAN_POINT('Ctrl Pts',(-2.94404820669076,-1.,-2.38914929090759));
#55033=CARTESIAN_POINT('Ctrl Pts',(-2.94404820669076,1.,-2.38914929090759));
#55034=CARTESIAN_POINT('Ctrl Pts',(-2.95085857128439,-1.,-2.39337207631667));
#55035=CARTESIAN_POINT('Ctrl Pts',(-2.95085857128439,1.,-2.39337207631667));
#55036=CARTESIAN_POINT('Ctrl Pts',(-2.95748006482942,-1.,-2.39730553974517));
#55037=CARTESIAN_POINT('Ctrl Pts',(-2.95748006482942,1.,-2.39730553974517));
#55038=CARTESIAN_POINT('Ctrl Pts',(-2.96390432240312,-1.,-2.4009556571164));
#55039=CARTESIAN_POINT('Ctrl Pts',(-2.96390432240312,1.,-2.4009556571164));
#55040=CARTESIAN_POINT('Ctrl Pts',(-2.9701964131236,-1.,-2.40438604734919));
#55041=CARTESIAN_POINT('Ctrl Pts',(-2.9701964131236,1.,-2.40438604734919));
#55042=CARTESIAN_POINT('Ctrl Pts',(-2.97646002822422,-1.,-2.40768975073713));
#55043=CARTESIAN_POINT('Ctrl Pts',(-2.97646002822422,1.,-2.40768975073713));
#55044=CARTESIAN_POINT('Ctrl Pts',(-2.98280015815107,-1.,-2.41095909342571));
#55045=CARTESIAN_POINT('Ctrl Pts',(-2.98280015815107,1.,-2.41095909342571));
#55046=CARTESIAN_POINT('Ctrl Pts',(-2.98927983005796,-1.,-2.41425064199586));
#55047=CARTESIAN_POINT('Ctrl Pts',(-2.98927983005796,1.,-2.41425064199586));
#55048=CARTESIAN_POINT('Ctrl Pts',(-2.99590509293503,-1.,-2.41757324500514));
#55049=CARTESIAN_POINT('Ctrl Pts',(-2.99590509293503,1.,-2.41757324500514));
#55050=CARTESIAN_POINT('Ctrl Pts',(-3.00264868585996,-1.,-2.42090763946779));
#55051=CARTESIAN_POINT('Ctrl Pts',(-3.00264868585996,1.,-2.42090763946779));
#55052=CARTESIAN_POINT('Ctrl Pts',(-3.00946442616658,-1.,-2.42421849439613));
#55053=CARTESIAN_POINT('Ctrl Pts',(-3.00946442616658,1.,-2.42421849439613));
#55054=CARTESIAN_POINT('Ctrl Pts',(-3.01630420830504,-1.,-2.42746856264168));
#55055=CARTESIAN_POINT('Ctrl Pts',(-3.01630420830504,1.,-2.42746856264168));
#55056=CARTESIAN_POINT('Ctrl Pts',(-3.02313656036004,-1.,-2.43063415586637));
#55057=CARTESIAN_POINT('Ctrl Pts',(-3.02313656036004,1.,-2.43063415586637));
#55058=CARTESIAN_POINT('Ctrl Pts',(-3.02995534946978,-1.,-2.43371241361488));
#55059=CARTESIAN_POINT('Ctrl Pts',(-3.02995534946978,1.,-2.43371241361488));
#55060=CARTESIAN_POINT('Ctrl Pts',(-3.03676949672821,-1.,-2.43671278042414));
#55061=CARTESIAN_POINT('Ctrl Pts',(-3.03676949672821,1.,-2.43671278042414));
#55062=CARTESIAN_POINT('Ctrl Pts',(-3.04359685040555,-1.,-2.43965194061857));
#55063=CARTESIAN_POINT('Ctrl Pts',(-3.04359685040555,1.,-2.43965194061857));
#55064=CARTESIAN_POINT('Ctrl Pts',(-3.05045678021504,-1.,-2.44254768923105));
#55065=CARTESIAN_POINT('Ctrl Pts',(-3.05045678021504,1.,-2.44254768923105));
#55066=CARTESIAN_POINT('Ctrl Pts',(-3.05736242671506,-1.,-2.44541251892556));
#55067=CARTESIAN_POINT('Ctrl Pts',(-3.05736242671506,1.,-2.44541251892556));
#55068=CARTESIAN_POINT('Ctrl Pts',(-3.06431596421405,-1.,-2.44824970516544));
#55069=CARTESIAN_POINT('Ctrl Pts',(-3.06431596421405,1.,-2.44824970516544));
#55070=CARTESIAN_POINT('Ctrl Pts',(-3.07131290521297,-1.,-2.45105688854422));
#55071=CARTESIAN_POINT('Ctrl Pts',(-3.07131290521297,1.,-2.45105688854422));
#55072=CARTESIAN_POINT('Ctrl Pts',(-3.07834472886139,-1.,-2.4538282678779));
#55073=CARTESIAN_POINT('Ctrl Pts',(-3.07834472886139,1.,-2.4538282678779));
#55074=CARTESIAN_POINT('Ctrl Pts',(-3.08540206545315,-1.,-2.45655725437039));
#55075=CARTESIAN_POINT('Ctrl Pts',(-3.08540206545315,1.,-2.45655725437039));
#55076=CARTESIAN_POINT('Ctrl Pts',(-3.09247787931887,-1.,-2.4592391256388));
#55077=CARTESIAN_POINT('Ctrl Pts',(-3.09247787931887,1.,-2.4592391256388));
#55078=CARTESIAN_POINT('Ctrl Pts',(-3.09956993697052,-1.,-2.46187308501884));
#55079=CARTESIAN_POINT('Ctrl Pts',(-3.09956993697052,1.,-2.46187308501884));
#55080=CARTESIAN_POINT('Ctrl Pts',(-3.1066790790198,-1.,-2.46446082979646));
#55081=CARTESIAN_POINT('Ctrl Pts',(-3.1066790790198,1.,-2.46446082979646));
#55082=CARTESIAN_POINT('Ctrl Pts',(-3.11380805536122,-1.,-2.46700558843506));
#55083=CARTESIAN_POINT('Ctrl Pts',(-3.11380805536122,1.,-2.46700558843506));
#55084=CARTESIAN_POINT('Ctrl Pts',(-3.12096015766983,-1.,-2.46951098947469));
#55085=CARTESIAN_POINT('Ctrl Pts',(-3.12096015766983,1.,-2.46951098947469));
#55086=CARTESIAN_POINT('Ctrl Pts',(-3.12813790805952,-1.,-2.47197997765871));
#55087=CARTESIAN_POINT('Ctrl Pts',(-3.12813790805952,1.,-2.47197997765871));
#55088=CARTESIAN_POINT('Ctrl Pts',(-3.13534181229295,-1.,-2.47441378371932));
#55089=CARTESIAN_POINT('Ctrl Pts',(-3.13534181229295,1.,-2.47441378371932));
#55090=CARTESIAN_POINT('Ctrl Pts',(-3.1425709954655,-1.,-2.47681245356109));
#55091=CARTESIAN_POINT('Ctrl Pts',(-3.1425709954655,1.,-2.47681245356109));
#55092=CARTESIAN_POINT('Ctrl Pts',(-3.14982373241352,-1.,-2.47917529057029));
#55093=CARTESIAN_POINT('Ctrl Pts',(-3.14982373241352,1.,-2.47917529057029));
#55094=CARTESIAN_POINT('Ctrl Pts',(-3.15709802322739,-1.,-2.48150133566571));
#55095=CARTESIAN_POINT('Ctrl Pts',(-3.15709802322739,1.,-2.48150133566571));
#55096=CARTESIAN_POINT('Ctrl Pts',(-3.16439213290161,-1.,-2.48378981792725));
#55097=CARTESIAN_POINT('Ctrl Pts',(-3.16439213290161,1.,-2.48378981792725));
#55098=CARTESIAN_POINT('Ctrl Pts',(-3.17170518863313,-1.,-2.48604065348587));
#55099=CARTESIAN_POINT('Ctrl Pts',(-3.17170518863313,1.,-2.48604065348587));
#55100=CARTESIAN_POINT('Ctrl Pts',(-3.17903698136622,-1.,-2.48825428288201));
#55101=CARTESIAN_POINT('Ctrl Pts',(-3.17903698136622,1.,-2.48825428288201));
#55102=CARTESIAN_POINT('Ctrl Pts',(-3.18638771282266,-1.,-2.49043146334059));
#55103=CARTESIAN_POINT('Ctrl Pts',(-3.18638771282266,1.,-2.49043146334059));
#55104=CARTESIAN_POINT('Ctrl Pts',(-3.19375775555798,-1.,-2.49257307239848));
#55105=CARTESIAN_POINT('Ctrl Pts',(-3.19375775555798,1.,-2.49257307239848));
#55106=CARTESIAN_POINT('Ctrl Pts',(-3.20114742397588,-1.,-2.49467992057755));
#55107=CARTESIAN_POINT('Ctrl Pts',(-3.20114742397588,1.,-2.49467992057755));
#55108=CARTESIAN_POINT('Ctrl Pts',(-3.20855669849836,-1.,-2.4967525264737));
#55109=CARTESIAN_POINT('Ctrl Pts',(-3.20855669849836,1.,-2.4967525264737));
#55110=CARTESIAN_POINT('Ctrl Pts',(-3.21598526261286,-1.,-2.4987911459939));
#55111=CARTESIAN_POINT('Ctrl Pts',(-3.21598526261286,1.,-2.4987911459939));
#55112=CARTESIAN_POINT('Ctrl Pts',(-3.22343262620503,-1.,-2.50079587201957));
#55113=CARTESIAN_POINT('Ctrl Pts',(-3.22343262620503,1.,-2.50079587201957));
#55114=CARTESIAN_POINT('Ctrl Pts',(-3.23089822320646,-1.,-2.50276671338111));
#55115=CARTESIAN_POINT('Ctrl Pts',(-3.23089822320646,1.,-2.50276671338111));
#55116=CARTESIAN_POINT('Ctrl Pts',(-3.23838151080319,-1.,-2.5047036758003));
#55117=CARTESIAN_POINT('Ctrl Pts',(-3.23838151080319,1.,-2.5047036758003));
#55118=CARTESIAN_POINT('Ctrl Pts',(-3.24588208983849,-1.,-2.506606859405));
#55119=CARTESIAN_POINT('Ctrl Pts',(-3.24588208983849,1.,-2.506606859405));
#55120=CARTESIAN_POINT('Ctrl Pts',(-3.25339971460982,-1.,-2.50847647070723));
#55121=CARTESIAN_POINT('Ctrl Pts',(-3.25339971460982,1.,-2.50847647070723));
#55122=CARTESIAN_POINT('Ctrl Pts',(-3.26093423001434,-1.,-2.51031277813486));
#55123=CARTESIAN_POINT('Ctrl Pts',(-3.26093423001434,1.,-2.51031277813486));
#55124=CARTESIAN_POINT('Ctrl Pts',(-3.26848552888115,-1.,-2.51211608411423));
#55125=CARTESIAN_POINT('Ctrl Pts',(-3.26848552888115,1.,-2.51211608411423));
#55126=CARTESIAN_POINT('Ctrl Pts',(-3.27605350473142,-1.,-2.513886692704));
#55127=CARTESIAN_POINT('Ctrl Pts',(-3.27605350473142,1.,-2.513886692704));
#55128=CARTESIAN_POINT('Ctrl Pts',(-3.28363799702982,-1.,-2.51562487464514));
#55129=CARTESIAN_POINT('Ctrl Pts',(-3.28363799702982,1.,-2.51562487464514));
#55130=CARTESIAN_POINT('Ctrl Pts',(-3.2912387729927,-1.,-2.51733085123797));
#55131=CARTESIAN_POINT('Ctrl Pts',(-3.2912387729927,1.,-2.51733085123797));
#55132=CARTESIAN_POINT('Ctrl Pts',(-3.29885556388352,-1.,-2.51900480701069));
#55133=CARTESIAN_POINT('Ctrl Pts',(-3.29885556388352,1.,-2.51900480701069));
#55134=CARTESIAN_POINT('Ctrl Pts',(-3.30648808815442,-1.,-2.52064689568511));
#55135=CARTESIAN_POINT('Ctrl Pts',(-3.30648808815442,1.,-2.52064689568511));
#55136=CARTESIAN_POINT('Ctrl Pts',(-3.31413607874645,-1.,-2.52225724871313));
#55137=CARTESIAN_POINT('Ctrl Pts',(-3.31413607874645,1.,-2.52225724871313));
#55138=CARTESIAN_POINT('Ctrl Pts',(-3.32179931078699,-1.,-2.5238359839626));
#55139=CARTESIAN_POINT('Ctrl Pts',(-3.32179931078699,1.,-2.5238359839626));
#55140=CARTESIAN_POINT('Ctrl Pts',(-3.32947762187533,-1.,-2.52538321164634));
#55141=CARTESIAN_POINT('Ctrl Pts',(-3.32947762187533,1.,-2.52538321164634));
#55142=CARTESIAN_POINT('Ctrl Pts',(-3.33717089999103,-1.,-2.52689902690158));
#55143=CARTESIAN_POINT('Ctrl Pts',(-3.33717089999103,1.,-2.52689902690158));
#55144=CARTESIAN_POINT('Ctrl Pts',(-3.34333744115511,-1.,-2.52808660915689));
#55145=CARTESIAN_POINT('Ctrl Pts',(-3.34333744115511,1.,-2.52808660915689));
#55146=CARTESIAN_POINT('Ctrl Pts',(-3.34796903576663,-1.,-2.52896321610703));
#55147=CARTESIAN_POINT('Ctrl Pts',(-3.34796903576663,1.,-2.52896321610703));
#55148=CARTESIAN_POINT('Ctrl Pts',(-3.35105973714071,-1.,-2.5295413654909));
#55149=CARTESIAN_POINT('Ctrl Pts',(-3.35105973714071,1.,-2.5295413654909));
#55150=CARTESIAN_POINT('Ctrl Pts',(-3.35260583073571,-1.,-2.52982887637028));
#55151=CARTESIAN_POINT('Ctrl Pts',(-3.35260583073571,1.,-2.52982887637028));
#55152=CARTESIAN_POINT('',(-2.90994629141676,1.,-2.36531447826073));
#55153=CARTESIAN_POINT('Ctrl Pts',(-2.90994629141676,-1.,-2.36531447826074));
#55154=CARTESIAN_POINT('Ctrl Pts',(-2.90994629141676,-0.666666666666667,
-2.36531447826074));
#55155=CARTESIAN_POINT('Ctrl Pts',(-2.90994629141676,-0.333333333333333,
-2.36531447826074));
#55156=CARTESIAN_POINT('Ctrl Pts',(-2.90994629141676,0.333333333333333,
-2.36531447826074));
#55157=CARTESIAN_POINT('Ctrl Pts',(-2.90994629141676,0.666666666666667,
-2.36531447826074));
#55158=CARTESIAN_POINT('Ctrl Pts',(-2.90994629141676,1.,-2.36531447826074));
#55159=CARTESIAN_POINT('',(-3.35260583073571,1.,-2.52982887637028));
#55160=CARTESIAN_POINT('',(-3.35260583073571,0.,-2.52982887637028));
#55161=CARTESIAN_POINT('Ctrl Pts',(-2.90994629141676,1.,-2.36531447826073));
#55162=CARTESIAN_POINT('Ctrl Pts',(-2.90995756655606,1.,-2.36536211188453));
#55163=CARTESIAN_POINT('Ctrl Pts',(-2.91005770527719,1.,-2.36553202948613));
#55164=CARTESIAN_POINT('Ctrl Pts',(-2.91051690822156,1.,-2.36599991765749));
#55165=CARTESIAN_POINT('Ctrl Pts',(-2.91181344022549,1.,-2.36707658451664));
#55166=CARTESIAN_POINT('Ctrl Pts',(-2.9146124988314,1.,-2.36919161373173));
#55167=CARTESIAN_POINT('Ctrl Pts',(-2.91891503791411,1.,-2.37229381109821));
#55168=CARTESIAN_POINT('Ctrl Pts',(-2.92430340582608,1.,-2.3760651052403));
#55169=CARTESIAN_POINT('Ctrl Pts',(-2.93049643640206,1.,-2.38028989582073));
#55170=CARTESIAN_POINT('Ctrl Pts',(-2.93717903280391,1.,-2.38472771516311));
#55171=CARTESIAN_POINT('Ctrl Pts',(-2.94404820669076,1.,-2.38914929090759));
#55172=CARTESIAN_POINT('Ctrl Pts',(-2.95085857128439,1.,-2.39337207631667));
#55173=CARTESIAN_POINT('Ctrl Pts',(-2.95748006482942,1.,-2.39730553974517));
#55174=CARTESIAN_POINT('Ctrl Pts',(-2.96390432240312,1.,-2.4009556571164));
#55175=CARTESIAN_POINT('Ctrl Pts',(-2.9701964131236,1.,-2.40438604734919));
#55176=CARTESIAN_POINT('Ctrl Pts',(-2.97646002822422,1.,-2.40768975073713));
#55177=CARTESIAN_POINT('Ctrl Pts',(-2.98280015815107,1.,-2.41095909342571));
#55178=CARTESIAN_POINT('Ctrl Pts',(-2.98927983005796,1.,-2.41425064199586));
#55179=CARTESIAN_POINT('Ctrl Pts',(-2.99590509293503,1.,-2.41757324500514));
#55180=CARTESIAN_POINT('Ctrl Pts',(-3.00264868585996,1.,-2.42090763946779));
#55181=CARTESIAN_POINT('Ctrl Pts',(-3.00946442616658,1.,-2.42421849439613));
#55182=CARTESIAN_POINT('Ctrl Pts',(-3.01630420830504,1.,-2.42746856264168));
#55183=CARTESIAN_POINT('Ctrl Pts',(-3.02313656036004,1.,-2.43063415586637));
#55184=CARTESIAN_POINT('Ctrl Pts',(-3.02995534946978,1.,-2.43371241361488));
#55185=CARTESIAN_POINT('Ctrl Pts',(-3.03676949672821,1.,-2.43671278042414));
#55186=CARTESIAN_POINT('Ctrl Pts',(-3.04359685040555,1.,-2.43965194061857));
#55187=CARTESIAN_POINT('Ctrl Pts',(-3.05045678021504,1.,-2.44254768923105));
#55188=CARTESIAN_POINT('Ctrl Pts',(-3.05736242671506,1.,-2.44541251892556));
#55189=CARTESIAN_POINT('Ctrl Pts',(-3.06431596421405,1.,-2.44824970516544));
#55190=CARTESIAN_POINT('Ctrl Pts',(-3.07131290521297,1.,-2.45105688854422));
#55191=CARTESIAN_POINT('Ctrl Pts',(-3.07834472886139,1.,-2.4538282678779));
#55192=CARTESIAN_POINT('Ctrl Pts',(-3.08540206545315,1.,-2.45655725437039));
#55193=CARTESIAN_POINT('Ctrl Pts',(-3.09247787931887,1.,-2.4592391256388));
#55194=CARTESIAN_POINT('Ctrl Pts',(-3.09956993697052,1.,-2.46187308501884));
#55195=CARTESIAN_POINT('Ctrl Pts',(-3.1066790790198,1.,-2.46446082979646));
#55196=CARTESIAN_POINT('Ctrl Pts',(-3.11380805536122,1.,-2.46700558843506));
#55197=CARTESIAN_POINT('Ctrl Pts',(-3.12096015766983,1.,-2.46951098947469));
#55198=CARTESIAN_POINT('Ctrl Pts',(-3.12813790805952,1.,-2.47197997765871));
#55199=CARTESIAN_POINT('Ctrl Pts',(-3.13534181229295,1.,-2.47441378371932));
#55200=CARTESIAN_POINT('Ctrl Pts',(-3.1425709954655,1.,-2.47681245356109));
#55201=CARTESIAN_POINT('Ctrl Pts',(-3.14982373241352,1.,-2.47917529057029));
#55202=CARTESIAN_POINT('Ctrl Pts',(-3.15709802322739,1.,-2.48150133566571));
#55203=CARTESIAN_POINT('Ctrl Pts',(-3.16439213290161,1.,-2.48378981792725));
#55204=CARTESIAN_POINT('Ctrl Pts',(-3.17170518863313,1.,-2.48604065348587));
#55205=CARTESIAN_POINT('Ctrl Pts',(-3.17903698136622,1.,-2.48825428288201));
#55206=CARTESIAN_POINT('Ctrl Pts',(-3.18638771282266,1.,-2.49043146334059));
#55207=CARTESIAN_POINT('Ctrl Pts',(-3.19375775555798,1.,-2.49257307239848));
#55208=CARTESIAN_POINT('Ctrl Pts',(-3.20114742397588,1.,-2.49467992057755));
#55209=CARTESIAN_POINT('Ctrl Pts',(-3.20855669849836,1.,-2.4967525264737));
#55210=CARTESIAN_POINT('Ctrl Pts',(-3.21598526261286,1.,-2.4987911459939));
#55211=CARTESIAN_POINT('Ctrl Pts',(-3.22343262620503,1.,-2.50079587201957));
#55212=CARTESIAN_POINT('Ctrl Pts',(-3.23089822320646,1.,-2.50276671338111));
#55213=CARTESIAN_POINT('Ctrl Pts',(-3.23838151080319,1.,-2.5047036758003));
#55214=CARTESIAN_POINT('Ctrl Pts',(-3.24588208983849,1.,-2.506606859405));
#55215=CARTESIAN_POINT('Ctrl Pts',(-3.25339971460982,1.,-2.50847647070723));
#55216=CARTESIAN_POINT('Ctrl Pts',(-3.26093423001434,1.,-2.51031277813486));
#55217=CARTESIAN_POINT('Ctrl Pts',(-3.26848552888115,1.,-2.51211608411423));
#55218=CARTESIAN_POINT('Ctrl Pts',(-3.27605350473142,1.,-2.513886692704));
#55219=CARTESIAN_POINT('Ctrl Pts',(-3.28363799702982,1.,-2.51562487464514));
#55220=CARTESIAN_POINT('Ctrl Pts',(-3.2912387729927,1.,-2.51733085123797));
#55221=CARTESIAN_POINT('Ctrl Pts',(-3.29885556388352,1.,-2.51900480701069));
#55222=CARTESIAN_POINT('Ctrl Pts',(-3.30648808815442,1.,-2.52064689568511));
#55223=CARTESIAN_POINT('Ctrl Pts',(-3.31413607874645,1.,-2.52225724871313));
#55224=CARTESIAN_POINT('Ctrl Pts',(-3.32179931078699,1.,-2.5238359839626));
#55225=CARTESIAN_POINT('Ctrl Pts',(-3.32947762187533,1.,-2.52538321164634));
#55226=CARTESIAN_POINT('Ctrl Pts',(-3.33717089999103,1.,-2.52689902690158));
#55227=CARTESIAN_POINT('Ctrl Pts',(-3.34333744115511,1.,-2.52808660915689));
#55228=CARTESIAN_POINT('Ctrl Pts',(-3.34796903576663,1.,-2.52896321610703));
#55229=CARTESIAN_POINT('Ctrl Pts',(-3.35105973714071,1.,-2.5295413654909));
#55230=CARTESIAN_POINT('Ctrl Pts',(-3.35260583073571,1.,-2.52982887637028));
#55231=CARTESIAN_POINT('Origin',(-3.35260583073571,0.,-2.52982887637028));
#55232=CARTESIAN_POINT('',(-3.44202241512147,1.,-2.40675750623143));
#55233=CARTESIAN_POINT('Origin',(0.,0.,0.));
#55234=CARTESIAN_POINT('',(-2.79140942341378,1.,-2.50410331873042));
#55235=CARTESIAN_POINT('Origin',(0.,1.,0.));
#55236=CARTESIAN_POINT('Ctrl Pts',(-2.79140942341378,1.,-2.50410331873042));
#55237=CARTESIAN_POINT('Ctrl Pts',(-2.79140942341378,0.666666666666667,
-2.50410331873042));
#55238=CARTESIAN_POINT('Ctrl Pts',(-2.79140942341378,0.333333333333333,
-2.50410331873042));
#55239=CARTESIAN_POINT('Ctrl Pts',(-2.79140942341378,-0.333333333333333,
-2.50410331873042));
#55240=CARTESIAN_POINT('Ctrl Pts',(-2.79140942341378,-0.666666666666667,
-2.50410331873042));
#55241=CARTESIAN_POINT('Ctrl Pts',(-2.79140942341378,-1.,-2.50410331873042));
#55242=CARTESIAN_POINT('Ctrl Pts',(-3.02314558451372,-1.,-2.91557726271063));
#55243=CARTESIAN_POINT('Ctrl Pts',(-3.02314558451372,1.,-2.91557726271063));
#55244=CARTESIAN_POINT('Ctrl Pts',(-3.02261975104912,-1.,-2.91409518070707));
#55245=CARTESIAN_POINT('Ctrl Pts',(-3.02261975104912,1.,-2.91409518070707));
#55246=CARTESIAN_POINT('Ctrl Pts',(-3.02156522743299,-1.,-2.91113297349052));
#55247=CARTESIAN_POINT('Ctrl Pts',(-3.02156522743299,1.,-2.91113297349052));
#55248=CARTESIAN_POINT('Ctrl Pts',(-3.01997487194926,-1.,-2.90669553303902));
#55249=CARTESIAN_POINT('Ctrl Pts',(-3.01997487194926,1.,-2.90669553303902));
#55250=CARTESIAN_POINT('Ctrl Pts',(-3.01783725123646,-1.,-2.90079069102661));
#55251=CARTESIAN_POINT('Ctrl Pts',(-3.01783725123646,1.,-2.90079069102661));
#55252=CARTESIAN_POINT('Ctrl Pts',(-3.01513660433291,-1.,-2.8934292556764));
#55253=CARTESIAN_POINT('Ctrl Pts',(-3.01513660433291,1.,-2.8934292556764));
#55254=CARTESIAN_POINT('Ctrl Pts',(-3.01240727309568,-1.,-2.88608751706796));
#55255=CARTESIAN_POINT('Ctrl Pts',(-3.01240727309568,1.,-2.88608751706796));
#55256=CARTESIAN_POINT('Ctrl Pts',(-3.0096491810855,-1.,-2.87876560072799));
#55257=CARTESIAN_POINT('Ctrl Pts',(-3.0096491810855,1.,-2.87876560072799));
#55258=CARTESIAN_POINT('Ctrl Pts',(-3.00686224485374,-1.,-2.87146368430104));
#55259=CARTESIAN_POINT('Ctrl Pts',(-3.00686224485374,1.,-2.87146368430104));
#55260=CARTESIAN_POINT('Ctrl Pts',(-3.00404638316245,-1.,-2.86418200833065));
#55261=CARTESIAN_POINT('Ctrl Pts',(-3.00404638316245,1.,-2.86418200833065));
#55262=CARTESIAN_POINT('Ctrl Pts',(-3.0012015079552,-1.,-2.85692085715129));
#55263=CARTESIAN_POINT('Ctrl Pts',(-3.0012015079552,1.,-2.85692085715129));
#55264=CARTESIAN_POINT('Ctrl Pts',(-2.99832751144566,-1.,-2.84968053289104));
#55265=CARTESIAN_POINT('Ctrl Pts',(-2.99832751144566,1.,-2.84968053289104));
#55266=CARTESIAN_POINT('Ctrl Pts',(-2.995424253416,-1.,-2.84246132984334));
#55267=CARTESIAN_POINT('Ctrl Pts',(-2.995424253416,1.,-2.84246132984334));
#55268=CARTESIAN_POINT('Ctrl Pts',(-2.99249155170479,-1.,-2.83526351254383));
#55269=CARTESIAN_POINT('Ctrl Pts',(-2.99249155170479,1.,-2.83526351254383));
#55270=CARTESIAN_POINT('Ctrl Pts',(-2.98952916401699,-1.,-2.82808728190402));
#55271=CARTESIAN_POINT('Ctrl Pts',(-2.98952916401699,1.,-2.82808728190402));
#55272=CARTESIAN_POINT('Ctrl Pts',(-2.98653680669434,-1.,-2.82093279065704));
#55273=CARTESIAN_POINT('Ctrl Pts',(-2.98653680669434,1.,-2.82093279065704));
#55274=CARTESIAN_POINT('Ctrl Pts',(-2.9835141977994,-1.,-2.81380019196454));
#55275=CARTESIAN_POINT('Ctrl Pts',(-2.9835141977994,1.,-2.81380019196454));
#55276=CARTESIAN_POINT('Ctrl Pts',(-2.98046109647299,-1.,-2.80668968101162));
#55277=CARTESIAN_POINT('Ctrl Pts',(-2.98046109647299,1.,-2.80668968101162));
#55278=CARTESIAN_POINT('Ctrl Pts',(-2.97737733718242,-1.,-2.79960153278186));
#55279=CARTESIAN_POINT('Ctrl Pts',(-2.97737733718242,1.,-2.79960153278186));
#55280=CARTESIAN_POINT('Ctrl Pts',(-2.97426288347475,-1.,-2.79253615718147));
#55281=CARTESIAN_POINT('Ctrl Pts',(-2.97426288347475,1.,-2.79253615718147));
#55282=CARTESIAN_POINT('Ctrl Pts',(-2.97111781461349,-1.,-2.78549409123657));
#55283=CARTESIAN_POINT('Ctrl Pts',(-2.97111781461349,1.,-2.78549409123657));
#55284=CARTESIAN_POINT('Ctrl Pts',(-2.9679422104295,-1.,-2.77847589542767));
#55285=CARTESIAN_POINT('Ctrl Pts',(-2.9679422104295,1.,-2.77847589542767));
#55286=CARTESIAN_POINT('Ctrl Pts',(-2.96473605585548,-1.,-2.77148206836464));
#55287=CARTESIAN_POINT('Ctrl Pts',(-2.96473605585548,1.,-2.77148206836464));
#55288=CARTESIAN_POINT('Ctrl Pts',(-2.96149914764832,-1.,-2.76451296269571));
#55289=CARTESIAN_POINT('Ctrl Pts',(-2.96149914764832,1.,-2.76451296269571));
#55290=CARTESIAN_POINT('Ctrl Pts',(-2.9582309766594,-1.,-2.75756867888393));
#55291=CARTESIAN_POINT('Ctrl Pts',(-2.9582309766594,1.,-2.75756867888393));
#55292=CARTESIAN_POINT('Ctrl Pts',(-2.95493069316211,-1.,-2.75064903318996));
#55293=CARTESIAN_POINT('Ctrl Pts',(-2.95493069316211,1.,-2.75064903318996));
#55294=CARTESIAN_POINT('Ctrl Pts',(-2.95159737214305,-1.,-2.7437537949221));
#55295=CARTESIAN_POINT('Ctrl Pts',(-2.95159737214305,1.,-2.7437537949221));
#55296=CARTESIAN_POINT('Ctrl Pts',(-2.94823023414381,-1.,-2.73688288329825));
#55297=CARTESIAN_POINT('Ctrl Pts',(-2.94823023414381,1.,-2.73688288329825));
#55298=CARTESIAN_POINT('Ctrl Pts',(-2.94482887675139,-1.,-2.73003657371613));
#55299=CARTESIAN_POINT('Ctrl Pts',(-2.94482887675139,1.,-2.73003657371613));
#55300=CARTESIAN_POINT('Ctrl Pts',(-2.94139351933882,-1.,-2.72321571511322));
#55301=CARTESIAN_POINT('Ctrl Pts',(-2.94139351933882,1.,-2.72321571511322));
#55302=CARTESIAN_POINT('Ctrl Pts',(-2.93792519474955,-1.,-2.71642190053575));
#55303=CARTESIAN_POINT('Ctrl Pts',(-2.93792519474955,1.,-2.71642190053575));
#55304=CARTESIAN_POINT('Ctrl Pts',(-2.93442516311168,-1.,-2.70965695523776));
#55305=CARTESIAN_POINT('Ctrl Pts',(-2.93442516311168,1.,-2.70965695523776));
#55306=CARTESIAN_POINT('Ctrl Pts',(-2.93089438233746,-1.,-2.70292247416881));
#55307=CARTESIAN_POINT('Ctrl Pts',(-2.93089438233746,1.,-2.70292247416881));
#55308=CARTESIAN_POINT('Ctrl Pts',(-2.92733294395268,-1.,-2.69621932864302));
#55309=CARTESIAN_POINT('Ctrl Pts',(-2.92733294395268,1.,-2.69621932864302));
#55310=CARTESIAN_POINT('Ctrl Pts',(-2.92373955325876,-1.,-2.68954721165342));
#55311=CARTESIAN_POINT('Ctrl Pts',(-2.92373955325876,1.,-2.68954721165342));
#55312=CARTESIAN_POINT('Ctrl Pts',(-2.92011090722152,-1.,-2.68290409279689));
#55313=CARTESIAN_POINT('Ctrl Pts',(-2.92011090722152,1.,-2.68290409279689));
#55314=CARTESIAN_POINT('Ctrl Pts',(-2.91644290704281,-1.,-2.67628728855309));
#55315=CARTESIAN_POINT('Ctrl Pts',(-2.91644290704281,1.,-2.67628728855309));
#55316=CARTESIAN_POINT('Ctrl Pts',(-2.91273193382876,-1.,-2.66969458792627));
#55317=CARTESIAN_POINT('Ctrl Pts',(-2.91273193382876,1.,-2.66969458792627));
#55318=CARTESIAN_POINT('Ctrl Pts',(-2.90897617968921,-1.,-2.66312542616808));
#55319=CARTESIAN_POINT('Ctrl Pts',(-2.90897617968921,1.,-2.66312542616808));
#55320=CARTESIAN_POINT('Ctrl Pts',(-2.90517678087467,-1.,-2.65658188464287));
#55321=CARTESIAN_POINT('Ctrl Pts',(-2.90517678087467,1.,-2.65658188464287));
#55322=CARTESIAN_POINT('Ctrl Pts',(-2.90133950224879,-1.,-2.65007017365576));
#55323=CARTESIAN_POINT('Ctrl Pts',(-2.90133950224879,1.,-2.65007017365576));
#55324=CARTESIAN_POINT('Ctrl Pts',(-2.89747231723361,-1.,-2.64359851684146));
#55325=CARTESIAN_POINT('Ctrl Pts',(-2.89747231723361,1.,-2.64359851684146));
#55326=CARTESIAN_POINT('Ctrl Pts',(-2.89358228854557,-1.,-2.63717442263944));
#55327=CARTESIAN_POINT('Ctrl Pts',(-2.89358228854557,1.,-2.63717442263944));
#55328=CARTESIAN_POINT('Ctrl Pts',(-2.88967244854243,-1.,-2.63080195420771));
#55329=CARTESIAN_POINT('Ctrl Pts',(-2.88967244854243,1.,-2.63080195420771));
#55330=CARTESIAN_POINT('Ctrl Pts',(-2.88573922195049,-1.,-2.62447947640253));
#55331=CARTESIAN_POINT('Ctrl Pts',(-2.88573922195049,1.,-2.62447947640253));
#55332=CARTESIAN_POINT('Ctrl Pts',(-2.88176821427502,-1.,-2.61819596473087));
#55333=CARTESIAN_POINT('Ctrl Pts',(-2.88176821427502,1.,-2.61819596473087));
#55334=CARTESIAN_POINT('Ctrl Pts',(-2.87773881947885,-1.,-2.61193507170928));
#55335=CARTESIAN_POINT('Ctrl Pts',(-2.87773881947885,1.,-2.61193507170928));
#55336=CARTESIAN_POINT('Ctrl Pts',(-2.87363176656475,-1.,-2.6056817788128));
#55337=CARTESIAN_POINT('Ctrl Pts',(-2.87363176656475,1.,-2.6056817788128));
#55338=CARTESIAN_POINT('Ctrl Pts',(-2.86943633170712,-1.,-2.59942875223202));
#55339=CARTESIAN_POINT('Ctrl Pts',(-2.86943633170712,1.,-2.59942875223202));
#55340=CARTESIAN_POINT('Ctrl Pts',(-2.86515629953528,-1.,-2.59318160184921));
#55341=CARTESIAN_POINT('Ctrl Pts',(-2.86515629953528,1.,-2.59318160184921));
#55342=CARTESIAN_POINT('Ctrl Pts',(-2.86081999003668,-1.,-2.5869677064356));
#55343=CARTESIAN_POINT('Ctrl Pts',(-2.86081999003668,1.,-2.5869677064356));
#55344=CARTESIAN_POINT('Ctrl Pts',(-2.85647171715147,-1.,-2.58082875254407));
#55345=CARTESIAN_POINT('Ctrl Pts',(-2.85647171715147,1.,-2.58082875254407));
#55346=CARTESIAN_POINT('Ctrl Pts',(-2.85215360144483,-1.,-2.57480482727128));
#55347=CARTESIAN_POINT('Ctrl Pts',(-2.85215360144483,1.,-2.57480482727128));
#55348=CARTESIAN_POINT('Ctrl Pts',(-2.84788893329091,-1.,-2.56891984251743));
#55349=CARTESIAN_POINT('Ctrl Pts',(-2.84788893329091,1.,-2.56891984251743));
#55350=CARTESIAN_POINT('Ctrl Pts',(-2.84366802680211,-1.,-2.56316920798489));
#55351=CARTESIAN_POINT('Ctrl Pts',(-2.84366802680211,1.,-2.56316920798489));
#55352=CARTESIAN_POINT('Ctrl Pts',(-2.83942515220699,-1.,-2.55749952145165));
#55353=CARTESIAN_POINT('Ctrl Pts',(-2.83942515220699,1.,-2.55749952145165));
#55354=CARTESIAN_POINT('Ctrl Pts',(-2.83505269592412,-1.,-2.55182152806964));
#55355=CARTESIAN_POINT('Ctrl Pts',(-2.83505269592412,1.,-2.55182152806964));
#55356=CARTESIAN_POINT('Ctrl Pts',(-2.83044254225794,-1.,-2.54604736792542));
#55357=CARTESIAN_POINT('Ctrl Pts',(-2.83044254225794,1.,-2.54604736792542));
#55358=CARTESIAN_POINT('Ctrl Pts',(-2.82552167649157,-1.,-2.54012272520141));
#55359=CARTESIAN_POINT('Ctrl Pts',(-2.82552167649157,1.,-2.54012272520141));
#55360=CARTESIAN_POINT('Ctrl Pts',(-2.82028550483744,-1.,-2.53405679667463));
#55361=CARTESIAN_POINT('Ctrl Pts',(-2.82028550483744,1.,-2.53405679667463));
#55362=CARTESIAN_POINT('Ctrl Pts',(-2.8148437904867,-1.,-2.52796388055457));
#55363=CARTESIAN_POINT('Ctrl Pts',(-2.8148437904867,1.,-2.52796388055457));
#55364=CARTESIAN_POINT('Ctrl Pts',(-2.80941521967234,-1.,-2.52205778589922));
#55365=CARTESIAN_POINT('Ctrl Pts',(-2.80941521967234,1.,-2.52205778589922));
#55366=CARTESIAN_POINT('Ctrl Pts',(-2.80427363984939,-1.,-2.51660190466067));
#55367=CARTESIAN_POINT('Ctrl Pts',(-2.80427363984939,1.,-2.51660190466067));
#55368=CARTESIAN_POINT('Ctrl Pts',(-2.79970585014308,-1.,-2.51186983687947));
#55369=CARTESIAN_POINT('Ctrl Pts',(-2.79970585014308,1.,-2.51186983687947));
#55370=CARTESIAN_POINT('Ctrl Pts',(-2.7959687805717,-1.,-2.50810555977564));
#55371=CARTESIAN_POINT('Ctrl Pts',(-2.7959687805717,1.,-2.50810555977564));
#55372=CARTESIAN_POINT('Ctrl Pts',(-2.79323694088143,-1.,-2.50547439929077));
#55373=CARTESIAN_POINT('Ctrl Pts',(-2.79323694088143,1.,-2.50547439929077));
#55374=CARTESIAN_POINT('Ctrl Pts',(-2.79192122906739,-1.,-2.50433799076945));
#55375=CARTESIAN_POINT('Ctrl Pts',(-2.79192122906739,1.,-2.50433799076945));
#55376=CARTESIAN_POINT('Ctrl Pts',(-2.79143626022225,-1.,-2.50404230339032));
#55377=CARTESIAN_POINT('Ctrl Pts',(-2.79143626022225,1.,-2.50404230339032));
#55378=CARTESIAN_POINT('Ctrl Pts',(-2.79133581100044,-1.,-2.50409239460011));
#55379=CARTESIAN_POINT('Ctrl Pts',(-2.79133581100044,1.,-2.50409239460011));
#55380=CARTESIAN_POINT('Ctrl Pts',(-2.79134130681569,-1.,-2.50417924854921));
#55381=CARTESIAN_POINT('Ctrl Pts',(-2.79134130681569,1.,-2.50417924854921));
#55382=CARTESIAN_POINT('',(-3.02314558451372,1.,-2.91557726271063));
#55383=CARTESIAN_POINT('Ctrl Pts',(-3.02314558451372,1.,-2.91557726271063));
#55384=CARTESIAN_POINT('Ctrl Pts',(-3.02261975104912,1.,-2.91409518070707));
#55385=CARTESIAN_POINT('Ctrl Pts',(-3.02156522743299,1.,-2.91113297349052));
#55386=CARTESIAN_POINT('Ctrl Pts',(-3.01997487194926,1.,-2.90669553303902));
#55387=CARTESIAN_POINT('Ctrl Pts',(-3.01783725123646,1.,-2.90079069102661));
#55388=CARTESIAN_POINT('Ctrl Pts',(-3.01513660433291,1.,-2.8934292556764));
#55389=CARTESIAN_POINT('Ctrl Pts',(-3.01240727309568,1.,-2.88608751706796));
#55390=CARTESIAN_POINT('Ctrl Pts',(-3.0096491810855,1.,-2.87876560072799));
#55391=CARTESIAN_POINT('Ctrl Pts',(-3.00686224485374,1.,-2.87146368430104));
#55392=CARTESIAN_POINT('Ctrl Pts',(-3.00404638316245,1.,-2.86418200833065));
#55393=CARTESIAN_POINT('Ctrl Pts',(-3.0012015079552,1.,-2.85692085715129));
#55394=CARTESIAN_POINT('Ctrl Pts',(-2.99832751144566,1.,-2.84968053289104));
#55395=CARTESIAN_POINT('Ctrl Pts',(-2.995424253416,1.,-2.84246132984334));
#55396=CARTESIAN_POINT('Ctrl Pts',(-2.99249155170479,1.,-2.83526351254383));
#55397=CARTESIAN_POINT('Ctrl Pts',(-2.98952916401699,1.,-2.82808728190402));
#55398=CARTESIAN_POINT('Ctrl Pts',(-2.98653680669434,1.,-2.82093279065704));
#55399=CARTESIAN_POINT('Ctrl Pts',(-2.9835141977994,1.,-2.81380019196454));
#55400=CARTESIAN_POINT('Ctrl Pts',(-2.98046109647299,1.,-2.80668968101162));
#55401=CARTESIAN_POINT('Ctrl Pts',(-2.97737733718242,1.,-2.79960153278186));
#55402=CARTESIAN_POINT('Ctrl Pts',(-2.97426288347475,1.,-2.79253615718147));
#55403=CARTESIAN_POINT('Ctrl Pts',(-2.97111781461349,1.,-2.78549409123657));
#55404=CARTESIAN_POINT('Ctrl Pts',(-2.9679422104295,1.,-2.77847589542767));
#55405=CARTESIAN_POINT('Ctrl Pts',(-2.96473605585548,1.,-2.77148206836464));
#55406=CARTESIAN_POINT('Ctrl Pts',(-2.96149914764832,1.,-2.76451296269571));
#55407=CARTESIAN_POINT('Ctrl Pts',(-2.9582309766594,1.,-2.75756867888393));
#55408=CARTESIAN_POINT('Ctrl Pts',(-2.95493069316211,1.,-2.75064903318996));
#55409=CARTESIAN_POINT('Ctrl Pts',(-2.95159737214305,1.,-2.7437537949221));
#55410=CARTESIAN_POINT('Ctrl Pts',(-2.94823023414381,1.,-2.73688288329825));
#55411=CARTESIAN_POINT('Ctrl Pts',(-2.94482887675139,1.,-2.73003657371613));
#55412=CARTESIAN_POINT('Ctrl Pts',(-2.94139351933882,1.,-2.72321571511322));
#55413=CARTESIAN_POINT('Ctrl Pts',(-2.93792519474955,1.,-2.71642190053575));
#55414=CARTESIAN_POINT('Ctrl Pts',(-2.93442516311168,1.,-2.70965695523776));
#55415=CARTESIAN_POINT('Ctrl Pts',(-2.93089438233746,1.,-2.70292247416881));
#55416=CARTESIAN_POINT('Ctrl Pts',(-2.92733294395268,1.,-2.69621932864302));
#55417=CARTESIAN_POINT('Ctrl Pts',(-2.92373955325876,1.,-2.68954721165342));
#55418=CARTESIAN_POINT('Ctrl Pts',(-2.92011090722152,1.,-2.68290409279689));
#55419=CARTESIAN_POINT('Ctrl Pts',(-2.91644290704281,1.,-2.67628728855309));
#55420=CARTESIAN_POINT('Ctrl Pts',(-2.91273193382876,1.,-2.66969458792627));
#55421=CARTESIAN_POINT('Ctrl Pts',(-2.90897617968921,1.,-2.66312542616808));
#55422=CARTESIAN_POINT('Ctrl Pts',(-2.90517678087467,1.,-2.65658188464287));
#55423=CARTESIAN_POINT('Ctrl Pts',(-2.90133950224879,1.,-2.65007017365576));
#55424=CARTESIAN_POINT('Ctrl Pts',(-2.89747231723361,1.,-2.64359851684146));
#55425=CARTESIAN_POINT('Ctrl Pts',(-2.89358228854557,1.,-2.63717442263944));
#55426=CARTESIAN_POINT('Ctrl Pts',(-2.88967244854243,1.,-2.63080195420771));
#55427=CARTESIAN_POINT('Ctrl Pts',(-2.88573922195049,1.,-2.62447947640253));
#55428=CARTESIAN_POINT('Ctrl Pts',(-2.88176821427502,1.,-2.61819596473087));
#55429=CARTESIAN_POINT('Ctrl Pts',(-2.87773881947885,1.,-2.61193507170928));
#55430=CARTESIAN_POINT('Ctrl Pts',(-2.87363176656475,1.,-2.6056817788128));
#55431=CARTESIAN_POINT('Ctrl Pts',(-2.86943633170712,1.,-2.59942875223202));
#55432=CARTESIAN_POINT('Ctrl Pts',(-2.86515629953528,1.,-2.59318160184921));
#55433=CARTESIAN_POINT('Ctrl Pts',(-2.86081999003668,1.,-2.5869677064356));
#55434=CARTESIAN_POINT('Ctrl Pts',(-2.85647171715147,1.,-2.58082875254407));
#55435=CARTESIAN_POINT('Ctrl Pts',(-2.85215360144483,1.,-2.57480482727128));
#55436=CARTESIAN_POINT('Ctrl Pts',(-2.84788893329091,1.,-2.56891984251743));
#55437=CARTESIAN_POINT('Ctrl Pts',(-2.84366802680211,1.,-2.56316920798489));
#55438=CARTESIAN_POINT('Ctrl Pts',(-2.83942515220699,1.,-2.55749952145165));
#55439=CARTESIAN_POINT('Ctrl Pts',(-2.83505269592412,1.,-2.55182152806964));
#55440=CARTESIAN_POINT('Ctrl Pts',(-2.83044254225794,1.,-2.54604736792542));
#55441=CARTESIAN_POINT('Ctrl Pts',(-2.82552167649157,1.,-2.54012272520141));
#55442=CARTESIAN_POINT('Ctrl Pts',(-2.82028550483744,1.,-2.53405679667463));
#55443=CARTESIAN_POINT('Ctrl Pts',(-2.8148437904867,1.,-2.52796388055457));
#55444=CARTESIAN_POINT('Ctrl Pts',(-2.80941521967234,1.,-2.52205778589922));
#55445=CARTESIAN_POINT('Ctrl Pts',(-2.80427363984939,1.,-2.51660190466067));
#55446=CARTESIAN_POINT('Ctrl Pts',(-2.79970585014308,1.,-2.51186983687947));
#55447=CARTESIAN_POINT('Ctrl Pts',(-2.7959687805717,1.,-2.50810555977564));
#55448=CARTESIAN_POINT('Ctrl Pts',(-2.79344192164204,1.,-2.50567182569153));
#55449=CARTESIAN_POINT('Ctrl Pts',(-2.79217568804874,1.,-2.50455968395235));
#55450=CARTESIAN_POINT('Ctrl Pts',(-2.79164172519039,1.,-2.50417932839344));
#55451=CARTESIAN_POINT('Ctrl Pts',(-2.79145823440899,1.,-2.50410700351427));
#55452=CARTESIAN_POINT('Ctrl Pts',(-2.79140942341378,1.,-2.50410331873043));
#55453=CARTESIAN_POINT('',(-3.02314558451372,0.,-2.91557726271063));
#55454=CARTESIAN_POINT('Ctrl Pts',(-2.50417924854921,-1.,-2.79134130681569));
#55455=CARTESIAN_POINT('Ctrl Pts',(-2.50417924854921,1.,-2.79134130681569));
#55456=CARTESIAN_POINT('Ctrl Pts',(-2.50409239460108,-1.,-2.7913358110015));
#55457=CARTESIAN_POINT('Ctrl Pts',(-2.50409239460108,1.,-2.7913358110015));
#55458=CARTESIAN_POINT('Ctrl Pts',(-2.50404230339286,-1.,-2.79143626022503));
#55459=CARTESIAN_POINT('Ctrl Pts',(-2.50404230339286,1.,-2.79143626022503));
#55460=CARTESIAN_POINT('Ctrl Pts',(-2.5043379907732,-1.,-2.79192122907148));
#55461=CARTESIAN_POINT('Ctrl Pts',(-2.5043379907732,1.,-2.79192122907148));
#55462=CARTESIAN_POINT('Ctrl Pts',(-2.50547439929414,-1.,-2.7932369408851));
#55463=CARTESIAN_POINT('Ctrl Pts',(-2.50547439929414,1.,-2.7932369408851));
#55464=CARTESIAN_POINT('Ctrl Pts',(-2.50810555977671,-1.,-2.79596878057287));
#55465=CARTESIAN_POINT('Ctrl Pts',(-2.50810555977671,1.,-2.79596878057287));
#55466=CARTESIAN_POINT('Ctrl Pts',(-2.51186983687818,-1.,-2.79970585014168));
#55467=CARTESIAN_POINT('Ctrl Pts',(-2.51186983687818,1.,-2.79970585014168));
#55468=CARTESIAN_POINT('Ctrl Pts',(-2.51660190465805,-1.,-2.80427363984653));
#55469=CARTESIAN_POINT('Ctrl Pts',(-2.51660190465805,1.,-2.80427363984653));
#55470=CARTESIAN_POINT('Ctrl Pts',(-2.52205778589653,-1.,-2.80941521966941));
#55471=CARTESIAN_POINT('Ctrl Pts',(-2.52205778589653,1.,-2.80941521966941));
#55472=CARTESIAN_POINT('Ctrl Pts',(-2.52796388055278,-1.,-2.81484379048475));
#55473=CARTESIAN_POINT('Ctrl Pts',(-2.52796388055278,1.,-2.81484379048475));
#55474=CARTESIAN_POINT('Ctrl Pts',(-2.53405679667412,-1.,-2.82028550483689));
#55475=CARTESIAN_POINT('Ctrl Pts',(-2.53405679667412,1.,-2.82028550483689));
#55476=CARTESIAN_POINT('Ctrl Pts',(-2.54012272520199,-1.,-2.8255216764922));
#55477=CARTESIAN_POINT('Ctrl Pts',(-2.54012272520199,1.,-2.8255216764922));
#55478=CARTESIAN_POINT('Ctrl Pts',(-2.54604736792655,-1.,-2.83044254225917));
#55479=CARTESIAN_POINT('Ctrl Pts',(-2.54604736792655,1.,-2.83044254225917));
#55480=CARTESIAN_POINT('Ctrl Pts',(-2.55182152807077,-1.,-2.83505269592536));
#55481=CARTESIAN_POINT('Ctrl Pts',(-2.55182152807077,1.,-2.83505269592536));
#55482=CARTESIAN_POINT('Ctrl Pts',(-2.55749952145241,-1.,-2.83942515220782));
#55483=CARTESIAN_POINT('Ctrl Pts',(-2.55749952145241,1.,-2.83942515220782));
#55484=CARTESIAN_POINT('Ctrl Pts',(-2.56316920798513,-1.,-2.84366802680237));
#55485=CARTESIAN_POINT('Ctrl Pts',(-2.56316920798513,1.,-2.84366802680237));
#55486=CARTESIAN_POINT('Ctrl Pts',(-2.56891984251721,-1.,-2.84788893329067));
#55487=CARTESIAN_POINT('Ctrl Pts',(-2.56891984251721,1.,-2.84788893329067));
#55488=CARTESIAN_POINT('Ctrl Pts',(-2.57480482727081,-1.,-2.85215360144431));
#55489=CARTESIAN_POINT('Ctrl Pts',(-2.57480482727081,1.,-2.85215360144431));
#55490=CARTESIAN_POINT('Ctrl Pts',(-2.58082875254357,-1.,-2.85647171715092));
#55491=CARTESIAN_POINT('Ctrl Pts',(-2.58082875254357,1.,-2.85647171715092));
#55492=CARTESIAN_POINT('Ctrl Pts',(-2.58696770643524,-1.,-2.86081999003629));
#55493=CARTESIAN_POINT('Ctrl Pts',(-2.58696770643524,1.,-2.86081999003629));
#55494=CARTESIAN_POINT('Ctrl Pts',(-2.59318160184908,-1.,-2.86515629953513));
#55495=CARTESIAN_POINT('Ctrl Pts',(-2.59318160184908,1.,-2.86515629953513));
#55496=CARTESIAN_POINT('Ctrl Pts',(-2.5994287522321,-1.,-2.86943633170722));
#55497=CARTESIAN_POINT('Ctrl Pts',(-2.5994287522321,1.,-2.86943633170722));
#55498=CARTESIAN_POINT('Ctrl Pts',(-2.60568177881303,-1.,-2.87363176656501));
#55499=CARTESIAN_POINT('Ctrl Pts',(-2.60568177881303,1.,-2.87363176656501));
#55500=CARTESIAN_POINT('Ctrl Pts',(-2.61193507170955,-1.,-2.87773881947915));
#55501=CARTESIAN_POINT('Ctrl Pts',(-2.61193507170955,1.,-2.87773881947915));
#55502=CARTESIAN_POINT('Ctrl Pts',(-2.61819596473108,-1.,-2.88176821427525));
#55503=CARTESIAN_POINT('Ctrl Pts',(-2.61819596473108,1.,-2.88176821427525));
#55504=CARTESIAN_POINT('Ctrl Pts',(-2.62447947640262,-1.,-2.88573922195059));
#55505=CARTESIAN_POINT('Ctrl Pts',(-2.62447947640262,1.,-2.88573922195059));
#55506=CARTESIAN_POINT('Ctrl Pts',(-2.63080195420767,-1.,-2.88967244854239));
#55507=CARTESIAN_POINT('Ctrl Pts',(-2.63080195420767,1.,-2.88967244854239));
#55508=CARTESIAN_POINT('Ctrl Pts',(-2.63717442263932,-1.,-2.89358228854544));
#55509=CARTESIAN_POINT('Ctrl Pts',(-2.63717442263932,1.,-2.89358228854544));
#55510=CARTESIAN_POINT('Ctrl Pts',(-2.64359851684131,-1.,-2.89747231723345));
#55511=CARTESIAN_POINT('Ctrl Pts',(-2.64359851684131,1.,-2.89747231723345));
#55512=CARTESIAN_POINT('Ctrl Pts',(-2.65007017365564,-1.,-2.90133950224867));
#55513=CARTESIAN_POINT('Ctrl Pts',(-2.65007017365564,1.,-2.90133950224867));
#55514=CARTESIAN_POINT('Ctrl Pts',(-2.65658188464282,-1.,-2.90517678087461));
#55515=CARTESIAN_POINT('Ctrl Pts',(-2.65658188464282,1.,-2.90517678087461));
#55516=CARTESIAN_POINT('Ctrl Pts',(-2.6631254261681,-1.,-2.90897617968923));
#55517=CARTESIAN_POINT('Ctrl Pts',(-2.6631254261681,1.,-2.90897617968923));
#55518=CARTESIAN_POINT('Ctrl Pts',(-2.66969458792631,-1.,-2.91273193382882));
#55519=CARTESIAN_POINT('Ctrl Pts',(-2.66969458792631,1.,-2.91273193382882));
#55520=CARTESIAN_POINT('Ctrl Pts',(-2.67628728855312,-1.,-2.91644290704285));
#55521=CARTESIAN_POINT('Ctrl Pts',(-2.67628728855312,1.,-2.91644290704285));
#55522=CARTESIAN_POINT('Ctrl Pts',(-2.68290409279688,-1.,-2.92011090722152));
#55523=CARTESIAN_POINT('Ctrl Pts',(-2.68290409279688,1.,-2.92011090722152));
#55524=CARTESIAN_POINT('Ctrl Pts',(-2.68954721165339,-1.,-2.92373955325875));
#55525=CARTESIAN_POINT('Ctrl Pts',(-2.68954721165339,1.,-2.92373955325875));
#55526=CARTESIAN_POINT('Ctrl Pts',(-2.69621932864301,-1.,-2.92733294395267));
#55527=CARTESIAN_POINT('Ctrl Pts',(-2.69621932864301,1.,-2.92733294395267));
#55528=CARTESIAN_POINT('Ctrl Pts',(-2.70292247416885,-1.,-2.93089438233749));
#55529=CARTESIAN_POINT('Ctrl Pts',(-2.70292247416885,1.,-2.93089438233749));
#55530=CARTESIAN_POINT('Ctrl Pts',(-2.70965695523787,-1.,-2.93442516311179));
#55531=CARTESIAN_POINT('Ctrl Pts',(-2.70965695523787,1.,-2.93442516311179));
#55532=CARTESIAN_POINT('Ctrl Pts',(-2.71642190053592,-1.,-2.93792519474972));
#55533=CARTESIAN_POINT('Ctrl Pts',(-2.71642190053592,1.,-2.93792519474972));
#55534=CARTESIAN_POINT('Ctrl Pts',(-2.72321571511337,-1.,-2.94139351933897));
#55535=CARTESIAN_POINT('Ctrl Pts',(-2.72321571511337,1.,-2.94139351933897));
#55536=CARTESIAN_POINT('Ctrl Pts',(-2.73003657371617,-1.,-2.94482887675143));
#55537=CARTESIAN_POINT('Ctrl Pts',(-2.73003657371617,1.,-2.94482887675143));
#55538=CARTESIAN_POINT('Ctrl Pts',(-2.73688288329808,-1.,-2.94823023414364));
#55539=CARTESIAN_POINT('Ctrl Pts',(-2.73688288329808,1.,-2.94823023414364));
#55540=CARTESIAN_POINT('Ctrl Pts',(-2.74375379492172,-1.,-2.95159737214266));
#55541=CARTESIAN_POINT('Ctrl Pts',(-2.74375379492172,1.,-2.95159737214266));
#55542=CARTESIAN_POINT('Ctrl Pts',(-2.75064903318947,-1.,-2.95493069316161));
#55543=CARTESIAN_POINT('Ctrl Pts',(-2.75064903318947,1.,-2.95493069316161));
#55544=CARTESIAN_POINT('Ctrl Pts',(-2.7575686788835,-1.,-2.95823097665896));
#55545=CARTESIAN_POINT('Ctrl Pts',(-2.7575686788835,1.,-2.95823097665896));
#55546=CARTESIAN_POINT('Ctrl Pts',(-2.76451296269557,-1.,-2.96149914764818));
#55547=CARTESIAN_POINT('Ctrl Pts',(-2.76451296269557,1.,-2.96149914764818));
#55548=CARTESIAN_POINT('Ctrl Pts',(-2.77148206836498,-1.,-2.96473605585583));
#55549=CARTESIAN_POINT('Ctrl Pts',(-2.77148206836498,1.,-2.96473605585583));
#55550=CARTESIAN_POINT('Ctrl Pts',(-2.7784758954285,-1.,-2.96794221043036));
#55551=CARTESIAN_POINT('Ctrl Pts',(-2.7784758954285,1.,-2.96794221043036));
#55552=CARTESIAN_POINT('Ctrl Pts',(-2.78549409123769,-1.,-2.97111781461465));
#55553=CARTESIAN_POINT('Ctrl Pts',(-2.78549409123769,1.,-2.97111781461465));
#55554=CARTESIAN_POINT('Ctrl Pts',(-2.79253615718248,-1.,-2.9742628834758));
#55555=CARTESIAN_POINT('Ctrl Pts',(-2.79253615718248,1.,-2.9742628834758));
#55556=CARTESIAN_POINT('Ctrl Pts',(-2.7996015327823,-1.,-2.97737733718287));
#55557=CARTESIAN_POINT('Ctrl Pts',(-2.7996015327823,1.,-2.97737733718287));
#55558=CARTESIAN_POINT('Ctrl Pts',(-2.80668968101106,-1.,-2.98046109647241));
#55559=CARTESIAN_POINT('Ctrl Pts',(-2.80668968101106,1.,-2.98046109647241));
#55560=CARTESIAN_POINT('Ctrl Pts',(-2.81380019196286,-1.,-2.98351419779767));
#55561=CARTESIAN_POINT('Ctrl Pts',(-2.81380019196286,1.,-2.98351419779767));
#55562=CARTESIAN_POINT('Ctrl Pts',(-2.82093279065457,-1.,-2.9865368066918));
#55563=CARTESIAN_POINT('Ctrl Pts',(-2.82093279065457,1.,-2.9865368066918));
#55564=CARTESIAN_POINT('Ctrl Pts',(-2.82808728190157,-1.,-2.98952916401446));
#55565=CARTESIAN_POINT('Ctrl Pts',(-2.82808728190157,1.,-2.98952916401446));
#55566=CARTESIAN_POINT('Ctrl Pts',(-2.83526351254248,-1.,-2.99249155170339));
#55567=CARTESIAN_POINT('Ctrl Pts',(-2.83526351254248,1.,-2.99249155170339));
#55568=CARTESIAN_POINT('Ctrl Pts',(-2.84246132984415,-1.,-2.99542425341685));
#55569=CARTESIAN_POINT('Ctrl Pts',(-2.84246132984415,1.,-2.99542425341685));
#55570=CARTESIAN_POINT('Ctrl Pts',(-2.84968053289451,-1.,-2.99832751144925));
#55571=CARTESIAN_POINT('Ctrl Pts',(-2.84968053289451,1.,-2.99832751144925));
#55572=CARTESIAN_POINT('Ctrl Pts',(-2.85692085715686,-1.,-3.00120150796095));
#55573=CARTESIAN_POINT('Ctrl Pts',(-2.85692085715686,1.,-3.00120150796095));
#55574=CARTESIAN_POINT('Ctrl Pts',(-2.86418200833667,-1.,-3.00404638316867));
#55575=CARTESIAN_POINT('Ctrl Pts',(-2.86418200833667,1.,-3.00404638316867));
#55576=CARTESIAN_POINT('Ctrl Pts',(-2.87146368430502,-1.,-3.00686224485784));
#55577=CARTESIAN_POINT('Ctrl Pts',(-2.87146368430502,1.,-3.00686224485784));
#55578=CARTESIAN_POINT('Ctrl Pts',(-2.87876560072727,-1.,-3.00964918108476));
#55579=CARTESIAN_POINT('Ctrl Pts',(-2.87876560072727,1.,-3.00964918108476));
#55580=CARTESIAN_POINT('Ctrl Pts',(-2.8860875170608,-1.,-3.01240727308829));
#55581=CARTESIAN_POINT('Ctrl Pts',(-2.8860875170608,1.,-3.01240727308829));
#55582=CARTESIAN_POINT('Ctrl Pts',(-2.89342925566321,-1.,-3.01513660431928));
#55583=CARTESIAN_POINT('Ctrl Pts',(-2.89342925566321,1.,-3.01513660431928));
#55584=CARTESIAN_POINT('Ctrl Pts',(-2.9007906910105,-1.,-3.01783725121981));
#55585=CARTESIAN_POINT('Ctrl Pts',(-2.9007906910105,1.,-3.01783725121981));
#55586=CARTESIAN_POINT('Ctrl Pts',(-2.90669553302526,-1.,-3.01997487193503));
#55587=CARTESIAN_POINT('Ctrl Pts',(-2.90669553302526,1.,-3.01997487193503));
#55588=CARTESIAN_POINT('Ctrl Pts',(-2.91113297348212,-1.,-3.02156522742431));
#55589=CARTESIAN_POINT('Ctrl Pts',(-2.91113297348212,1.,-3.02156522742431));
#55590=CARTESIAN_POINT('Ctrl Pts',(-2.91409518070399,-1.,-3.02261975104593));
#55591=CARTESIAN_POINT('Ctrl Pts',(-2.91409518070399,1.,-3.02261975104593));
#55592=CARTESIAN_POINT('Ctrl Pts',(-2.91557726271063,-1.,-3.02314558451372));
#55593=CARTESIAN_POINT('Ctrl Pts',(-2.91557726271063,1.,-3.02314558451372));
#55594=CARTESIAN_POINT('',(-2.50410331873176,1.,-2.79140942341258));
#55595=CARTESIAN_POINT('Ctrl Pts',(-2.50410331873176,-1.,-2.79140942341258));
#55596=CARTESIAN_POINT('Ctrl Pts',(-2.50410331873176,-0.666666666666667,
-2.79140942341258));
#55597=CARTESIAN_POINT('Ctrl Pts',(-2.50410331873176,-0.333333333333333,
-2.79140942341258));
#55598=CARTESIAN_POINT('Ctrl Pts',(-2.50410331873176,0.333333333333333,
-2.79140942341258));
#55599=CARTESIAN_POINT('Ctrl Pts',(-2.50410331873176,0.666666666666667,
-2.79140942341258));
#55600=CARTESIAN_POINT('Ctrl Pts',(-2.50410331873176,1.,-2.79140942341258));
#55601=CARTESIAN_POINT('',(-2.91557726271063,1.,-3.02314558451372));
#55602=CARTESIAN_POINT('',(-2.91557726271063,0.,-3.02314558451372));
#55603=CARTESIAN_POINT('Ctrl Pts',(-2.50410331873176,1.,-2.79140942341258));
#55604=CARTESIAN_POINT('Ctrl Pts',(-2.50410700351493,1.,-2.79145823440781));
#55605=CARTESIAN_POINT('Ctrl Pts',(-2.50417932839313,1.,-2.79164172518905));
#55606=CARTESIAN_POINT('Ctrl Pts',(-2.50455968395146,1.,-2.79217568804755));
#55607=CARTESIAN_POINT('Ctrl Pts',(-2.50567182569081,1.,-2.79344192164147));
#55608=CARTESIAN_POINT('Ctrl Pts',(-2.50810555977671,1.,-2.79596878057287));
#55609=CARTESIAN_POINT('Ctrl Pts',(-2.51186983687818,1.,-2.79970585014168));
#55610=CARTESIAN_POINT('Ctrl Pts',(-2.51660190465805,1.,-2.80427363984653));
#55611=CARTESIAN_POINT('Ctrl Pts',(-2.52205778589653,1.,-2.80941521966941));
#55612=CARTESIAN_POINT('Ctrl Pts',(-2.52796388055278,1.,-2.81484379048475));
#55613=CARTESIAN_POINT('Ctrl Pts',(-2.53405679667412,1.,-2.82028550483689));
#55614=CARTESIAN_POINT('Ctrl Pts',(-2.54012272520199,1.,-2.8255216764922));
#55615=CARTESIAN_POINT('Ctrl Pts',(-2.54604736792655,1.,-2.83044254225917));
#55616=CARTESIAN_POINT('Ctrl Pts',(-2.55182152807077,1.,-2.83505269592536));
#55617=CARTESIAN_POINT('Ctrl Pts',(-2.55749952145241,1.,-2.83942515220782));
#55618=CARTESIAN_POINT('Ctrl Pts',(-2.56316920798513,1.,-2.84366802680237));
#55619=CARTESIAN_POINT('Ctrl Pts',(-2.56891984251721,1.,-2.84788893329067));
#55620=CARTESIAN_POINT('Ctrl Pts',(-2.57480482727081,1.,-2.85215360144431));
#55621=CARTESIAN_POINT('Ctrl Pts',(-2.58082875254357,1.,-2.85647171715092));
#55622=CARTESIAN_POINT('Ctrl Pts',(-2.58696770643524,1.,-2.86081999003629));
#55623=CARTESIAN_POINT('Ctrl Pts',(-2.59318160184908,1.,-2.86515629953513));
#55624=CARTESIAN_POINT('Ctrl Pts',(-2.5994287522321,1.,-2.86943633170722));
#55625=CARTESIAN_POINT('Ctrl Pts',(-2.60568177881303,1.,-2.87363176656501));
#55626=CARTESIAN_POINT('Ctrl Pts',(-2.61193507170955,1.,-2.87773881947915));
#55627=CARTESIAN_POINT('Ctrl Pts',(-2.61819596473108,1.,-2.88176821427525));
#55628=CARTESIAN_POINT('Ctrl Pts',(-2.62447947640262,1.,-2.88573922195059));
#55629=CARTESIAN_POINT('Ctrl Pts',(-2.63080195420767,1.,-2.88967244854239));
#55630=CARTESIAN_POINT('Ctrl Pts',(-2.63717442263932,1.,-2.89358228854544));
#55631=CARTESIAN_POINT('Ctrl Pts',(-2.64359851684131,1.,-2.89747231723345));
#55632=CARTESIAN_POINT('Ctrl Pts',(-2.65007017365564,1.,-2.90133950224867));
#55633=CARTESIAN_POINT('Ctrl Pts',(-2.65658188464282,1.,-2.90517678087461));
#55634=CARTESIAN_POINT('Ctrl Pts',(-2.6631254261681,1.,-2.90897617968923));
#55635=CARTESIAN_POINT('Ctrl Pts',(-2.66969458792631,1.,-2.91273193382882));
#55636=CARTESIAN_POINT('Ctrl Pts',(-2.67628728855312,1.,-2.91644290704285));
#55637=CARTESIAN_POINT('Ctrl Pts',(-2.68290409279688,1.,-2.92011090722152));
#55638=CARTESIAN_POINT('Ctrl Pts',(-2.68954721165339,1.,-2.92373955325875));
#55639=CARTESIAN_POINT('Ctrl Pts',(-2.69621932864301,1.,-2.92733294395267));
#55640=CARTESIAN_POINT('Ctrl Pts',(-2.70292247416885,1.,-2.93089438233749));
#55641=CARTESIAN_POINT('Ctrl Pts',(-2.70965695523787,1.,-2.93442516311179));
#55642=CARTESIAN_POINT('Ctrl Pts',(-2.71642190053592,1.,-2.93792519474972));
#55643=CARTESIAN_POINT('Ctrl Pts',(-2.72321571511337,1.,-2.94139351933897));
#55644=CARTESIAN_POINT('Ctrl Pts',(-2.73003657371617,1.,-2.94482887675143));
#55645=CARTESIAN_POINT('Ctrl Pts',(-2.73688288329808,1.,-2.94823023414364));
#55646=CARTESIAN_POINT('Ctrl Pts',(-2.74375379492172,1.,-2.95159737214266));
#55647=CARTESIAN_POINT('Ctrl Pts',(-2.75064903318947,1.,-2.95493069316161));
#55648=CARTESIAN_POINT('Ctrl Pts',(-2.7575686788835,1.,-2.95823097665896));
#55649=CARTESIAN_POINT('Ctrl Pts',(-2.76451296269557,1.,-2.96149914764818));
#55650=CARTESIAN_POINT('Ctrl Pts',(-2.77148206836498,1.,-2.96473605585583));
#55651=CARTESIAN_POINT('Ctrl Pts',(-2.7784758954285,1.,-2.96794221043036));
#55652=CARTESIAN_POINT('Ctrl Pts',(-2.78549409123769,1.,-2.97111781461465));
#55653=CARTESIAN_POINT('Ctrl Pts',(-2.79253615718248,1.,-2.9742628834758));
#55654=CARTESIAN_POINT('Ctrl Pts',(-2.7996015327823,1.,-2.97737733718287));
#55655=CARTESIAN_POINT('Ctrl Pts',(-2.80668968101106,1.,-2.98046109647241));
#55656=CARTESIAN_POINT('Ctrl Pts',(-2.81380019196286,1.,-2.98351419779767));
#55657=CARTESIAN_POINT('Ctrl Pts',(-2.82093279065457,1.,-2.9865368066918));
#55658=CARTESIAN_POINT('Ctrl Pts',(-2.82808728190157,1.,-2.98952916401446));
#55659=CARTESIAN_POINT('Ctrl Pts',(-2.83526351254248,1.,-2.99249155170339));
#55660=CARTESIAN_POINT('Ctrl Pts',(-2.84246132984415,1.,-2.99542425341685));
#55661=CARTESIAN_POINT('Ctrl Pts',(-2.84968053289451,1.,-2.99832751144925));
#55662=CARTESIAN_POINT('Ctrl Pts',(-2.85692085715686,1.,-3.00120150796095));
#55663=CARTESIAN_POINT('Ctrl Pts',(-2.86418200833667,1.,-3.00404638316867));
#55664=CARTESIAN_POINT('Ctrl Pts',(-2.87146368430502,1.,-3.00686224485784));
#55665=CARTESIAN_POINT('Ctrl Pts',(-2.87876560072727,1.,-3.00964918108476));
#55666=CARTESIAN_POINT('Ctrl Pts',(-2.8860875170608,1.,-3.01240727308829));
#55667=CARTESIAN_POINT('Ctrl Pts',(-2.89342925566321,1.,-3.01513660431928));
#55668=CARTESIAN_POINT('Ctrl Pts',(-2.9007906910105,1.,-3.01783725121981));
#55669=CARTESIAN_POINT('Ctrl Pts',(-2.90669553302526,1.,-3.01997487193503));
#55670=CARTESIAN_POINT('Ctrl Pts',(-2.91113297348212,1.,-3.02156522742431));
#55671=CARTESIAN_POINT('Ctrl Pts',(-2.91409518070399,1.,-3.02261975104593));
#55672=CARTESIAN_POINT('Ctrl Pts',(-2.91557726271063,1.,-3.02314558451372));
#55673=CARTESIAN_POINT('Origin',(-2.91557726271063,0.,-3.02314558451372));
#55674=CARTESIAN_POINT('',(-3.02314558451372,1.,-2.91557726271063));
#55675=CARTESIAN_POINT('Origin',(0.,0.,0.));
#55676=CARTESIAN_POINT('',(-2.36531447826213,1.,-2.90994629141562));
#55677=CARTESIAN_POINT('Origin',(0.,1.,0.));
#55678=CARTESIAN_POINT('Ctrl Pts',(-2.36531447826213,1.,-2.90994629141562));
#55679=CARTESIAN_POINT('Ctrl Pts',(-2.36531447826213,0.666666666666667,
-2.90994629141562));
#55680=CARTESIAN_POINT('Ctrl Pts',(-2.36531447826213,0.333333333333333,
-2.90994629141562));
#55681=CARTESIAN_POINT('Ctrl Pts',(-2.36531447826213,-0.333333333333333,
-2.90994629141562));
#55682=CARTESIAN_POINT('Ctrl Pts',(-2.36531447826213,-0.666666666666667,
-2.90994629141562));
#55683=CARTESIAN_POINT('Ctrl Pts',(-2.36531447826213,-1.,-2.90994629141562));
#55684=CARTESIAN_POINT('Ctrl Pts',(-2.52982887637028,-1.,-3.35260583073571));
#55685=CARTESIAN_POINT('Ctrl Pts',(-2.52982887637028,1.,-3.35260583073571));
#55686=CARTESIAN_POINT('Ctrl Pts',(-2.52954136549357,-1.,-3.35105973714426));
#55687=CARTESIAN_POINT('Ctrl Pts',(-2.52954136549357,1.,-3.35105973714426));
#55688=CARTESIAN_POINT('Ctrl Pts',(-2.5289632161143,-1.,-3.34796903577628));
#55689=CARTESIAN_POINT('Ctrl Pts',(-2.5289632161143,1.,-3.34796903577628));
#55690=CARTESIAN_POINT('Ctrl Pts',(-2.52808660916879,-1.,-3.34333744117093));
#55691=CARTESIAN_POINT('Ctrl Pts',(-2.52808660916879,1.,-3.34333744117093));
#55692=CARTESIAN_POINT('Ctrl Pts',(-2.52689902691551,-1.,-3.33717090000955));
#55693=CARTESIAN_POINT('Ctrl Pts',(-2.52689902691551,1.,-3.33717090000955));
#55694=CARTESIAN_POINT('Ctrl Pts',(-2.52538321165774,-1.,-3.32947762189049));
#55695=CARTESIAN_POINT('Ctrl Pts',(-2.52538321165774,1.,-3.32947762189049));
#55696=CARTESIAN_POINT('Ctrl Pts',(-2.52383598396878,-1.,-3.32179931079521));
#55697=CARTESIAN_POINT('Ctrl Pts',(-2.52383598396878,1.,-3.32179931079521));
#55698=CARTESIAN_POINT('Ctrl Pts',(-2.52225724871375,-1.,-3.31413607874727));
#55699=CARTESIAN_POINT('Ctrl Pts',(-2.52225724871375,1.,-3.31413607874727));
#55700=CARTESIAN_POINT('Ctrl Pts',(-2.52064689568167,-1.,-3.30648808814986));
#55701=CARTESIAN_POINT('Ctrl Pts',(-2.52064689568167,1.,-3.30648808814986));
#55702=CARTESIAN_POINT('Ctrl Pts',(-2.51900480700548,-1.,-3.29885556387661));
#55703=CARTESIAN_POINT('Ctrl Pts',(-2.51900480700548,1.,-3.29885556387661));
#55704=CARTESIAN_POINT('Ctrl Pts',(-2.51733085123316,-1.,-3.2912387729863));
#55705=CARTESIAN_POINT('Ctrl Pts',(-2.51733085123316,1.,-3.2912387729863));
#55706=CARTESIAN_POINT('Ctrl Pts',(-2.51562487464215,-1.,-3.28363799702583));
#55707=CARTESIAN_POINT('Ctrl Pts',(-2.51562487464215,1.,-3.28363799702583));
#55708=CARTESIAN_POINT('Ctrl Pts',(-2.51388669270329,-1.,-3.27605350473048));
#55709=CARTESIAN_POINT('Ctrl Pts',(-2.51388669270329,1.,-3.27605350473048));
#55710=CARTESIAN_POINT('Ctrl Pts',(-2.51211608411539,-1.,-3.26848552888271));
#55711=CARTESIAN_POINT('Ctrl Pts',(-2.51211608411539,1.,-3.26848552888271));
#55712=CARTESIAN_POINT('Ctrl Pts',(-2.51031277813697,-1.,-3.26093423001716));
#55713=CARTESIAN_POINT('Ctrl Pts',(-2.51031277813697,1.,-3.26093423001716));
#55714=CARTESIAN_POINT('Ctrl Pts',(-2.50847647070936,-1.,-3.25339971461265));
#55715=CARTESIAN_POINT('Ctrl Pts',(-2.50847647070936,1.,-3.25339971461265));
#55716=CARTESIAN_POINT('Ctrl Pts',(-2.50660685940645,-1.,-3.24588208984042));
#55717=CARTESIAN_POINT('Ctrl Pts',(-2.50660685940645,1.,-3.24588208984042));
#55718=CARTESIAN_POINT('Ctrl Pts',(-2.50470367580078,-1.,-3.23838151080383));
#55719=CARTESIAN_POINT('Ctrl Pts',(-2.50470367580078,1.,-3.23838151080383));
#55720=CARTESIAN_POINT('Ctrl Pts',(-2.50276671338074,-1.,-3.23089822320596));
#55721=CARTESIAN_POINT('Ctrl Pts',(-2.50276671338074,1.,-3.23089822320596));
#55722=CARTESIAN_POINT('Ctrl Pts',(-2.5007958720187,-1.,-3.22343262620387));
#55723=CARTESIAN_POINT('Ctrl Pts',(-2.5007958720187,1.,-3.22343262620387));
#55724=CARTESIAN_POINT('Ctrl Pts',(-2.49879114599293,-1.,-3.21598526261157));
#55725=CARTESIAN_POINT('Ctrl Pts',(-2.49879114599293,1.,-3.21598526261157));
#55726=CARTESIAN_POINT('Ctrl Pts',(-2.49675252647298,-1.,-3.2085566984974));
#55727=CARTESIAN_POINT('Ctrl Pts',(-2.49675252647298,1.,-3.2085566984974));
#55728=CARTESIAN_POINT('Ctrl Pts',(-2.49467992057726,-1.,-3.20114742397549));
#55729=CARTESIAN_POINT('Ctrl Pts',(-2.49467992057726,1.,-3.20114742397549));
#55730=CARTESIAN_POINT('Ctrl Pts',(-2.4925730723986,-1.,-3.19375775555814));
#55731=CARTESIAN_POINT('Ctrl Pts',(-2.4925730723986,1.,-3.19375775555814));
#55732=CARTESIAN_POINT('Ctrl Pts',(-2.49043146334095,-1.,-3.18638771282315));
#55733=CARTESIAN_POINT('Ctrl Pts',(-2.49043146334095,1.,-3.18638771282315));
#55734=CARTESIAN_POINT('Ctrl Pts',(-2.48825428288243,-1.,-3.17903698136679));
#55735=CARTESIAN_POINT('Ctrl Pts',(-2.48825428288243,1.,-3.17903698136679));
#55736=CARTESIAN_POINT('Ctrl Pts',(-2.48604065348619,-1.,-3.17170518863357));
#55737=CARTESIAN_POINT('Ctrl Pts',(-2.48604065348619,1.,-3.17170518863357));
#55738=CARTESIAN_POINT('Ctrl Pts',(-2.48378981792739,-1.,-3.16439213290181));
#55739=CARTESIAN_POINT('Ctrl Pts',(-2.48378981792739,1.,-3.16439213290181));
#55740=CARTESIAN_POINT('Ctrl Pts',(-2.48150133566568,-1.,-3.15709802322735));
#55741=CARTESIAN_POINT('Ctrl Pts',(-2.48150133566568,1.,-3.15709802322735));
#55742=CARTESIAN_POINT('Ctrl Pts',(-2.47917529057016,-1.,-3.14982373241335));
#55743=CARTESIAN_POINT('Ctrl Pts',(-2.47917529057016,1.,-3.14982373241335));
#55744=CARTESIAN_POINT('Ctrl Pts',(-2.47681245356095,-1.,-3.14257099546531));
#55745=CARTESIAN_POINT('Ctrl Pts',(-2.47681245356095,1.,-3.14257099546531));
#55746=CARTESIAN_POINT('Ctrl Pts',(-2.47441378371923,-1.,-3.13534181229282));
#55747=CARTESIAN_POINT('Ctrl Pts',(-2.47441378371923,1.,-3.13534181229282));
#55748=CARTESIAN_POINT('Ctrl Pts',(-2.47197997765868,-1.,-3.12813790805948));
#55749=CARTESIAN_POINT('Ctrl Pts',(-2.47197997765868,1.,-3.12813790805948));
#55750=CARTESIAN_POINT('Ctrl Pts',(-2.4695109894747,-1.,-3.12096015766984));
#55751=CARTESIAN_POINT('Ctrl Pts',(-2.4695109894747,1.,-3.12096015766984));
#55752=CARTESIAN_POINT('Ctrl Pts',(-2.46700558843507,-1.,-3.11380805536124));
#55753=CARTESIAN_POINT('Ctrl Pts',(-2.46700558843507,1.,-3.11380805536124));
#55754=CARTESIAN_POINT('Ctrl Pts',(-2.46446082979645,-1.,-3.10667907901981));
#55755=CARTESIAN_POINT('Ctrl Pts',(-2.46446082979645,1.,-3.10667907901981));
#55756=CARTESIAN_POINT('Ctrl Pts',(-2.4618730850188,-1.,-3.09956993697048));
#55757=CARTESIAN_POINT('Ctrl Pts',(-2.4618730850188,1.,-3.09956993697048));
#55758=CARTESIAN_POINT('Ctrl Pts',(-2.45923912563875,-1.,-3.09247787931881));
#55759=CARTESIAN_POINT('Ctrl Pts',(-2.45923912563875,1.,-3.09247787931881));
#55760=CARTESIAN_POINT('Ctrl Pts',(-2.45655725437037,-1.,-3.08540206545313));
#55761=CARTESIAN_POINT('Ctrl Pts',(-2.45655725437037,1.,-3.08540206545313));
#55762=CARTESIAN_POINT('Ctrl Pts',(-2.45382826787795,-1.,-3.07834472886145));
#55763=CARTESIAN_POINT('Ctrl Pts',(-2.45382826787795,1.,-3.07834472886145));
#55764=CARTESIAN_POINT('Ctrl Pts',(-2.45105688854432,-1.,-3.0713129052131));
#55765=CARTESIAN_POINT('Ctrl Pts',(-2.45105688854432,1.,-3.0713129052131));
#55766=CARTESIAN_POINT('Ctrl Pts',(-2.44824970516558,-1.,-3.06431596421422));
#55767=CARTESIAN_POINT('Ctrl Pts',(-2.44824970516558,1.,-3.06431596421422));
#55768=CARTESIAN_POINT('Ctrl Pts',(-2.44541251892568,-1.,-3.05736242671521));
#55769=CARTESIAN_POINT('Ctrl Pts',(-2.44541251892568,1.,-3.05736242671521));
#55770=CARTESIAN_POINT('Ctrl Pts',(-2.44254768923109,-1.,-3.05045678021509));
#55771=CARTESIAN_POINT('Ctrl Pts',(-2.44254768923109,1.,-3.05045678021509));
#55772=CARTESIAN_POINT('Ctrl Pts',(-2.43965194061849,-1.,-3.04359685040545));
#55773=CARTESIAN_POINT('Ctrl Pts',(-2.43965194061849,1.,-3.04359685040545));
#55774=CARTESIAN_POINT('Ctrl Pts',(-2.43671278042394,-1.,-3.03676949672797));
#55775=CARTESIAN_POINT('Ctrl Pts',(-2.43671278042394,1.,-3.03676949672797));
#55776=CARTESIAN_POINT('Ctrl Pts',(-2.43371241361462,-1.,-3.02995534946946));
#55777=CARTESIAN_POINT('Ctrl Pts',(-2.43371241361462,1.,-3.02995534946946));
#55778=CARTESIAN_POINT('Ctrl Pts',(-2.43063415586615,-1.,-3.02313656035977));
#55779=CARTESIAN_POINT('Ctrl Pts',(-2.43063415586615,1.,-3.02313656035977));
#55780=CARTESIAN_POINT('Ctrl Pts',(-2.4274685626416,-1.,-3.01630420830494));
#55781=CARTESIAN_POINT('Ctrl Pts',(-2.4274685626416,1.,-3.01630420830494));
#55782=CARTESIAN_POINT('Ctrl Pts',(-2.42421849439625,-1.,-3.00946442616674));
#55783=CARTESIAN_POINT('Ctrl Pts',(-2.42421849439625,1.,-3.00946442616674));
#55784=CARTESIAN_POINT('Ctrl Pts',(-2.42090763946812,-1.,-3.00264868586038));
#55785=CARTESIAN_POINT('Ctrl Pts',(-2.42090763946812,1.,-3.00264868586038));
#55786=CARTESIAN_POINT('Ctrl Pts',(-2.4175732450056,-1.,-2.99590509293561));
#55787=CARTESIAN_POINT('Ctrl Pts',(-2.4175732450056,1.,-2.99590509293561));
#55788=CARTESIAN_POINT('Ctrl Pts',(-2.4142506419963,-1.,-2.98927983005851));
#55789=CARTESIAN_POINT('Ctrl Pts',(-2.4142506419963,1.,-2.98927983005851));
#55790=CARTESIAN_POINT('Ctrl Pts',(-2.41095909342591,-1.,-2.98280015815132));
#55791=CARTESIAN_POINT('Ctrl Pts',(-2.41095909342591,1.,-2.98280015815132));
#55792=CARTESIAN_POINT('Ctrl Pts',(-2.40768975073691,-1.,-2.97646002822395));
#55793=CARTESIAN_POINT('Ctrl Pts',(-2.40768975073691,1.,-2.97646002822395));
#55794=CARTESIAN_POINT('Ctrl Pts',(-2.40438604734848,-1.,-2.97019641312272));
#55795=CARTESIAN_POINT('Ctrl Pts',(-2.40438604734848,1.,-2.97019641312272));
#55796=CARTESIAN_POINT('Ctrl Pts',(-2.40095565711535,-1.,-2.96390432240181));
#55797=CARTESIAN_POINT('Ctrl Pts',(-2.40095565711535,1.,-2.96390432240181));
#55798=CARTESIAN_POINT('Ctrl Pts',(-2.39730553974412,-1.,-2.95748006482811));
#55799=CARTESIAN_POINT('Ctrl Pts',(-2.39730553974412,1.,-2.95748006482811));
#55800=CARTESIAN_POINT('Ctrl Pts',(-2.39337207631613,-1.,-2.95085857128372));
#55801=CARTESIAN_POINT('Ctrl Pts',(-2.39337207631613,1.,-2.95085857128372));
#55802=CARTESIAN_POINT('Ctrl Pts',(-2.38914929090806,-1.,-2.94404820669135));
#55803=CARTESIAN_POINT('Ctrl Pts',(-2.38914929090806,1.,-2.94404820669135));
#55804=CARTESIAN_POINT('Ctrl Pts',(-2.38472771516476,-1.,-2.93717903280599));
#55805=CARTESIAN_POINT('Ctrl Pts',(-2.38472771516476,1.,-2.93717903280599));
#55806=CARTESIAN_POINT('Ctrl Pts',(-2.3802898958232,-1.,-2.93049643640517));
#55807=CARTESIAN_POINT('Ctrl Pts',(-2.3802898958232,1.,-2.93049643640517));
#55808=CARTESIAN_POINT('Ctrl Pts',(-2.37606510524271,-1.,-2.92430340582912));
#55809=CARTESIAN_POINT('Ctrl Pts',(-2.37606510524271,1.,-2.92430340582912));
#55810=CARTESIAN_POINT('Ctrl Pts',(-2.37229381109939,-1.,-2.9189150379156));
#55811=CARTESIAN_POINT('Ctrl Pts',(-2.37229381109939,1.,-2.9189150379156));
#55812=CARTESIAN_POINT('Ctrl Pts',(-2.36919161373074,-1.,-2.91461249883016));
#55813=CARTESIAN_POINT('Ctrl Pts',(-2.36919161373074,1.,-2.91461249883016));
#55814=CARTESIAN_POINT('Ctrl Pts',(-2.36690501170317,-1.,-2.9115863784165));
#55815=CARTESIAN_POINT('Ctrl Pts',(-2.36690501170317,1.,-2.9115863784165));
#55816=CARTESIAN_POINT('Ctrl Pts',(-2.36578327194396,-1.,-2.91025813829606));
#55817=CARTESIAN_POINT('Ctrl Pts',(-2.36578327194396,1.,-2.91025813829606));
#55818=CARTESIAN_POINT('Ctrl Pts',(-2.36535052956704,-1.,-2.90989022547738));
#55819=CARTESIAN_POINT('Ctrl Pts',(-2.36535052956704,1.,-2.90989022547738));
#55820=CARTESIAN_POINT('Ctrl Pts',(-2.36524348105023,-1.,-2.90992398626098));
#55821=CARTESIAN_POINT('Ctrl Pts',(-2.36524348105023,1.,-2.90992398626098));
#55822=CARTESIAN_POINT('Ctrl Pts',(-2.36523532225181,-1.,-2.91001063062876));
#55823=CARTESIAN_POINT('Ctrl Pts',(-2.36523532225181,1.,-2.91001063062876));
#55824=CARTESIAN_POINT('',(-2.52982887637028,1.,-3.35260583073571));
#55825=CARTESIAN_POINT('Ctrl Pts',(-2.52982887637028,1.,-3.35260583073571));
#55826=CARTESIAN_POINT('Ctrl Pts',(-2.52954136549357,1.,-3.35105973714426));
#55827=CARTESIAN_POINT('Ctrl Pts',(-2.5289632161143,1.,-3.34796903577628));
#55828=CARTESIAN_POINT('Ctrl Pts',(-2.52808660916879,1.,-3.34333744117093));
#55829=CARTESIAN_POINT('Ctrl Pts',(-2.52689902691551,1.,-3.33717090000955));
#55830=CARTESIAN_POINT('Ctrl Pts',(-2.52538321165774,1.,-3.32947762189049));
#55831=CARTESIAN_POINT('Ctrl Pts',(-2.52383598396878,1.,-3.32179931079521));
#55832=CARTESIAN_POINT('Ctrl Pts',(-2.52225724871375,1.,-3.31413607874727));
#55833=CARTESIAN_POINT('Ctrl Pts',(-2.52064689568167,1.,-3.30648808814986));
#55834=CARTESIAN_POINT('Ctrl Pts',(-2.51900480700548,1.,-3.29885556387661));
#55835=CARTESIAN_POINT('Ctrl Pts',(-2.51733085123316,1.,-3.2912387729863));
#55836=CARTESIAN_POINT('Ctrl Pts',(-2.51562487464215,1.,-3.28363799702583));
#55837=CARTESIAN_POINT('Ctrl Pts',(-2.51388669270329,1.,-3.27605350473048));
#55838=CARTESIAN_POINT('Ctrl Pts',(-2.51211608411539,1.,-3.26848552888271));
#55839=CARTESIAN_POINT('Ctrl Pts',(-2.51031277813697,1.,-3.26093423001716));
#55840=CARTESIAN_POINT('Ctrl Pts',(-2.50847647070936,1.,-3.25339971461265));
#55841=CARTESIAN_POINT('Ctrl Pts',(-2.50660685940645,1.,-3.24588208984042));
#55842=CARTESIAN_POINT('Ctrl Pts',(-2.50470367580078,1.,-3.23838151080383));
#55843=CARTESIAN_POINT('Ctrl Pts',(-2.50276671338074,1.,-3.23089822320596));
#55844=CARTESIAN_POINT('Ctrl Pts',(-2.5007958720187,1.,-3.22343262620387));
#55845=CARTESIAN_POINT('Ctrl Pts',(-2.49879114599293,1.,-3.21598526261157));
#55846=CARTESIAN_POINT('Ctrl Pts',(-2.49675252647298,1.,-3.2085566984974));
#55847=CARTESIAN_POINT('Ctrl Pts',(-2.49467992057726,1.,-3.20114742397549));
#55848=CARTESIAN_POINT('Ctrl Pts',(-2.4925730723986,1.,-3.19375775555814));
#55849=CARTESIAN_POINT('Ctrl Pts',(-2.49043146334095,1.,-3.18638771282315));
#55850=CARTESIAN_POINT('Ctrl Pts',(-2.48825428288243,1.,-3.17903698136679));
#55851=CARTESIAN_POINT('Ctrl Pts',(-2.48604065348619,1.,-3.17170518863357));
#55852=CARTESIAN_POINT('Ctrl Pts',(-2.48378981792739,1.,-3.16439213290181));
#55853=CARTESIAN_POINT('Ctrl Pts',(-2.48150133566568,1.,-3.15709802322735));
#55854=CARTESIAN_POINT('Ctrl Pts',(-2.47917529057016,1.,-3.14982373241335));
#55855=CARTESIAN_POINT('Ctrl Pts',(-2.47681245356095,1.,-3.14257099546531));
#55856=CARTESIAN_POINT('Ctrl Pts',(-2.47441378371923,1.,-3.13534181229282));
#55857=CARTESIAN_POINT('Ctrl Pts',(-2.47197997765868,1.,-3.12813790805948));
#55858=CARTESIAN_POINT('Ctrl Pts',(-2.4695109894747,1.,-3.12096015766984));
#55859=CARTESIAN_POINT('Ctrl Pts',(-2.46700558843507,1.,-3.11380805536124));
#55860=CARTESIAN_POINT('Ctrl Pts',(-2.46446082979645,1.,-3.10667907901981));
#55861=CARTESIAN_POINT('Ctrl Pts',(-2.4618730850188,1.,-3.09956993697048));
#55862=CARTESIAN_POINT('Ctrl Pts',(-2.45923912563875,1.,-3.09247787931881));
#55863=CARTESIAN_POINT('Ctrl Pts',(-2.45655725437037,1.,-3.08540206545313));
#55864=CARTESIAN_POINT('Ctrl Pts',(-2.45382826787795,1.,-3.07834472886145));
#55865=CARTESIAN_POINT('Ctrl Pts',(-2.45105688854432,1.,-3.0713129052131));
#55866=CARTESIAN_POINT('Ctrl Pts',(-2.44824970516558,1.,-3.06431596421422));
#55867=CARTESIAN_POINT('Ctrl Pts',(-2.44541251892568,1.,-3.05736242671521));
#55868=CARTESIAN_POINT('Ctrl Pts',(-2.44254768923109,1.,-3.05045678021509));
#55869=CARTESIAN_POINT('Ctrl Pts',(-2.43965194061849,1.,-3.04359685040545));
#55870=CARTESIAN_POINT('Ctrl Pts',(-2.43671278042394,1.,-3.03676949672797));
#55871=CARTESIAN_POINT('Ctrl Pts',(-2.43371241361462,1.,-3.02995534946946));
#55872=CARTESIAN_POINT('Ctrl Pts',(-2.43063415586615,1.,-3.02313656035977));
#55873=CARTESIAN_POINT('Ctrl Pts',(-2.4274685626416,1.,-3.01630420830494));
#55874=CARTESIAN_POINT('Ctrl Pts',(-2.42421849439625,1.,-3.00946442616674));
#55875=CARTESIAN_POINT('Ctrl Pts',(-2.42090763946812,1.,-3.00264868586038));
#55876=CARTESIAN_POINT('Ctrl Pts',(-2.4175732450056,1.,-2.99590509293561));
#55877=CARTESIAN_POINT('Ctrl Pts',(-2.4142506419963,1.,-2.98927983005851));
#55878=CARTESIAN_POINT('Ctrl Pts',(-2.41095909342591,1.,-2.98280015815132));
#55879=CARTESIAN_POINT('Ctrl Pts',(-2.40768975073691,1.,-2.97646002822395));
#55880=CARTESIAN_POINT('Ctrl Pts',(-2.40438604734848,1.,-2.97019641312272));
#55881=CARTESIAN_POINT('Ctrl Pts',(-2.40095565711535,1.,-2.96390432240181));
#55882=CARTESIAN_POINT('Ctrl Pts',(-2.39730553974412,1.,-2.95748006482811));
#55883=CARTESIAN_POINT('Ctrl Pts',(-2.39337207631613,1.,-2.95085857128372));
#55884=CARTESIAN_POINT('Ctrl Pts',(-2.38914929090806,1.,-2.94404820669135));
#55885=CARTESIAN_POINT('Ctrl Pts',(-2.38472771516476,1.,-2.93717903280599));
#55886=CARTESIAN_POINT('Ctrl Pts',(-2.3802898958232,1.,-2.93049643640517));
#55887=CARTESIAN_POINT('Ctrl Pts',(-2.37606510524271,1.,-2.92430340582912));
#55888=CARTESIAN_POINT('Ctrl Pts',(-2.37229381109939,1.,-2.9189150379156));
#55889=CARTESIAN_POINT('Ctrl Pts',(-2.36919161373074,1.,-2.91461249883016));
#55890=CARTESIAN_POINT('Ctrl Pts',(-2.36707658451709,1.,-2.91181344022628));
#55891=CARTESIAN_POINT('Ctrl Pts',(-2.36599991765853,1.,-2.91051690822262));
#55892=CARTESIAN_POINT('Ctrl Pts',(-2.36553202948741,1.,-2.9100577052777));
#55893=CARTESIAN_POINT('Ctrl Pts',(-2.3653621118858,1.,-2.90995756655559));
#55894=CARTESIAN_POINT('Ctrl Pts',(-2.36531447826213,1.,-2.90994629141563));
#55895=CARTESIAN_POINT('',(-2.52982887637028,0.,-3.35260583073571));
#55896=CARTESIAN_POINT('Ctrl Pts',(-2.03668666247593,-1.,-3.1487152044751));
#55897=CARTESIAN_POINT('Ctrl Pts',(-2.03668666247593,1.,-3.1487152044751));
#55898=CARTESIAN_POINT('Ctrl Pts',(-2.03660173757879,-1.,-3.14869618937258));
#55899=CARTESIAN_POINT('Ctrl Pts',(-2.03660173757879,1.,-3.14869618937258));
#55900=CARTESIAN_POINT('Ctrl Pts',(-2.03653654935592,-1.,-3.14878756590812));
#55901=CARTESIAN_POINT('Ctrl Pts',(-2.03653654935592,1.,-3.14878756590812));
#55902=CARTESIAN_POINT('Ctrl Pts',(-2.03675273049189,-1.,-3.14931281968048));
#55903=CARTESIAN_POINT('Ctrl Pts',(-2.03675273049189,1.,-3.14931281968048));
#55904=CARTESIAN_POINT('Ctrl Pts',(-2.03766932526445,-1.,-3.15079010635742));
#55905=CARTESIAN_POINT('Ctrl Pts',(-2.03766932526445,1.,-3.15079010635742));
#55906=CARTESIAN_POINT('Ctrl Pts',(-2.03984073791519,-1.,-3.15389991674792));
#55907=CARTESIAN_POINT('Ctrl Pts',(-2.03984073791519,1.,-3.15389991674792));
#55908=CARTESIAN_POINT('Ctrl Pts',(-2.04297406404027,-1.,-3.15817983946367));
#55909=CARTESIAN_POINT('Ctrl Pts',(-2.04297406404027,1.,-3.15817983946367));
#55910=CARTESIAN_POINT('Ctrl Pts',(-2.04693331247446,-1.,-3.16343165058912));
#55911=CARTESIAN_POINT('Ctrl Pts',(-2.04693331247446,1.,-3.16343165058912));
#55912=CARTESIAN_POINT('Ctrl Pts',(-2.05151770247233,-1.,-3.16936341689527));
#55913=CARTESIAN_POINT('Ctrl Pts',(-2.05151770247233,1.,-3.16936341689527));
#55914=CARTESIAN_POINT('Ctrl Pts',(-2.05650186773132,-1.,-3.17564906975371));
#55915=CARTESIAN_POINT('Ctrl Pts',(-2.05650186773132,1.,-3.17564906975371));
#55916=CARTESIAN_POINT('Ctrl Pts',(-2.06166849827101,-1.,-3.18197692964614));
#55917=CARTESIAN_POINT('Ctrl Pts',(-2.06166849827101,1.,-3.18197692964614));
#55918=CARTESIAN_POINT('Ctrl Pts',(-2.06684062744112,-1.,-3.18809755562368));
#55919=CARTESIAN_POINT('Ctrl Pts',(-2.06684062744112,1.,-3.18809755562368));
#55920=CARTESIAN_POINT('Ctrl Pts',(-2.07192253497857,-1.,-3.19388465568252));
#55921=CARTESIAN_POINT('Ctrl Pts',(-2.07192253497857,1.,-3.19388465568252));
#55922=CARTESIAN_POINT('Ctrl Pts',(-2.07690441870722,-1.,-3.19934132836019));
#55923=CARTESIAN_POINT('Ctrl Pts',(-2.07690441870722,1.,-3.19934132836019));
#55924=CARTESIAN_POINT('Ctrl Pts',(-2.08182850370878,-1.,-3.2045481863073));
#55925=CARTESIAN_POINT('Ctrl Pts',(-2.08182850370878,1.,-3.2045481863073));
#55926=CARTESIAN_POINT('Ctrl Pts',(-2.08676465517455,-1.,-3.20962575845463));
#55927=CARTESIAN_POINT('Ctrl Pts',(-2.08676465517455,1.,-3.20962575845463));
#55928=CARTESIAN_POINT('Ctrl Pts',(-2.09178419460443,-1.,-3.21469429601654));
#55929=CARTESIAN_POINT('Ctrl Pts',(-2.09178419460443,1.,-3.21469429601654));
#55930=CARTESIAN_POINT('Ctrl Pts',(-2.09692958434895,-1.,-3.21982707347009));
#55931=CARTESIAN_POINT('Ctrl Pts',(-2.09692958434895,1.,-3.21982707347009));
#55932=CARTESIAN_POINT('Ctrl Pts',(-2.10220384298492,-1.,-3.22503437553434));
#55933=CARTESIAN_POINT('Ctrl Pts',(-2.10220384298492,1.,-3.22503437553434));
#55934=CARTESIAN_POINT('Ctrl Pts',(-2.10758699642451,-1.,-3.23028945793289));
#55935=CARTESIAN_POINT('Ctrl Pts',(-2.10758699642451,1.,-3.23028945793289));
#55936=CARTESIAN_POINT('Ctrl Pts',(-2.11304604021773,-1.,-3.23554444767099));
#55937=CARTESIAN_POINT('Ctrl Pts',(-2.11304604021773,1.,-3.23554444767099));
#55938=CARTESIAN_POINT('Ctrl Pts',(-2.11854673326979,-1.,-3.24074905517293));
#55939=CARTESIAN_POINT('Ctrl Pts',(-2.11854673326979,1.,-3.24074905517293));
#55940=CARTESIAN_POINT('Ctrl Pts',(-2.12406646410962,-1.,-3.24587102613376));
#55941=CARTESIAN_POINT('Ctrl Pts',(-2.12406646410962,1.,-3.24587102613376));
#55942=CARTESIAN_POINT('Ctrl Pts',(-2.12960028396832,-1.,-3.25090574494028));
#55943=CARTESIAN_POINT('Ctrl Pts',(-2.12960028396832,1.,-3.25090574494028));
#55944=CARTESIAN_POINT('Ctrl Pts',(-2.13515375878803,-1.,-3.25586495065054));
#55945=CARTESIAN_POINT('Ctrl Pts',(-2.13515375878803,1.,-3.25586495065054));
#55946=CARTESIAN_POINT('Ctrl Pts',(-2.14073870754264,-1.,-3.26077002641879));
#55947=CARTESIAN_POINT('Ctrl Pts',(-2.14073870754264,1.,-3.26077002641879));
#55948=CARTESIAN_POINT('Ctrl Pts',(-2.1463680529566,-1.,-3.26564388189759));
#55949=CARTESIAN_POINT('Ctrl Pts',(-2.1463680529566,1.,-3.26564388189759));
#55950=CARTESIAN_POINT('Ctrl Pts',(-2.15205043199808,-1.,-3.27050245897228));
#55951=CARTESIAN_POINT('Ctrl Pts',(-2.15205043199808,1.,-3.27050245897228));
#55952=CARTESIAN_POINT('Ctrl Pts',(-2.15778690038347,-1.,-3.27534954469187));
#55953=CARTESIAN_POINT('Ctrl Pts',(-2.15778690038347,1.,-3.27534954469187));
#55954=CARTESIAN_POINT('Ctrl Pts',(-2.16357391934425,-1.,-3.280181508414));
#55955=CARTESIAN_POINT('Ctrl Pts',(-2.16357391934425,1.,-3.280181508414));
#55956=CARTESIAN_POINT('Ctrl Pts',(-2.16940517773455,-1.,-3.28499019979724));
#55957=CARTESIAN_POINT('Ctrl Pts',(-2.16940517773455,1.,-3.28499019979724));
#55958=CARTESIAN_POINT('Ctrl Pts',(-2.17527380048423,-1.,-3.28976645712568));
#55959=CARTESIAN_POINT('Ctrl Pts',(-2.17527380048423,1.,-3.28976645712568));
#55960=CARTESIAN_POINT('Ctrl Pts',(-2.18117455557065,-1.,-3.2945036150049));
#55961=CARTESIAN_POINT('Ctrl Pts',(-2.18117455557065,1.,-3.2945036150049));
#55962=CARTESIAN_POINT('Ctrl Pts',(-2.18710556500327,-1.,-3.29920022557639));
#55963=CARTESIAN_POINT('Ctrl Pts',(-2.18710556500327,1.,-3.29920022557639));
#55964=CARTESIAN_POINT('Ctrl Pts',(-2.19306710376111,-1.,-3.30385816281831));
#55965=CARTESIAN_POINT('Ctrl Pts',(-2.19306710376111,1.,-3.30385816281831));
#55966=CARTESIAN_POINT('Ctrl Pts',(-2.19906078949923,-1.,-3.30848134694595));
#55967=CARTESIAN_POINT('Ctrl Pts',(-2.19906078949923,1.,-3.30848134694595));
#55968=CARTESIAN_POINT('Ctrl Pts',(-2.20508863150607,-1.,-3.31307424608949));
#55969=CARTESIAN_POINT('Ctrl Pts',(-2.20508863150607,1.,-3.31307424608949));
#55970=CARTESIAN_POINT('Ctrl Pts',(-2.21115211847875,-1.,-3.31764044024235));
#55971=CARTESIAN_POINT('Ctrl Pts',(-2.21115211847875,1.,-3.31764044024235));
#55972=CARTESIAN_POINT('Ctrl Pts',(-2.21725135110898,-1.,-3.32218125618968));
#55973=CARTESIAN_POINT('Ctrl Pts',(-2.21725135110898,1.,-3.32218125618968));
#55974=CARTESIAN_POINT('Ctrl Pts',(-2.22338548312772,-1.,-3.3266964672289));
#55975=CARTESIAN_POINT('Ctrl Pts',(-2.22338548312772,1.,-3.3266964672289));
#55976=CARTESIAN_POINT('Ctrl Pts',(-2.22955308907233,-1.,-3.33118487773611));
#55977=CARTESIAN_POINT('Ctrl Pts',(-2.22955308907233,1.,-3.33118487773611));
#55978=CARTESIAN_POINT('Ctrl Pts',(-2.23575256328812,-1.,-3.33564495756482));
#55979=CARTESIAN_POINT('Ctrl Pts',(-2.23575256328812,1.,-3.33564495756482));
#55980=CARTESIAN_POINT('Ctrl Pts',(-2.24198249391422,-1.,-3.34007543738025));
#55981=CARTESIAN_POINT('Ctrl Pts',(-2.24198249391422,1.,-3.34007543738025));
#55982=CARTESIAN_POINT('Ctrl Pts',(-2.24824207678256,-1.,-3.34447596770723));
#55983=CARTESIAN_POINT('Ctrl Pts',(-2.24824207678256,1.,-3.34447596770723));
#55984=CARTESIAN_POINT('Ctrl Pts',(-2.25453097693483,-1.,-3.34884690292285));
#55985=CARTESIAN_POINT('Ctrl Pts',(-2.25453097693483,1.,-3.34884690292285));
#55986=CARTESIAN_POINT('Ctrl Pts',(-2.26084915222449,-1.,-3.35318902552626));
#55987=CARTESIAN_POINT('Ctrl Pts',(-2.26084915222449,1.,-3.35318902552626));
#55988=CARTESIAN_POINT('Ctrl Pts',(-2.2671966857991,-1.,-3.35750328523061));
#55989=CARTESIAN_POINT('Ctrl Pts',(-2.2671966857991,1.,-3.35750328523061));
#55990=CARTESIAN_POINT('Ctrl Pts',(-2.2735736262093,-1.,-3.36179055004409));
#55991=CARTESIAN_POINT('Ctrl Pts',(-2.2735736262093,1.,-3.36179055004409));
#55992=CARTESIAN_POINT('Ctrl Pts',(-2.27997979458037,-1.,-3.36605130713076));
#55993=CARTESIAN_POINT('Ctrl Pts',(-2.27997979458037,1.,-3.36605130713076));
#55994=CARTESIAN_POINT('Ctrl Pts',(-2.28641481081137,-1.,-3.37028570206488));
#55995=CARTESIAN_POINT('Ctrl Pts',(-2.28641481081137,1.,-3.37028570206488));
#55996=CARTESIAN_POINT('Ctrl Pts',(-2.29287818007393,-1.,-3.37449367172826));
#55997=CARTESIAN_POINT('Ctrl Pts',(-2.29287818007393,1.,-3.37449367172826));
#55998=CARTESIAN_POINT('Ctrl Pts',(-2.29936936127624,-1.,-3.37867504959433));
#55999=CARTESIAN_POINT('Ctrl Pts',(-2.29936936127624,1.,-3.37867504959433));
#56000=CARTESIAN_POINT('Ctrl Pts',(-2.30588783640343,-1.,-3.3828296733661));
#56001=CARTESIAN_POINT('Ctrl Pts',(-2.30588783640343,1.,-3.3828296733661));
#56002=CARTESIAN_POINT('Ctrl Pts',(-2.31243319489367,-1.,-3.38695751492462));
#56003=CARTESIAN_POINT('Ctrl Pts',(-2.31243319489367,1.,-3.38695751492462));
#56004=CARTESIAN_POINT('Ctrl Pts',(-2.31900513925424,-1.,-3.39105869474822));
#56005=CARTESIAN_POINT('Ctrl Pts',(-2.31900513925424,1.,-3.39105869474822));
#56006=CARTESIAN_POINT('Ctrl Pts',(-2.3256034390248,-1.,-3.39513342019756));
#56007=CARTESIAN_POINT('Ctrl Pts',(-2.3256034390248,1.,-3.39513342019756));
#56008=CARTESIAN_POINT('Ctrl Pts',(-2.33222789882489,-1.,-3.39918194577956));
#56009=CARTESIAN_POINT('Ctrl Pts',(-2.33222789882489,1.,-3.39918194577956));
#56010=CARTESIAN_POINT('Ctrl Pts',(-2.33887832342782,-1.,-3.40320452776743));
#56011=CARTESIAN_POINT('Ctrl Pts',(-2.33887832342782,1.,-3.40320452776743));
#56012=CARTESIAN_POINT('Ctrl Pts',(-2.34555447649188,-1.,-3.40720137404297));
#56013=CARTESIAN_POINT('Ctrl Pts',(-2.34555447649188,1.,-3.40720137404297));
#56014=CARTESIAN_POINT('Ctrl Pts',(-2.35225606824109,-1.,-3.41117262314119));
#56015=CARTESIAN_POINT('Ctrl Pts',(-2.35225606824109,1.,-3.41117262314119));
#56016=CARTESIAN_POINT('Ctrl Pts',(-2.35898278606946,-1.,-3.41511836751469));
#56017=CARTESIAN_POINT('Ctrl Pts',(-2.35898278606946,1.,-3.41511836751469));
#56018=CARTESIAN_POINT('Ctrl Pts',(-2.36573431470642,-1.,-3.41903866635852));
#56019=CARTESIAN_POINT('Ctrl Pts',(-2.36573431470642,1.,-3.41903866635852));
#56020=CARTESIAN_POINT('Ctrl Pts',(-2.37251035954292,-1.,-3.42293356216511));
#56021=CARTESIAN_POINT('Ctrl Pts',(-2.37251035954292,1.,-3.42293356216511));
#56022=CARTESIAN_POINT('Ctrl Pts',(-2.37931067028926,-1.,-3.42680309754399));
#56023=CARTESIAN_POINT('Ctrl Pts',(-2.37931067028926,1.,-3.42680309754399));
#56024=CARTESIAN_POINT('Ctrl Pts',(-2.38613505843552,-1.,-3.4306473271292));
#56025=CARTESIAN_POINT('Ctrl Pts',(-2.38613505843552,1.,-3.4306473271292));
#56026=CARTESIAN_POINT('Ctrl Pts',(-2.39298338804493,-1.,-3.4344663067854));
#56027=CARTESIAN_POINT('Ctrl Pts',(-2.39298338804493,1.,-3.4344663067854));
#56028=CARTESIAN_POINT('Ctrl Pts',(-2.39848113410292,-1.,-3.43750133064416));
#56029=CARTESIAN_POINT('Ctrl Pts',(-2.39848113410292,1.,-3.43750133064416));
#56030=CARTESIAN_POINT('Ctrl Pts',(-2.40261515589405,-1.,-3.43976627484234));
#56031=CARTESIAN_POINT('Ctrl Pts',(-2.40261515589405,1.,-3.43976627484234));
#56032=CARTESIAN_POINT('Ctrl Pts',(-2.4053759295909,-1.,-3.44127120683039));
#56033=CARTESIAN_POINT('Ctrl Pts',(-2.4053759295909,1.,-3.44127120683039));
#56034=CARTESIAN_POINT('Ctrl Pts',(-2.40675750623143,-1.,-3.44202241512147));
#56035=CARTESIAN_POINT('Ctrl Pts',(-2.40675750623143,1.,-3.44202241512147));
#56036=CARTESIAN_POINT('',(-2.03660101169714,1.,-3.14877060440328));
#56037=CARTESIAN_POINT('Ctrl Pts',(-2.03660101169715,-1.,-3.14877060440327));
#56038=CARTESIAN_POINT('Ctrl Pts',(-2.03660101169715,-0.666666666666667,
-3.14877060440327));
#56039=CARTESIAN_POINT('Ctrl Pts',(-2.03660101169715,-0.333333333333333,
-3.14877060440327));
#56040=CARTESIAN_POINT('Ctrl Pts',(-2.03660101169715,0.333333333333333,
-3.14877060440327));
#56041=CARTESIAN_POINT('Ctrl Pts',(-2.03660101169715,0.666666666666667,
-3.14877060440327));
#56042=CARTESIAN_POINT('Ctrl Pts',(-2.03660101169715,1.,-3.14877060440327));
#56043=CARTESIAN_POINT('',(-2.40675750623143,1.,-3.44202241512147));
#56044=CARTESIAN_POINT('',(-2.40675750623143,0.,-3.44202241512147));
#56045=CARTESIAN_POINT('Ctrl Pts',(-2.03660101169715,1.,-3.14877060440328));
#56046=CARTESIAN_POINT('Ctrl Pts',(-2.03659701539259,1.,-3.14881939088124));
#56047=CARTESIAN_POINT('Ctrl Pts',(-2.03663974554932,1.,-3.1490119366901));
#56048=CARTESIAN_POINT('Ctrl Pts',(-2.03693188810545,1.,-3.14959882629805));
#56049=CARTESIAN_POINT('Ctrl Pts',(-2.03783225495961,1.,-3.15102344775328));
#56050=CARTESIAN_POINT('Ctrl Pts',(-2.03984073791519,1.,-3.15389991674792));
#56051=CARTESIAN_POINT('Ctrl Pts',(-2.04297406404027,1.,-3.15817983946367));
#56052=CARTESIAN_POINT('Ctrl Pts',(-2.04693331247446,1.,-3.16343165058912));
#56053=CARTESIAN_POINT('Ctrl Pts',(-2.05151770247233,1.,-3.16936341689527));
#56054=CARTESIAN_POINT('Ctrl Pts',(-2.05650186773132,1.,-3.17564906975371));
#56055=CARTESIAN_POINT('Ctrl Pts',(-2.06166849827101,1.,-3.18197692964614));
#56056=CARTESIAN_POINT('Ctrl Pts',(-2.06684062744112,1.,-3.18809755562368));
#56057=CARTESIAN_POINT('Ctrl Pts',(-2.07192253497857,1.,-3.19388465568252));
#56058=CARTESIAN_POINT('Ctrl Pts',(-2.07690441870722,1.,-3.19934132836019));
#56059=CARTESIAN_POINT('Ctrl Pts',(-2.08182850370878,1.,-3.2045481863073));
#56060=CARTESIAN_POINT('Ctrl Pts',(-2.08676465517455,1.,-3.20962575845463));
#56061=CARTESIAN_POINT('Ctrl Pts',(-2.09178419460443,1.,-3.21469429601654));
#56062=CARTESIAN_POINT('Ctrl Pts',(-2.09692958434895,1.,-3.21982707347009));
#56063=CARTESIAN_POINT('Ctrl Pts',(-2.10220384298492,1.,-3.22503437553434));
#56064=CARTESIAN_POINT('Ctrl Pts',(-2.10758699642451,1.,-3.23028945793289));
#56065=CARTESIAN_POINT('Ctrl Pts',(-2.11304604021773,1.,-3.23554444767099));
#56066=CARTESIAN_POINT('Ctrl Pts',(-2.11854673326979,1.,-3.24074905517293));
#56067=CARTESIAN_POINT('Ctrl Pts',(-2.12406646410962,1.,-3.24587102613376));
#56068=CARTESIAN_POINT('Ctrl Pts',(-2.12960028396832,1.,-3.25090574494028));
#56069=CARTESIAN_POINT('Ctrl Pts',(-2.13515375878803,1.,-3.25586495065054));
#56070=CARTESIAN_POINT('Ctrl Pts',(-2.14073870754264,1.,-3.26077002641879));
#56071=CARTESIAN_POINT('Ctrl Pts',(-2.1463680529566,1.,-3.26564388189759));
#56072=CARTESIAN_POINT('Ctrl Pts',(-2.15205043199808,1.,-3.27050245897228));
#56073=CARTESIAN_POINT('Ctrl Pts',(-2.15778690038347,1.,-3.27534954469187));
#56074=CARTESIAN_POINT('Ctrl Pts',(-2.16357391934425,1.,-3.280181508414));
#56075=CARTESIAN_POINT('Ctrl Pts',(-2.16940517773455,1.,-3.28499019979724));
#56076=CARTESIAN_POINT('Ctrl Pts',(-2.17527380048423,1.,-3.28976645712568));
#56077=CARTESIAN_POINT('Ctrl Pts',(-2.18117455557065,1.,-3.2945036150049));
#56078=CARTESIAN_POINT('Ctrl Pts',(-2.18710556500327,1.,-3.29920022557639));
#56079=CARTESIAN_POINT('Ctrl Pts',(-2.19306710376111,1.,-3.30385816281831));
#56080=CARTESIAN_POINT('Ctrl Pts',(-2.19906078949923,1.,-3.30848134694595));
#56081=CARTESIAN_POINT('Ctrl Pts',(-2.20508863150607,1.,-3.31307424608949));
#56082=CARTESIAN_POINT('Ctrl Pts',(-2.21115211847875,1.,-3.31764044024235));
#56083=CARTESIAN_POINT('Ctrl Pts',(-2.21725135110898,1.,-3.32218125618968));
#56084=CARTESIAN_POINT('Ctrl Pts',(-2.22338548312772,1.,-3.3266964672289));
#56085=CARTESIAN_POINT('Ctrl Pts',(-2.22955308907233,1.,-3.33118487773611));
#56086=CARTESIAN_POINT('Ctrl Pts',(-2.23575256328812,1.,-3.33564495756482));
#56087=CARTESIAN_POINT('Ctrl Pts',(-2.24198249391422,1.,-3.34007543738025));
#56088=CARTESIAN_POINT('Ctrl Pts',(-2.24824207678256,1.,-3.34447596770723));
#56089=CARTESIAN_POINT('Ctrl Pts',(-2.25453097693483,1.,-3.34884690292285));
#56090=CARTESIAN_POINT('Ctrl Pts',(-2.26084915222449,1.,-3.35318902552626));
#56091=CARTESIAN_POINT('Ctrl Pts',(-2.2671966857991,1.,-3.35750328523061));
#56092=CARTESIAN_POINT('Ctrl Pts',(-2.2735736262093,1.,-3.36179055004409));
#56093=CARTESIAN_POINT('Ctrl Pts',(-2.27997979458037,1.,-3.36605130713076));
#56094=CARTESIAN_POINT('Ctrl Pts',(-2.28641481081137,1.,-3.37028570206488));
#56095=CARTESIAN_POINT('Ctrl Pts',(-2.29287818007393,1.,-3.37449367172826));
#56096=CARTESIAN_POINT('Ctrl Pts',(-2.29936936127624,1.,-3.37867504959433));
#56097=CARTESIAN_POINT('Ctrl Pts',(-2.30588783640343,1.,-3.3828296733661));
#56098=CARTESIAN_POINT('Ctrl Pts',(-2.31243319489367,1.,-3.38695751492462));
#56099=CARTESIAN_POINT('Ctrl Pts',(-2.31900513925424,1.,-3.39105869474822));
#56100=CARTESIAN_POINT('Ctrl Pts',(-2.3256034390248,1.,-3.39513342019756));
#56101=CARTESIAN_POINT('Ctrl Pts',(-2.33222789882489,1.,-3.39918194577956));
#56102=CARTESIAN_POINT('Ctrl Pts',(-2.33887832342782,1.,-3.40320452776743));
#56103=CARTESIAN_POINT('Ctrl Pts',(-2.34555447649188,1.,-3.40720137404297));
#56104=CARTESIAN_POINT('Ctrl Pts',(-2.35225606824109,1.,-3.41117262314119));
#56105=CARTESIAN_POINT('Ctrl Pts',(-2.35898278606946,1.,-3.41511836751469));
#56106=CARTESIAN_POINT('Ctrl Pts',(-2.36573431470642,1.,-3.41903866635852));
#56107=CARTESIAN_POINT('Ctrl Pts',(-2.37251035954292,1.,-3.42293356216511));
#56108=CARTESIAN_POINT('Ctrl Pts',(-2.37931067028926,1.,-3.42680309754399));
#56109=CARTESIAN_POINT('Ctrl Pts',(-2.38613505843552,1.,-3.4306473271292));
#56110=CARTESIAN_POINT('Ctrl Pts',(-2.39298338804493,1.,-3.4344663067854));
#56111=CARTESIAN_POINT('Ctrl Pts',(-2.39848113410292,1.,-3.43750133064416));
#56112=CARTESIAN_POINT('Ctrl Pts',(-2.40261515589405,1.,-3.43976627484234));
#56113=CARTESIAN_POINT('Ctrl Pts',(-2.4053759295909,1.,-3.44127120683039));
#56114=CARTESIAN_POINT('Ctrl Pts',(-2.40675750623143,1.,-3.44202241512147));
#56115=CARTESIAN_POINT('Origin',(-2.40675750623143,0.,-3.44202241512147));
#56116=CARTESIAN_POINT('',(-2.52982887637028,1.,-3.35260583073571));
#56117=CARTESIAN_POINT('Origin',(0.,0.,0.));
#56118=CARTESIAN_POINT('',(-1.88097764062697,1.,-3.24413672884812));
#56119=CARTESIAN_POINT('Origin',(0.,1.,0.));
#56120=CARTESIAN_POINT('Ctrl Pts',(-1.88097764062697,1.,-3.24413672884812));
#56121=CARTESIAN_POINT('Ctrl Pts',(-1.88097764062697,0.666666666666667,
-3.24413672884812));
#56122=CARTESIAN_POINT('Ctrl Pts',(-1.88097764062697,0.333333333333333,
-3.24413672884812));
#56123=CARTESIAN_POINT('Ctrl Pts',(-1.88097764062697,-0.333333333333333,
-3.24413672884812));
#56124=CARTESIAN_POINT('Ctrl Pts',(-1.88097764062697,-0.666666666666667,
-3.24413672884812));
#56125=CARTESIAN_POINT('Ctrl Pts',(-1.88097764062697,-1.,-3.24413672884812));
#56126=CARTESIAN_POINT('Ctrl Pts',(-1.97421938526992,-1.,-3.70708211654725));
#56127=CARTESIAN_POINT('Ctrl Pts',(-1.97421938526992,1.,-3.70708211654725));
#56128=CARTESIAN_POINT('Ctrl Pts',(-1.97417727645308,-1.,-3.70551008132332));
#56129=CARTESIAN_POINT('Ctrl Pts',(-1.97417727645308,1.,-3.70551008132332));
#56130=CARTESIAN_POINT('Ctrl Pts',(-1.97408973726715,-1.,-3.70236698912904));
#56131=CARTESIAN_POINT('Ctrl Pts',(-1.97408973726715,1.,-3.70236698912904));
#56132=CARTESIAN_POINT('Ctrl Pts',(-1.97394846383216,-1.,-3.6976552856004));
#56133=CARTESIAN_POINT('Ctrl Pts',(-1.97394846383216,1.,-3.6976552856004));
#56134=CARTESIAN_POINT('Ctrl Pts',(-1.97374016225483,-1.,-3.69137888599902));
#56135=CARTESIAN_POINT('Ctrl Pts',(-1.97374016225483,1.,-3.69137888599902));
#56136=CARTESIAN_POINT('Ctrl Pts',(-1.97344650304519,-1.,-3.68354319915092));
#56137=CARTESIAN_POINT('Ctrl Pts',(-1.97344650304519,1.,-3.68354319915092));
#56138=CARTESIAN_POINT('Ctrl Pts',(-1.97311947678517,-1.,-3.67571738107084));
#56139=CARTESIAN_POINT('Ctrl Pts',(-1.97311947678517,1.,-3.67571738107084));
#56140=CARTESIAN_POINT('Ctrl Pts',(-1.97275897198678,-1.,-3.66790152752075));
#56141=CARTESIAN_POINT('Ctrl Pts',(-1.97275897198678,1.,-3.66790152752075));
#56142=CARTESIAN_POINT('Ctrl Pts',(-1.9723648543905,-1.,-3.6600957816636));
#56143=CARTESIAN_POINT('Ctrl Pts',(-1.9723648543905,1.,-3.6600957816636));
#56144=CARTESIAN_POINT('Ctrl Pts',(-1.9719369724024,-1.,-3.652300347166));
#56145=CARTESIAN_POINT('Ctrl Pts',(-1.9719369724024,1.,-3.652300347166));
#56146=CARTESIAN_POINT('Ctrl Pts',(-1.97147515441164,-1.,-3.64451546723514));
#56147=CARTESIAN_POINT('Ctrl Pts',(-1.97147515441164,1.,-3.64451546723514));
#56148=CARTESIAN_POINT('Ctrl Pts',(-1.97097920454464,-1.,-3.63674139590412));
#56149=CARTESIAN_POINT('Ctrl Pts',(-1.97097920454464,1.,-3.63674139590412));
#56150=CARTESIAN_POINT('Ctrl Pts',(-1.97044889850463,-1.,-3.62897836973293));
#56151=CARTESIAN_POINT('Ctrl Pts',(-1.97044889850463,1.,-3.62897836973293));
#56152=CARTESIAN_POINT('Ctrl Pts',(-1.96988398129978,-1.,-3.62122658401893));
#56153=CARTESIAN_POINT('Ctrl Pts',(-1.96988398129978,1.,-3.62122658401893));
#56154=CARTESIAN_POINT('Ctrl Pts',(-1.96928416040877,-1.,-3.61348615496704));
#56155=CARTESIAN_POINT('Ctrl Pts',(-1.96928416040877,1.,-3.61348615496704));
#56156=CARTESIAN_POINT('Ctrl Pts',(-1.9686491188594,-1.,-3.60575714017989));
#56157=CARTESIAN_POINT('Ctrl Pts',(-1.9686491188594,1.,-3.60575714017989));
#56158=CARTESIAN_POINT('Ctrl Pts',(-1.96797854118369,-1.,-3.59803959819938));
#56159=CARTESIAN_POINT('Ctrl Pts',(-1.96797854118369,1.,-3.59803959819938));
#56160=CARTESIAN_POINT('Ctrl Pts',(-1.96727213799544,-1.,-3.59033364022801));
#56161=CARTESIAN_POINT('Ctrl Pts',(-1.96727213799544,1.,-3.59033364022801));
#56162=CARTESIAN_POINT('Ctrl Pts',(-1.96652966688911,-1.,-3.58263947663829));
#56163=CARTESIAN_POINT('Ctrl Pts',(-1.96652966688911,1.,-3.58263947663829));
#56164=CARTESIAN_POINT('Ctrl Pts',(-1.96575096652789,-1.,-3.57495748600959));
#56165=CARTESIAN_POINT('Ctrl Pts',(-1.96575096652789,1.,-3.57495748600959));
#56166=CARTESIAN_POINT('Ctrl Pts',(-1.96493594634567,-1.,-3.56728820357791));
#56167=CARTESIAN_POINT('Ctrl Pts',(-1.96493594634567,1.,-3.56728820357791));
#56168=CARTESIAN_POINT('Ctrl Pts',(-1.96408450906812,-1.,-3.55963218706096));
#56169=CARTESIAN_POINT('Ctrl Pts',(-1.96408450906812,1.,-3.55963218706096));
#56170=CARTESIAN_POINT('Ctrl Pts',(-1.96319648628644,-1.,-3.55198990600886));
#56171=CARTESIAN_POINT('Ctrl Pts',(-1.96319648628644,1.,-3.55198990600886));
#56172=CARTESIAN_POINT('Ctrl Pts',(-1.96227157573067,-1.,-3.54436163300443));
#56173=CARTESIAN_POINT('Ctrl Pts',(-1.96227157573067,1.,-3.54436163300443));
#56174=CARTESIAN_POINT('Ctrl Pts',(-1.96130926212689,-1.,-3.53674730625813));
#56175=CARTESIAN_POINT('Ctrl Pts',(-1.96130926212689,1.,-3.53674730625813));
#56176=CARTESIAN_POINT('Ctrl Pts',(-1.96030879411566,-1.,-3.52914648844351));
#56177=CARTESIAN_POINT('Ctrl Pts',(-1.96030879411566,1.,-3.52914648844351));
#56178=CARTESIAN_POINT('Ctrl Pts',(-1.95926936324461,-1.,-3.52155867431486));
#56179=CARTESIAN_POINT('Ctrl Pts',(-1.95926936324461,1.,-3.52155867431486));
#56180=CARTESIAN_POINT('Ctrl Pts',(-1.95819025316779,-1.,-3.51398354617794));
#56181=CARTESIAN_POINT('Ctrl Pts',(-1.95819025316779,1.,-3.51398354617794));
#56182=CARTESIAN_POINT('Ctrl Pts',(-1.95707099606511,-1.,-3.50642124159909));
#56183=CARTESIAN_POINT('Ctrl Pts',(-1.95707099606511,1.,-3.50642124159909));
#56184=CARTESIAN_POINT('Ctrl Pts',(-1.95591153823661,-1.,-3.49887263575583));
#56185=CARTESIAN_POINT('Ctrl Pts',(-1.95591153823661,1.,-3.49887263575583));
#56186=CARTESIAN_POINT('Ctrl Pts',(-1.95471236969643,-1.,-3.49133956289133));
#56187=CARTESIAN_POINT('Ctrl Pts',(-1.95471236969643,1.,-3.49133956289133));
#56188=CARTESIAN_POINT('Ctrl Pts',(-1.95347412486309,-1.,-3.48382414832634));
#56189=CARTESIAN_POINT('Ctrl Pts',(-1.95347412486309,1.,-3.48382414832634));
#56190=CARTESIAN_POINT('Ctrl Pts',(-1.95219722189876,-1.,-3.47632820495921));
#56191=CARTESIAN_POINT('Ctrl Pts',(-1.95219722189876,1.,-3.47632820495921));
#56192=CARTESIAN_POINT('Ctrl Pts',(-1.95088147859877,-1.,-3.46885258974191));
#56193=CARTESIAN_POINT('Ctrl Pts',(-1.95088147859877,1.,-3.46885258974191));
#56194=CARTESIAN_POINT('Ctrl Pts',(-1.94952575850197,-1.,-3.46139661060962));
#56195=CARTESIAN_POINT('Ctrl Pts',(-1.94952575850197,1.,-3.46139661060962));
#56196=CARTESIAN_POINT('Ctrl Pts',(-1.94812754766524,-1.,-3.45395731584051));
#56197=CARTESIAN_POINT('Ctrl Pts',(-1.94812754766524,1.,-3.45395731584051));
#56198=CARTESIAN_POINT('Ctrl Pts',(-1.94668377715329,-1.,-3.44653088665681));
#56199=CARTESIAN_POINT('Ctrl Pts',(-1.94668377715329,1.,-3.44653088665681));
#56200=CARTESIAN_POINT('Ctrl Pts',(-1.94519168842879,-1.,-3.43911410197687));
#56201=CARTESIAN_POINT('Ctrl Pts',(-1.94519168842879,1.,-3.43911410197687));
#56202=CARTESIAN_POINT('Ctrl Pts',(-1.94364973660284,-1.,-3.43170586602434));
#56203=CARTESIAN_POINT('Ctrl Pts',(-1.94364973660284,1.,-3.43170586602434));
#56204=CARTESIAN_POINT('Ctrl Pts',(-1.94205835913696,-1.,-3.42430850941503));
#56205=CARTESIAN_POINT('Ctrl Pts',(-1.94205835913696,1.,-3.42430850941503));
#56206=CARTESIAN_POINT('Ctrl Pts',(-1.94042111965246,-1.,-3.41692971994096));
#56207=CARTESIAN_POINT('Ctrl Pts',(-1.94042111965246,1.,-3.41692971994096));
#56208=CARTESIAN_POINT('Ctrl Pts',(-1.93874306008143,-1.,-3.40957978266642));
#56209=CARTESIAN_POINT('Ctrl Pts',(-1.93874306008143,1.,-3.40957978266642));
#56210=CARTESIAN_POINT('Ctrl Pts',(-1.93702857723098,-1.,-3.40226802104109));
#56211=CARTESIAN_POINT('Ctrl Pts',(-1.93702857723098,1.,-3.40226802104109));
#56212=CARTESIAN_POINT('Ctrl Pts',(-1.93527929945985,-1.,-3.39499923640795));
#56213=CARTESIAN_POINT('Ctrl Pts',(-1.93527929945985,1.,-3.39499923640795));
#56214=CARTESIAN_POINT('Ctrl Pts',(-1.93349233176788,-1.,-3.38777076883256));
#56215=CARTESIAN_POINT('Ctrl Pts',(-1.93349233176788,1.,-3.38777076883256));
#56216=CARTESIAN_POINT('Ctrl Pts',(-1.93165739093276,-1.,-3.3805676852555));
#56217=CARTESIAN_POINT('Ctrl Pts',(-1.93165739093276,1.,-3.3805676852555));
#56218=CARTESIAN_POINT('Ctrl Pts',(-1.92975993109877,-1.,-3.37336807068043));
#56219=CARTESIAN_POINT('Ctrl Pts',(-1.92975993109877,1.,-3.37336807068043));
#56220=CARTESIAN_POINT('Ctrl Pts',(-1.92778626543786,-1.,-3.36615168657567));
#56221=CARTESIAN_POINT('Ctrl Pts',(-1.92778626543786,1.,-3.36615168657567));
#56222=CARTESIAN_POINT('Ctrl Pts',(-1.92572846125756,-1.,-3.35890824422965));
#56223=CARTESIAN_POINT('Ctrl Pts',(-1.92572846125756,1.,-3.35890824422965));
#56224=CARTESIAN_POINT('Ctrl Pts',(-1.92358838440528,-1.,-3.35164424847223));
#56225=CARTESIAN_POINT('Ctrl Pts',(-1.92358838440528,1.,-3.35164424847223));
#56226=CARTESIAN_POINT('Ctrl Pts',(-1.92138450828404,-1.,-3.34439448941961));
#56227=CARTESIAN_POINT('Ctrl Pts',(-1.92138450828404,1.,-3.34439448941961));
#56228=CARTESIAN_POINT('Ctrl Pts',(-1.9191460961021,-1.,-3.33721230710012));
#56229=CARTESIAN_POINT('Ctrl Pts',(-1.9191460961021,1.,-3.33721230710012));
#56230=CARTESIAN_POINT('Ctrl Pts',(-1.91690081930331,-1.,-3.33014884257873));
#56231=CARTESIAN_POINT('Ctrl Pts',(-1.91690081930331,1.,-3.33014884257873));
#56232=CARTESIAN_POINT('Ctrl Pts',(-1.91466343916628,-1.,-3.32323403454535));
#56233=CARTESIAN_POINT('Ctrl Pts',(-1.91466343916628,1.,-3.32323403454535));
#56234=CARTESIAN_POINT('Ctrl Pts',(-1.91242616234442,-1.,-3.31646052426364));
#56235=CARTESIAN_POINT('Ctrl Pts',(-1.91242616234442,1.,-3.31646052426364));
#56236=CARTESIAN_POINT('Ctrl Pts',(-1.91014297830446,-1.,-3.30975721158596));
#56237=CARTESIAN_POINT('Ctrl Pts',(-1.91014297830446,1.,-3.30975721158596));
#56238=CARTESIAN_POINT('Ctrl Pts',(-1.90773912171341,-1.,-3.30300595568195));
#56239=CARTESIAN_POINT('Ctrl Pts',(-1.90773912171341,1.,-3.30300595568195));
#56240=CARTESIAN_POINT('Ctrl Pts',(-1.90513891864087,-1.,-3.29608978722113));
#56241=CARTESIAN_POINT('Ctrl Pts',(-1.90513891864087,1.,-3.29608978722113));
#56242=CARTESIAN_POINT('Ctrl Pts',(-1.90228971247527,-1.,-3.2889344860029));
#56243=CARTESIAN_POINT('Ctrl Pts',(-1.90228971247527,1.,-3.2889344860029));
#56244=CARTESIAN_POINT('Ctrl Pts',(-1.89918429230462,-1.,-3.28154737912352));
#56245=CARTESIAN_POINT('Ctrl Pts',(-1.89918429230462,1.,-3.28154737912352));
#56246=CARTESIAN_POINT('Ctrl Pts',(-1.89589172903793,-1.,-3.27407108933139));
#56247=CARTESIAN_POINT('Ctrl Pts',(-1.89589172903793,1.,-3.27407108933139));
#56248=CARTESIAN_POINT('Ctrl Pts',(-1.89255393500965,-1.,-3.26677653888676));
#56249=CARTESIAN_POINT('Ctrl Pts',(-1.89255393500965,1.,-3.26677653888676));
#56250=CARTESIAN_POINT('Ctrl Pts',(-1.88934996203698,-1.,-3.25999885193947));
#56251=CARTESIAN_POINT('Ctrl Pts',(-1.88934996203698,1.,-3.25999885193947));
#56252=CARTESIAN_POINT('Ctrl Pts',(-1.88646802523466,-1.,-3.25408686339463));
#56253=CARTESIAN_POINT('Ctrl Pts',(-1.88646802523466,1.,-3.25408686339463));
#56254=CARTESIAN_POINT('Ctrl Pts',(-1.88407708646357,-1.,-3.24935200511918));
#56255=CARTESIAN_POINT('Ctrl Pts',(-1.88407708646357,1.,-3.24935200511918));
#56256=CARTESIAN_POINT('Ctrl Pts',(-1.88229202582941,-1.,-3.24600543790443));
#56257=CARTESIAN_POINT('Ctrl Pts',(-1.88229202582941,1.,-3.24600543790443));
#56258=CARTESIAN_POINT('Ctrl Pts',(-1.88139187908074,-1.,-3.24451807186481));
#56259=CARTESIAN_POINT('Ctrl Pts',(-1.88139187908074,1.,-3.24451807186481));
#56260=CARTESIAN_POINT('Ctrl Pts',(-1.88102201872555,-1.,-3.24408699284121));
#56261=CARTESIAN_POINT('Ctrl Pts',(-1.88102201872555,1.,-3.24408699284121));
#56262=CARTESIAN_POINT('Ctrl Pts',(-1.88091100680349,-1.,-3.24410359189609));
#56263=CARTESIAN_POINT('Ctrl Pts',(-1.88091100680349,1.,-3.24410359189609));
#56264=CARTESIAN_POINT('Ctrl Pts',(-1.8808893942881,-1.,-3.24418789321065));
#56265=CARTESIAN_POINT('Ctrl Pts',(-1.8808893942881,1.,-3.24418789321065));
#56266=CARTESIAN_POINT('',(-1.97421938526992,1.,-3.70708211654725));
#56267=CARTESIAN_POINT('Ctrl Pts',(-1.97421938526992,1.,-3.70708211654725));
#56268=CARTESIAN_POINT('Ctrl Pts',(-1.97417727645308,1.,-3.70551008132332));
#56269=CARTESIAN_POINT('Ctrl Pts',(-1.97408973726715,1.,-3.70236698912904));
#56270=CARTESIAN_POINT('Ctrl Pts',(-1.97394846383216,1.,-3.6976552856004));
#56271=CARTESIAN_POINT('Ctrl Pts',(-1.97374016225483,1.,-3.69137888599902));
#56272=CARTESIAN_POINT('Ctrl Pts',(-1.97344650304519,1.,-3.68354319915092));
#56273=CARTESIAN_POINT('Ctrl Pts',(-1.97311947678517,1.,-3.67571738107084));
#56274=CARTESIAN_POINT('Ctrl Pts',(-1.97275897198678,1.,-3.66790152752075));
#56275=CARTESIAN_POINT('Ctrl Pts',(-1.9723648543905,1.,-3.6600957816636));
#56276=CARTESIAN_POINT('Ctrl Pts',(-1.9719369724024,1.,-3.652300347166));
#56277=CARTESIAN_POINT('Ctrl Pts',(-1.97147515441164,1.,-3.64451546723514));
#56278=CARTESIAN_POINT('Ctrl Pts',(-1.97097920454464,1.,-3.63674139590412));
#56279=CARTESIAN_POINT('Ctrl Pts',(-1.97044889850463,1.,-3.62897836973293));
#56280=CARTESIAN_POINT('Ctrl Pts',(-1.96988398129978,1.,-3.62122658401893));
#56281=CARTESIAN_POINT('Ctrl Pts',(-1.96928416040877,1.,-3.61348615496704));
#56282=CARTESIAN_POINT('Ctrl Pts',(-1.9686491188594,1.,-3.60575714017989));
#56283=CARTESIAN_POINT('Ctrl Pts',(-1.96797854118369,1.,-3.59803959819938));
#56284=CARTESIAN_POINT('Ctrl Pts',(-1.96727213799544,1.,-3.59033364022801));
#56285=CARTESIAN_POINT('Ctrl Pts',(-1.96652966688911,1.,-3.58263947663829));
#56286=CARTESIAN_POINT('Ctrl Pts',(-1.96575096652789,1.,-3.57495748600959));
#56287=CARTESIAN_POINT('Ctrl Pts',(-1.96493594634567,1.,-3.56728820357791));
#56288=CARTESIAN_POINT('Ctrl Pts',(-1.96408450906812,1.,-3.55963218706096));
#56289=CARTESIAN_POINT('Ctrl Pts',(-1.96319648628644,1.,-3.55198990600886));
#56290=CARTESIAN_POINT('Ctrl Pts',(-1.96227157573067,1.,-3.54436163300443));
#56291=CARTESIAN_POINT('Ctrl Pts',(-1.96130926212689,1.,-3.53674730625813));
#56292=CARTESIAN_POINT('Ctrl Pts',(-1.96030879411566,1.,-3.52914648844351));
#56293=CARTESIAN_POINT('Ctrl Pts',(-1.95926936324461,1.,-3.52155867431486));
#56294=CARTESIAN_POINT('Ctrl Pts',(-1.95819025316779,1.,-3.51398354617794));
#56295=CARTESIAN_POINT('Ctrl Pts',(-1.95707099606511,1.,-3.50642124159909));
#56296=CARTESIAN_POINT('Ctrl Pts',(-1.95591153823661,1.,-3.49887263575583));
#56297=CARTESIAN_POINT('Ctrl Pts',(-1.95471236969643,1.,-3.49133956289133));
#56298=CARTESIAN_POINT('Ctrl Pts',(-1.95347412486309,1.,-3.48382414832634));
#56299=CARTESIAN_POINT('Ctrl Pts',(-1.95219722189876,1.,-3.47632820495921));
#56300=CARTESIAN_POINT('Ctrl Pts',(-1.95088147859877,1.,-3.46885258974191));
#56301=CARTESIAN_POINT('Ctrl Pts',(-1.94952575850197,1.,-3.46139661060962));
#56302=CARTESIAN_POINT('Ctrl Pts',(-1.94812754766524,1.,-3.45395731584051));
#56303=CARTESIAN_POINT('Ctrl Pts',(-1.94668377715329,1.,-3.44653088665681));
#56304=CARTESIAN_POINT('Ctrl Pts',(-1.94519168842879,1.,-3.43911410197687));
#56305=CARTESIAN_POINT('Ctrl Pts',(-1.94364973660284,1.,-3.43170586602434));
#56306=CARTESIAN_POINT('Ctrl Pts',(-1.94205835913696,1.,-3.42430850941503));
#56307=CARTESIAN_POINT('Ctrl Pts',(-1.94042111965246,1.,-3.41692971994096));
#56308=CARTESIAN_POINT('Ctrl Pts',(-1.93874306008143,1.,-3.40957978266642));
#56309=CARTESIAN_POINT('Ctrl Pts',(-1.93702857723098,1.,-3.40226802104109));
#56310=CARTESIAN_POINT('Ctrl Pts',(-1.93527929945985,1.,-3.39499923640795));
#56311=CARTESIAN_POINT('Ctrl Pts',(-1.93349233176788,1.,-3.38777076883256));
#56312=CARTESIAN_POINT('Ctrl Pts',(-1.93165739093276,1.,-3.3805676852555));
#56313=CARTESIAN_POINT('Ctrl Pts',(-1.92975993109877,1.,-3.37336807068043));
#56314=CARTESIAN_POINT('Ctrl Pts',(-1.92778626543786,1.,-3.36615168657567));
#56315=CARTESIAN_POINT('Ctrl Pts',(-1.92572846125756,1.,-3.35890824422965));
#56316=CARTESIAN_POINT('Ctrl Pts',(-1.92358838440528,1.,-3.35164424847223));
#56317=CARTESIAN_POINT('Ctrl Pts',(-1.92138450828404,1.,-3.34439448941961));
#56318=CARTESIAN_POINT('Ctrl Pts',(-1.9191460961021,1.,-3.33721230710012));
#56319=CARTESIAN_POINT('Ctrl Pts',(-1.91690081930331,1.,-3.33014884257873));
#56320=CARTESIAN_POINT('Ctrl Pts',(-1.91466343916628,1.,-3.32323403454535));
#56321=CARTESIAN_POINT('Ctrl Pts',(-1.91242616234442,1.,-3.31646052426364));
#56322=CARTESIAN_POINT('Ctrl Pts',(-1.91014297830446,1.,-3.30975721158596));
#56323=CARTESIAN_POINT('Ctrl Pts',(-1.90773912171341,1.,-3.30300595568195));
#56324=CARTESIAN_POINT('Ctrl Pts',(-1.90513891864087,1.,-3.29608978722113));
#56325=CARTESIAN_POINT('Ctrl Pts',(-1.90228971247527,1.,-3.2889344860029));
#56326=CARTESIAN_POINT('Ctrl Pts',(-1.89918429230462,1.,-3.28154737912352));
#56327=CARTESIAN_POINT('Ctrl Pts',(-1.89589172903793,1.,-3.27407108933139));
#56328=CARTESIAN_POINT('Ctrl Pts',(-1.89255393500965,1.,-3.26677653888676));
#56329=CARTESIAN_POINT('Ctrl Pts',(-1.88934996203698,1.,-3.25999885193947));
#56330=CARTESIAN_POINT('Ctrl Pts',(-1.88646802523466,1.,-3.25408686339463));
#56331=CARTESIAN_POINT('Ctrl Pts',(-1.88407708646357,1.,-3.24935200511918));
#56332=CARTESIAN_POINT('Ctrl Pts',(-1.88242596600454,1.,-3.2462565441079));
#56333=CARTESIAN_POINT('Ctrl Pts',(-1.88156537699203,1.,-3.24480754676064));
#56334=CARTESIAN_POINT('Ctrl Pts',(-1.88117508446775,1.,-3.24428080353022));
#56335=CARTESIAN_POINT('Ctrl Pts',(-1.8810229239812,1.,-3.24415531671284));
#56336=CARTESIAN_POINT('Ctrl Pts',(-1.88097764062697,1.,-3.24413672884812));
#56337=CARTESIAN_POINT('',(-1.97421938526992,0.,-3.70708211654725));
#56338=CARTESIAN_POINT('Ctrl Pts',(-1.519044091397,-1.,-3.42855728381368));
#56339=CARTESIAN_POINT('Ctrl Pts',(-1.519044091397,1.,-3.42855728381368));
#56340=CARTESIAN_POINT('Ctrl Pts',(-1.51896318668366,-1.,-3.42852521763778));
#56341=CARTESIAN_POINT('Ctrl Pts',(-1.51896318668366,1.,-3.42852521763778));
#56342=CARTESIAN_POINT('Ctrl Pts',(-1.51888450659652,-1.,-3.42860527149177));
#56343=CARTESIAN_POINT('Ctrl Pts',(-1.51888450659652,1.,-3.42860527149177));
#56344=CARTESIAN_POINT('Ctrl Pts',(-1.51901585839109,-1.,-3.42915787669893));
#56345=CARTESIAN_POINT('Ctrl Pts',(-1.51901585839109,1.,-3.42915787669893));
#56346=CARTESIAN_POINT('Ctrl Pts',(-1.51969006980999,-1.,-3.43076036253837));
#56347=CARTESIAN_POINT('Ctrl Pts',(-1.51969006980999,1.,-3.43076036253837));
#56348=CARTESIAN_POINT('Ctrl Pts',(-1.52134826724293,-1.,-3.43417156977893));
#56349=CARTESIAN_POINT('Ctrl Pts',(-1.52134826724293,1.,-3.43417156977893));
#56350=CARTESIAN_POINT('Ctrl Pts',(-1.5237734895035,-1.,-3.4388889597401));
#56351=CARTESIAN_POINT('Ctrl Pts',(-1.5237734895035,1.,-3.4388889597401));
#56352=CARTESIAN_POINT('Ctrl Pts',(-1.52686242875556,-1.,-3.44469547526647));
#56353=CARTESIAN_POINT('Ctrl Pts',(-1.52686242875556,1.,-3.44469547526647));
#56354=CARTESIAN_POINT('Ctrl Pts',(-1.53046244461635,-1.,-3.45127136828305));
#56355=CARTESIAN_POINT('Ctrl Pts',(-1.53046244461635,1.,-3.45127136828305));
#56356=CARTESIAN_POINT('Ctrl Pts',(-1.53440195378792,-1.,-3.45825932955032));
#56357=CARTESIAN_POINT('Ctrl Pts',(-1.53440195378792,1.,-3.45825932955032));
#56358=CARTESIAN_POINT('Ctrl Pts',(-1.53851507915502,-1.,-3.46531752207153));
#56359=CARTESIAN_POINT('Ctrl Pts',(-1.53851507915502,1.,-3.46531752207153));
#56360=CARTESIAN_POINT('Ctrl Pts',(-1.54266605398187,-1.,-3.47217189224653));
#56361=CARTESIAN_POINT('Ctrl Pts',(-1.54266605398187,1.,-3.47217189224653));
#56362=CARTESIAN_POINT('Ctrl Pts',(-1.54678009290276,-1.,-3.47868272898751));
#56363=CARTESIAN_POINT('Ctrl Pts',(-1.54678009290276,1.,-3.47868272898751));
#56364=CARTESIAN_POINT('Ctrl Pts',(-1.55084702970452,-1.,-3.48485155928567));
#56365=CARTESIAN_POINT('Ctrl Pts',(-1.55084702970452,1.,-3.48485155928567));
#56366=CARTESIAN_POINT('Ctrl Pts',(-1.55489595901116,-1.,-3.4907646087742));
#56367=CARTESIAN_POINT('Ctrl Pts',(-1.55489595901116,1.,-3.4907646087742));
#56368=CARTESIAN_POINT('Ctrl Pts',(-1.55897703097874,-1.,-3.49655185179655));
#56369=CARTESIAN_POINT('Ctrl Pts',(-1.55897703097874,1.,-3.49655185179655));
#56370=CARTESIAN_POINT('Ctrl Pts',(-1.56314187758675,-1.,-3.50234321621578));
#56371=CARTESIAN_POINT('Ctrl Pts',(-1.56314187758675,1.,-3.50234321621578));
#56372=CARTESIAN_POINT('Ctrl Pts',(-1.56742097575012,-1.,-3.50821771695363));
#56373=CARTESIAN_POINT('Ctrl Pts',(-1.56742097575012,1.,-3.50821771695363));
#56374=CARTESIAN_POINT('Ctrl Pts',(-1.57181569799743,-1.,-3.51418598431665));
#56375=CARTESIAN_POINT('Ctrl Pts',(-1.57181569799743,1.,-3.51418598431665));
#56376=CARTESIAN_POINT('Ctrl Pts',(-1.57631049988158,-1.,-3.52021847865912));
#56377=CARTESIAN_POINT('Ctrl Pts',(-1.57631049988158,1.,-3.52021847865912));
#56378=CARTESIAN_POINT('Ctrl Pts',(-1.58088027227848,-1.,-3.52626275334881));
#56379=CARTESIAN_POINT('Ctrl Pts',(-1.58088027227848,1.,-3.52626275334881));
#56380=CARTESIAN_POINT('Ctrl Pts',(-1.58549906268088,-1.,-3.5322637814708));
#56381=CARTESIAN_POINT('Ctrl Pts',(-1.58549906268088,1.,-3.5322637814708));
#56382=CARTESIAN_POINT('Ctrl Pts',(-1.59014958368739,-1.,-3.53818616861077));
#56383=CARTESIAN_POINT('Ctrl Pts',(-1.59014958368739,1.,-3.53818616861077));
#56384=CARTESIAN_POINT('Ctrl Pts',(-1.59482766949766,-1.,-3.54402458182337));
#56385=CARTESIAN_POINT('Ctrl Pts',(-1.59482766949766,1.,-3.54402458182337));
#56386=CARTESIAN_POINT('Ctrl Pts',(-1.59953698113457,-1.,-3.54979148634454));
#56387=CARTESIAN_POINT('Ctrl Pts',(-1.59953698113457,1.,-3.54979148634454));
#56388=CARTESIAN_POINT('Ctrl Pts',(-1.60428584699853,-1.,-3.55550985096129));
#56389=CARTESIAN_POINT('Ctrl Pts',(-1.60428584699853,1.,-3.55550985096129));
#56390=CARTESIAN_POINT('Ctrl Pts',(-1.60908344685457,-1.,-3.5612043248298));
#56391=CARTESIAN_POINT('Ctrl Pts',(-1.60908344685457,1.,-3.5612043248298));
#56392=CARTESIAN_POINT('Ctrl Pts',(-1.61393581747514,-1.,-3.56689200468387));
#56393=CARTESIAN_POINT('Ctrl Pts',(-1.61393581747514,1.,-3.56689200468387));
#56394=CARTESIAN_POINT('Ctrl Pts',(-1.61884340915404,-1.,-3.57257679609806));
#56395=CARTESIAN_POINT('Ctrl Pts',(-1.61884340915404,1.,-3.57257679609806));
#56396=CARTESIAN_POINT('Ctrl Pts',(-1.62380329464844,-1.,-3.5782545595439));
#56397=CARTESIAN_POINT('Ctrl Pts',(-1.62380329464844,1.,-3.5782545595439));
#56398=CARTESIAN_POINT('Ctrl Pts',(-1.62881051550745,-1.,-3.58391625774343));
#56399=CARTESIAN_POINT('Ctrl Pts',(-1.62881051550745,1.,-3.58391625774343));
#56400=CARTESIAN_POINT('Ctrl Pts',(-1.6338597145126,-1.,-3.58955176627879));
#56401=CARTESIAN_POINT('Ctrl Pts',(-1.6338597145126,1.,-3.58955176627879));
#56402=CARTESIAN_POINT('Ctrl Pts',(-1.63894676675352,-1.,-3.59515368334893));
#56403=CARTESIAN_POINT('Ctrl Pts',(-1.63894676675352,1.,-3.59515368334893));
#56404=CARTESIAN_POINT('Ctrl Pts',(-1.64407004385582,-1.,-3.60072028513845));
#56405=CARTESIAN_POINT('Ctrl Pts',(-1.64407004385582,1.,-3.60072028513845));
#56406=CARTESIAN_POINT('Ctrl Pts',(-1.64922952425832,-1.,-3.60625346556992));
#56407=CARTESIAN_POINT('Ctrl Pts',(-1.64922952425832,1.,-3.60625346556992));
#56408=CARTESIAN_POINT('Ctrl Pts',(-1.65442619244325,-1.,-3.61175734965127));
#56409=CARTESIAN_POINT('Ctrl Pts',(-1.65442619244325,1.,-3.61175734965127));
#56410=CARTESIAN_POINT('Ctrl Pts',(-1.65966133399186,-1.,-3.61723666482456));
#56411=CARTESIAN_POINT('Ctrl Pts',(-1.65966133399186,1.,-3.61723666482456));
#56412=CARTESIAN_POINT('Ctrl Pts',(-1.66493585923855,-1.,-3.62269517989109));
#56413=CARTESIAN_POINT('Ctrl Pts',(-1.66493585923855,1.,-3.62269517989109));
#56414=CARTESIAN_POINT('Ctrl Pts',(-1.67024966008045,-1.,-3.62813422105271));
#56415=CARTESIAN_POINT('Ctrl Pts',(-1.67024966008045,1.,-3.62813422105271));
#56416=CARTESIAN_POINT('Ctrl Pts',(-1.67560193613156,-1.,-3.63355343201232));
#56417=CARTESIAN_POINT('Ctrl Pts',(-1.67560193613156,1.,-3.63355343201232));
#56418=CARTESIAN_POINT('Ctrl Pts',(-1.68099146651586,-1.,-3.63895140887462));
#56419=CARTESIAN_POINT('Ctrl Pts',(-1.68099146651586,1.,-3.63895140887462));
#56420=CARTESIAN_POINT('Ctrl Pts',(-1.68641690471457,-1.,-3.64432638915203));
#56421=CARTESIAN_POINT('Ctrl Pts',(-1.68641690471457,1.,-3.64432638915203));
#56422=CARTESIAN_POINT('Ctrl Pts',(-1.69187705481689,-1.,-3.64967689827371));
#56423=CARTESIAN_POINT('Ctrl Pts',(-1.69187705481689,1.,-3.64967689827371));
#56424=CARTESIAN_POINT('Ctrl Pts',(-1.69737117722534,-1.,-3.65500246526749));
#56425=CARTESIAN_POINT('Ctrl Pts',(-1.69737117722534,1.,-3.65500246526749));
#56426=CARTESIAN_POINT('Ctrl Pts',(-1.70289888566873,-1.,-3.66030338774847));
#56427=CARTESIAN_POINT('Ctrl Pts',(-1.70289888566873,1.,-3.66030338774847));
#56428=CARTESIAN_POINT('Ctrl Pts',(-1.70846001610956,-1.,-3.66558043198876));
#56429=CARTESIAN_POINT('Ctrl Pts',(-1.70846001610956,1.,-3.66558043198876));
#56430=CARTESIAN_POINT('Ctrl Pts',(-1.71405450210384,-1.,-3.67083454901611));
#56431=CARTESIAN_POINT('Ctrl Pts',(-1.71405450210384,1.,-3.67083454901611));
#56432=CARTESIAN_POINT('Ctrl Pts',(-1.71968225581808,-1.,-3.67606660374709));
#56433=CARTESIAN_POINT('Ctrl Pts',(-1.71968225581808,1.,-3.67606660374709));
#56434=CARTESIAN_POINT('Ctrl Pts',(-1.72534302437056,-1.,-3.68127704936579));
#56435=CARTESIAN_POINT('Ctrl Pts',(-1.72534302437056,1.,-3.68127704936579));
#56436=CARTESIAN_POINT('Ctrl Pts',(-1.73103640956717,-1.,-3.68646597019332));
#56437=CARTESIAN_POINT('Ctrl Pts',(-1.73103640956717,1.,-3.68646597019332));
#56438=CARTESIAN_POINT('Ctrl Pts',(-1.73676193254557,-1.,-3.69163322648036));
#56439=CARTESIAN_POINT('Ctrl Pts',(-1.73676193254557,1.,-3.69163322648036));
#56440=CARTESIAN_POINT('Ctrl Pts',(-1.74251908492617,-1.,-3.69677856910517));
#56441=CARTESIAN_POINT('Ctrl Pts',(-1.74251908492617,1.,-3.69677856910517));
#56442=CARTESIAN_POINT('Ctrl Pts',(-1.74830738046057,-1.,-3.7019017567335));
#56443=CARTESIAN_POINT('Ctrl Pts',(-1.74830738046057,1.,-3.7019017567335));
#56444=CARTESIAN_POINT('Ctrl Pts',(-1.75412641804042,-1.,-3.70700269736659));
#56445=CARTESIAN_POINT('Ctrl Pts',(-1.75412641804042,1.,-3.70700269736659));
#56446=CARTESIAN_POINT('Ctrl Pts',(-1.75997588498865,-1.,-3.71208146346136));
#56447=CARTESIAN_POINT('Ctrl Pts',(-1.75997588498865,1.,-3.71208146346136));
#56448=CARTESIAN_POINT('Ctrl Pts',(-1.76585552124394,-1.,-3.71713822377359));
#56449=CARTESIAN_POINT('Ctrl Pts',(-1.76585552124394,1.,-3.71713822377359));
#56450=CARTESIAN_POINT('Ctrl Pts',(-1.77176509401761,-1.,-3.72217319911254));
#56451=CARTESIAN_POINT('Ctrl Pts',(-1.77176509401761,1.,-3.72217319911254));
#56452=CARTESIAN_POINT('Ctrl Pts',(-1.77770437039658,-1.,-3.72718661205609));
#56453=CARTESIAN_POINT('Ctrl Pts',(-1.77770437039658,1.,-3.72718661205609));
#56454=CARTESIAN_POINT('Ctrl Pts',(-1.78367308442901,-1.,-3.7321786309547));
#56455=CARTESIAN_POINT('Ctrl Pts',(-1.78367308442901,1.,-3.7321786309547));
#56456=CARTESIAN_POINT('Ctrl Pts',(-1.78967092823491,-1.,-3.73714934730681));
#56457=CARTESIAN_POINT('Ctrl Pts',(-1.78967092823491,1.,-3.73714934730681));
#56458=CARTESIAN_POINT('Ctrl Pts',(-1.79569757859422,-1.,-3.74209880352445));
#56459=CARTESIAN_POINT('Ctrl Pts',(-1.79569757859422,1.,-3.74209880352445));
#56460=CARTESIAN_POINT('Ctrl Pts',(-1.8017527148577,-1.,-3.74702700875467));
#56461=CARTESIAN_POINT('Ctrl Pts',(-1.8017527148577,1.,-3.74702700875467));
#56462=CARTESIAN_POINT('Ctrl Pts',(-1.80783603939617,-1.,-3.75193395887977));
#56463=CARTESIAN_POINT('Ctrl Pts',(-1.80783603939617,1.,-3.75193395887977));
#56464=CARTESIAN_POINT('Ctrl Pts',(-1.8139472983358,-1.,-3.75681965683071));
#56465=CARTESIAN_POINT('Ctrl Pts',(-1.8139472983358,1.,-3.75681965683071));
#56466=CARTESIAN_POINT('Ctrl Pts',(-1.82008629694091,-1.,-3.76168412707948));
#56467=CARTESIAN_POINT('Ctrl Pts',(-1.82008629694091,1.,-3.76168412707948));
#56468=CARTESIAN_POINT('Ctrl Pts',(-1.82625289220915,-1.,-3.76652740353775));
#56469=CARTESIAN_POINT('Ctrl Pts',(-1.82625289220915,1.,-3.76652740353775));
#56470=CARTESIAN_POINT('Ctrl Pts',(-1.83120816955645,-1.,-3.77038509817999));
#56471=CARTESIAN_POINT('Ctrl Pts',(-1.83120816955645,1.,-3.77038509817999));
#56472=CARTESIAN_POINT('Ctrl Pts',(-1.83493697934534,-1.,-3.77326886064398));
#56473=CARTESIAN_POINT('Ctrl Pts',(-1.83493697934534,1.,-3.77326886064398));
#56474=CARTESIAN_POINT('Ctrl Pts',(-1.83742834010626,-1.,-3.77518714457833));
#56475=CARTESIAN_POINT('Ctrl Pts',(-1.83742834010626,1.,-3.77518714457833));
#56476=CARTESIAN_POINT('Ctrl Pts',(-1.83867539237861,-1.,-3.77614523045147));
#56477=CARTESIAN_POINT('Ctrl Pts',(-1.83867539237861,1.,-3.77614523045147));
#56478=CARTESIAN_POINT('',(-1.5189508286633,1.,-3.42859860294306));
#56479=CARTESIAN_POINT('Ctrl Pts',(-1.5189508286633,-1.,-3.42859860294306));
#56480=CARTESIAN_POINT('Ctrl Pts',(-1.5189508286633,-0.666666666666667,
-3.42859860294306));
#56481=CARTESIAN_POINT('Ctrl Pts',(-1.5189508286633,-0.333333333333333,
-3.42859860294306));
#56482=CARTESIAN_POINT('Ctrl Pts',(-1.5189508286633,0.333333333333333,-3.42859860294306));
#56483=CARTESIAN_POINT('Ctrl Pts',(-1.5189508286633,0.666666666666667,-3.42859860294305));
#56484=CARTESIAN_POINT('Ctrl Pts',(-1.5189508286633,1.,-3.42859860294305));
#56485=CARTESIAN_POINT('',(-1.83867539237861,1.,-3.77614523045147));
#56486=CARTESIAN_POINT('',(-1.83867539237861,0.,-3.77614523045147));
#56487=CARTESIAN_POINT('Ctrl Pts',(-1.5189508286633,1.,-3.42859860294306));
#56488=CARTESIAN_POINT('Ctrl Pts',(-1.51893924967331,1.,-3.42864616361875));
#56489=CARTESIAN_POINT('Ctrl Pts',(-1.5189513329503,1.,-3.42884302333841));
#56490=CARTESIAN_POINT('Ctrl Pts',(-1.51914806898491,1.,-3.42946838852588));
#56491=CARTESIAN_POINT('Ctrl Pts',(-1.5198144909338,1.,-3.43101631893414));
#56492=CARTESIAN_POINT('Ctrl Pts',(-1.52134826724293,1.,-3.43417156977893));
#56493=CARTESIAN_POINT('Ctrl Pts',(-1.5237734895035,1.,-3.4388889597401));
#56494=CARTESIAN_POINT('Ctrl Pts',(-1.52686242875556,1.,-3.44469547526647));
#56495=CARTESIAN_POINT('Ctrl Pts',(-1.53046244461635,1.,-3.45127136828305));
#56496=CARTESIAN_POINT('Ctrl Pts',(-1.53440195378792,1.,-3.45825932955032));
#56497=CARTESIAN_POINT('Ctrl Pts',(-1.53851507915502,1.,-3.46531752207153));
#56498=CARTESIAN_POINT('Ctrl Pts',(-1.54266605398187,1.,-3.47217189224653));
#56499=CARTESIAN_POINT('Ctrl Pts',(-1.54678009290276,1.,-3.47868272898751));
#56500=CARTESIAN_POINT('Ctrl Pts',(-1.55084702970452,1.,-3.48485155928567));
#56501=CARTESIAN_POINT('Ctrl Pts',(-1.55489595901116,1.,-3.4907646087742));
#56502=CARTESIAN_POINT('Ctrl Pts',(-1.55897703097874,1.,-3.49655185179655));
#56503=CARTESIAN_POINT('Ctrl Pts',(-1.56314187758675,1.,-3.50234321621578));
#56504=CARTESIAN_POINT('Ctrl Pts',(-1.56742097575012,1.,-3.50821771695363));
#56505=CARTESIAN_POINT('Ctrl Pts',(-1.57181569799743,1.,-3.51418598431665));
#56506=CARTESIAN_POINT('Ctrl Pts',(-1.57631049988158,1.,-3.52021847865912));
#56507=CARTESIAN_POINT('Ctrl Pts',(-1.58088027227848,1.,-3.52626275334881));
#56508=CARTESIAN_POINT('Ctrl Pts',(-1.58549906268088,1.,-3.5322637814708));
#56509=CARTESIAN_POINT('Ctrl Pts',(-1.59014958368739,1.,-3.53818616861077));
#56510=CARTESIAN_POINT('Ctrl Pts',(-1.59482766949766,1.,-3.54402458182337));
#56511=CARTESIAN_POINT('Ctrl Pts',(-1.59953698113457,1.,-3.54979148634454));
#56512=CARTESIAN_POINT('Ctrl Pts',(-1.60428584699853,1.,-3.55550985096129));
#56513=CARTESIAN_POINT('Ctrl Pts',(-1.60908344685457,1.,-3.5612043248298));
#56514=CARTESIAN_POINT('Ctrl Pts',(-1.61393581747514,1.,-3.56689200468387));
#56515=CARTESIAN_POINT('Ctrl Pts',(-1.61884340915404,1.,-3.57257679609806));
#56516=CARTESIAN_POINT('Ctrl Pts',(-1.62380329464844,1.,-3.5782545595439));
#56517=CARTESIAN_POINT('Ctrl Pts',(-1.62881051550745,1.,-3.58391625774343));
#56518=CARTESIAN_POINT('Ctrl Pts',(-1.6338597145126,1.,-3.58955176627879));
#56519=CARTESIAN_POINT('Ctrl Pts',(-1.63894676675352,1.,-3.59515368334893));
#56520=CARTESIAN_POINT('Ctrl Pts',(-1.64407004385582,1.,-3.60072028513845));
#56521=CARTESIAN_POINT('Ctrl Pts',(-1.64922952425832,1.,-3.60625346556992));
#56522=CARTESIAN_POINT('Ctrl Pts',(-1.65442619244325,1.,-3.61175734965127));
#56523=CARTESIAN_POINT('Ctrl Pts',(-1.65966133399186,1.,-3.61723666482456));
#56524=CARTESIAN_POINT('Ctrl Pts',(-1.66493585923855,1.,-3.62269517989109));
#56525=CARTESIAN_POINT('Ctrl Pts',(-1.67024966008045,1.,-3.62813422105271));
#56526=CARTESIAN_POINT('Ctrl Pts',(-1.67560193613156,1.,-3.63355343201232));
#56527=CARTESIAN_POINT('Ctrl Pts',(-1.68099146651586,1.,-3.63895140887462));
#56528=CARTESIAN_POINT('Ctrl Pts',(-1.68641690471457,1.,-3.64432638915203));
#56529=CARTESIAN_POINT('Ctrl Pts',(-1.69187705481689,1.,-3.64967689827371));
#56530=CARTESIAN_POINT('Ctrl Pts',(-1.69737117722534,1.,-3.65500246526749));
#56531=CARTESIAN_POINT('Ctrl Pts',(-1.70289888566873,1.,-3.66030338774847));
#56532=CARTESIAN_POINT('Ctrl Pts',(-1.70846001610956,1.,-3.66558043198876));
#56533=CARTESIAN_POINT('Ctrl Pts',(-1.71405450210384,1.,-3.67083454901611));
#56534=CARTESIAN_POINT('Ctrl Pts',(-1.71968225581808,1.,-3.67606660374709));
#56535=CARTESIAN_POINT('Ctrl Pts',(-1.72534302437056,1.,-3.68127704936579));
#56536=CARTESIAN_POINT('Ctrl Pts',(-1.73103640956717,1.,-3.68646597019332));
#56537=CARTESIAN_POINT('Ctrl Pts',(-1.73676193254557,1.,-3.69163322648036));
#56538=CARTESIAN_POINT('Ctrl Pts',(-1.74251908492617,1.,-3.69677856910517));
#56539=CARTESIAN_POINT('Ctrl Pts',(-1.74830738046057,1.,-3.7019017567335));
#56540=CARTESIAN_POINT('Ctrl Pts',(-1.75412641804042,1.,-3.70700269736659));
#56541=CARTESIAN_POINT('Ctrl Pts',(-1.75997588498865,1.,-3.71208146346136));
#56542=CARTESIAN_POINT('Ctrl Pts',(-1.76585552124394,1.,-3.71713822377359));
#56543=CARTESIAN_POINT('Ctrl Pts',(-1.77176509401761,1.,-3.72217319911254));
#56544=CARTESIAN_POINT('Ctrl Pts',(-1.77770437039658,1.,-3.72718661205609));
#56545=CARTESIAN_POINT('Ctrl Pts',(-1.78367308442901,1.,-3.7321786309547));
#56546=CARTESIAN_POINT('Ctrl Pts',(-1.78967092823491,1.,-3.73714934730681));
#56547=CARTESIAN_POINT('Ctrl Pts',(-1.79569757859422,1.,-3.74209880352445));
#56548=CARTESIAN_POINT('Ctrl Pts',(-1.8017527148577,1.,-3.74702700875467));
#56549=CARTESIAN_POINT('Ctrl Pts',(-1.80783603939617,1.,-3.75193395887977));
#56550=CARTESIAN_POINT('Ctrl Pts',(-1.8139472983358,1.,-3.75681965683071));
#56551=CARTESIAN_POINT('Ctrl Pts',(-1.82008629694091,1.,-3.76168412707948));
#56552=CARTESIAN_POINT('Ctrl Pts',(-1.82625289220915,1.,-3.76652740353775));
#56553=CARTESIAN_POINT('Ctrl Pts',(-1.83120816955645,1.,-3.77038509817999));
#56554=CARTESIAN_POINT('Ctrl Pts',(-1.83493697934534,1.,-3.77326886064398));
#56555=CARTESIAN_POINT('Ctrl Pts',(-1.83742834010626,1.,-3.77518714457833));
#56556=CARTESIAN_POINT('Ctrl Pts',(-1.83867539237861,1.,-3.77614523045147));
#56557=CARTESIAN_POINT('Origin',(-1.83867539237861,0.,-3.77614523045147));
#56558=CARTESIAN_POINT('',(-1.97421938526992,1.,-3.70708211654725));
#56559=CARTESIAN_POINT('Origin',(0.,0.,0.));
#56560=CARTESIAN_POINT('',(-1.35032489087269,1.,-3.49844575334386));
#56561=CARTESIAN_POINT('Origin',(0.,1.,0.));
#56562=CARTESIAN_POINT('Ctrl Pts',(-1.35032489087269,1.,-3.49844575334386));
#56563=CARTESIAN_POINT('Ctrl Pts',(-1.35032489087269,0.666666666666667,
-3.49844575334386));
#56564=CARTESIAN_POINT('Ctrl Pts',(-1.35032489087269,0.333333333333333,
-3.49844575334386));
#56565=CARTESIAN_POINT('Ctrl Pts',(-1.35032489087269,-0.333333333333333,
-3.49844575334386));
#56566=CARTESIAN_POINT('Ctrl Pts',(-1.35032489087269,-0.666666666666667,
-3.49844575334386));
#56567=CARTESIAN_POINT('Ctrl Pts',(-1.35032489087269,-1.,-3.49844575334386));
#56568=CARTESIAN_POINT('Ctrl Pts',(-1.36999806084572,-1.,-3.97027773754922));
#56569=CARTESIAN_POINT('Ctrl Pts',(-1.36999806084572,1.,-3.97027773754922));
#56570=CARTESIAN_POINT('Ctrl Pts',(-1.37020239094758,-1.,-3.9687184694173));
#56571=CARTESIAN_POINT('Ctrl Pts',(-1.37020239094758,1.,-3.9687184694173));
#56572=CARTESIAN_POINT('Ctrl Pts',(-1.37060761746027,-1.,-3.96560037975788));
#56573=CARTESIAN_POINT('Ctrl Pts',(-1.37060761746027,1.,-3.96560037975788));
#56574=CARTESIAN_POINT('Ctrl Pts',(-1.37120515615663,-1.,-3.96092458508407));
#56575=CARTESIAN_POINT('Ctrl Pts',(-1.37120515615663,1.,-3.96092458508407));
#56576=CARTESIAN_POINT('Ctrl Pts',(-1.37198126433139,-1.,-3.95469287283105));
#56577=CARTESIAN_POINT('Ctrl Pts',(-1.37198126433139,1.,-3.95469287283105));
#56578=CARTESIAN_POINT('Ctrl Pts',(-1.37291699203423,-1.,-3.94690771786926));
#56579=CARTESIAN_POINT('Ctrl Pts',(-1.37291699203423,1.,-3.94690771786926));
#56580=CARTESIAN_POINT('Ctrl Pts',(-1.37381821967499,-1.,-3.93912709041791));
#56581=CARTESIAN_POINT('Ctrl Pts',(-1.37381821967499,1.,-3.93912709041791));
#56582=CARTESIAN_POINT('Ctrl Pts',(-1.37468482215784,-1.,-3.93135106761941));
#56583=CARTESIAN_POINT('Ctrl Pts',(-1.37468482215784,1.,-3.93135106761941));
#56584=CARTESIAN_POINT('Ctrl Pts',(-1.37551664448057,-1.,-3.92357976987132));
#56585=CARTESIAN_POINT('Ctrl Pts',(-1.37551664448057,1.,-3.92357976987132));
#56586=CARTESIAN_POINT('Ctrl Pts',(-1.37631350505516,-1.,-3.91581337461825));
#56587=CARTESIAN_POINT('Ctrl Pts',(-1.37631350505516,1.,-3.91581337461825));
#56588=CARTESIAN_POINT('Ctrl Pts',(-1.3770751963376,-1.,-3.90805209522729));
#56589=CARTESIAN_POINT('Ctrl Pts',(-1.3770751963376,1.,-3.90805209522729));
#56590=CARTESIAN_POINT('Ctrl Pts',(-1.3778014851263,-1.,-3.90029615196255));
#56591=CARTESIAN_POINT('Ctrl Pts',(-1.3778014851263,1.,-3.90029615196255));
#56592=CARTESIAN_POINT('Ctrl Pts',(-1.37849211287981,-1.,-3.89254574338385));
#56593=CARTESIAN_POINT('Ctrl Pts',(-1.37849211287981,1.,-3.89254574338385));
#56594=CARTESIAN_POINT('Ctrl Pts',(-1.37914679719446,-1.,-3.88480102249461));
#56595=CARTESIAN_POINT('Ctrl Pts',(-1.37914679719446,1.,-3.88480102249461));
#56596=CARTESIAN_POINT('Ctrl Pts',(-1.37976523097187,-1.,-3.87706205830865));
#56597=CARTESIAN_POINT('Ctrl Pts',(-1.37976523097187,1.,-3.87706205830865));
#56598=CARTESIAN_POINT('Ctrl Pts',(-1.38034709213129,-1.,-3.86932885813403));
#56599=CARTESIAN_POINT('Ctrl Pts',(-1.38034709213129,1.,-3.86932885813403));
#56600=CARTESIAN_POINT('Ctrl Pts',(-1.38089205993067,-1.,-3.86160143044187));
#56601=CARTESIAN_POINT('Ctrl Pts',(-1.38089205993067,1.,-3.86160143044187));
#56602=CARTESIAN_POINT('Ctrl Pts',(-1.38139983115075,-1.,-3.85387983979557));
#56603=CARTESIAN_POINT('Ctrl Pts',(-1.38139983115075,1.,-3.85387983979557));
#56604=CARTESIAN_POINT('Ctrl Pts',(-1.38187013346089,-1.,-3.84616425605705));
#56605=CARTESIAN_POINT('Ctrl Pts',(-1.38187013346089,1.,-3.84616425605705));
#56606=CARTESIAN_POINT('Ctrl Pts',(-1.38230274828774,-1.,-3.83845502790609));
#56607=CARTESIAN_POINT('Ctrl Pts',(-1.38230274828774,1.,-3.83845502790609));
#56608=CARTESIAN_POINT('Ctrl Pts',(-1.38269750245086,-1.,-3.83075266982138));
#56609=CARTESIAN_POINT('Ctrl Pts',(-1.38269750245086,1.,-3.83075266982138));
#56610=CARTESIAN_POINT('Ctrl Pts',(-1.38305421262724,-1.,-3.82305771743715));
#56611=CARTESIAN_POINT('Ctrl Pts',(-1.38305421262724,1.,-3.82305771743715));
#56612=CARTESIAN_POINT('Ctrl Pts',(-1.38337263902766,-1.,-3.81537060817765));
#56613=CARTESIAN_POINT('Ctrl Pts',(-1.38337263902766,1.,-3.81537060817765));
#56614=CARTESIAN_POINT('Ctrl Pts',(-1.38365244046226,-1.,-3.80769156398429));
#56615=CARTESIAN_POINT('Ctrl Pts',(-1.38365244046226,1.,-3.80769156398429));
#56616=CARTESIAN_POINT('Ctrl Pts',(-1.38389311766701,-1.,-3.80002044322169));
#56617=CARTESIAN_POINT('Ctrl Pts',(-1.38389311766701,1.,-3.80002044322169));
#56618=CARTESIAN_POINT('Ctrl Pts',(-1.38409399694589,-1.,-3.79235669640907));
#56619=CARTESIAN_POINT('Ctrl Pts',(-1.38409399694589,1.,-3.79235669640907));
#56620=CARTESIAN_POINT('Ctrl Pts',(-1.38425435883773,-1.,-3.78469969805134));
#56621=CARTESIAN_POINT('Ctrl Pts',(-1.38425435883773,1.,-3.78469969805134));
#56622=CARTESIAN_POINT('Ctrl Pts',(-1.38437354551435,-1.,-3.77704902230441));
#56623=CARTESIAN_POINT('Ctrl Pts',(-1.38437354551435,1.,-3.77704902230441));
#56624=CARTESIAN_POINT('Ctrl Pts',(-1.38445107339517,-1.,-3.76940473185775));
#56625=CARTESIAN_POINT('Ctrl Pts',(-1.38445107339517,1.,-3.76940473185775));
#56626=CARTESIAN_POINT('Ctrl Pts',(-1.38448675253343,-1.,-3.76176768271347));
#56627=CARTESIAN_POINT('Ctrl Pts',(-1.38448675253343,1.,-3.76176768271347));
#56628=CARTESIAN_POINT('Ctrl Pts',(-1.38448077997155,-1.,-3.75413976318727));
#56629=CARTESIAN_POINT('Ctrl Pts',(-1.38448077997155,1.,-3.75413976318727));
#56630=CARTESIAN_POINT('Ctrl Pts',(-1.38443344984389,-1.,-3.7465231716786));
#56631=CARTESIAN_POINT('Ctrl Pts',(-1.38443344984389,1.,-3.7465231716786));
#56632=CARTESIAN_POINT('Ctrl Pts',(-1.38434489156456,-1.,-3.73891976418099));
#56633=CARTESIAN_POINT('Ctrl Pts',(-1.38434489156456,1.,-3.73891976418099));
#56634=CARTESIAN_POINT('Ctrl Pts',(-1.38421479111531,-1.,-3.73133035859283));
#56635=CARTESIAN_POINT('Ctrl Pts',(-1.38421479111531,1.,-3.73133035859283));
#56636=CARTESIAN_POINT('Ctrl Pts',(-1.3840421342895,-1.,-3.72375409358805));
#56637=CARTESIAN_POINT('Ctrl Pts',(-1.3840421342895,1.,-3.72375409358805));
#56638=CARTESIAN_POINT('Ctrl Pts',(-1.38382489984585,-1.,-3.7161876605181));
#56639=CARTESIAN_POINT('Ctrl Pts',(-1.38382489984585,1.,-3.7161876605181));
#56640=CARTESIAN_POINT('Ctrl Pts',(-1.38356065402122,-1.,-3.70862680753343));
#56641=CARTESIAN_POINT('Ctrl Pts',(-1.38356065402122,1.,-3.70862680753343));
#56642=CARTESIAN_POINT('Ctrl Pts',(-1.38324717612862,-1.,-3.70106792167894));
#56643=CARTESIAN_POINT('Ctrl Pts',(-1.38324717612862,1.,-3.70106792167894));
#56644=CARTESIAN_POINT('Ctrl Pts',(-1.38288311171649,-1.,-3.69350967899523));
#56645=CARTESIAN_POINT('Ctrl Pts',(-1.38288311171649,1.,-3.69350967899523));
#56646=CARTESIAN_POINT('Ctrl Pts',(-1.38246852827185,-1.,-3.68595444983844));
#56647=CARTESIAN_POINT('Ctrl Pts',(-1.38246852827185,1.,-3.68595444983844));
#56648=CARTESIAN_POINT('Ctrl Pts',(-1.38200574290626,-1.,-3.6784103848243));
#56649=CARTESIAN_POINT('Ctrl Pts',(-1.38200574290626,1.,-3.6784103848243));
#56650=CARTESIAN_POINT('Ctrl Pts',(-1.38149812653876,-1.,-3.67088843112282));
#56651=CARTESIAN_POINT('Ctrl Pts',(-1.38149812653876,1.,-3.67088843112282));
#56652=CARTESIAN_POINT('Ctrl Pts',(-1.38094856333558,-1.,-3.66339848520874));
#56653=CARTESIAN_POINT('Ctrl Pts',(-1.38094856333558,1.,-3.66339848520874));
#56654=CARTESIAN_POINT('Ctrl Pts',(-1.38035791051215,-1.,-3.65594554404396));
#56655=CARTESIAN_POINT('Ctrl Pts',(-1.38035791051215,1.,-3.65594554404396));
#56656=CARTESIAN_POINT('Ctrl Pts',(-1.37972372481598,-1.,-3.64852652756444));
#56657=CARTESIAN_POINT('Ctrl Pts',(-1.37972372481598,1.,-3.64852652756444));
#56658=CARTESIAN_POINT('Ctrl Pts',(-1.37903818567347,-1.,-3.64112507791112));
#56659=CARTESIAN_POINT('Ctrl Pts',(-1.37903818567347,1.,-3.64112507791112));
#56660=CARTESIAN_POINT('Ctrl Pts',(-1.37829035457324,-1.,-3.63371727442448));
#56661=CARTESIAN_POINT('Ctrl Pts',(-1.37829035457324,1.,-3.63371727442448));
#56662=CARTESIAN_POINT('Ctrl Pts',(-1.37746987919868,-1.,-3.62628098665112));
#56663=CARTESIAN_POINT('Ctrl Pts',(-1.37746987919868,1.,-3.62628098665112));
#56664=CARTESIAN_POINT('Ctrl Pts',(-1.37657053403102,-1.,-3.61880481160408));
#56665=CARTESIAN_POINT('Ctrl Pts',(-1.37657053403102,1.,-3.61880481160408));
#56666=CARTESIAN_POINT('Ctrl Pts',(-1.37559314436641,-1.,-3.61129546591082));
#56667=CARTESIAN_POINT('Ctrl Pts',(-1.37559314436641,1.,-3.61129546591082));
#56668=CARTESIAN_POINT('Ctrl Pts',(-1.37455051379642,-1.,-3.60379020124038));
#56669=CARTESIAN_POINT('Ctrl Pts',(-1.37455051379642,1.,-3.60379020124038));
#56670=CARTESIAN_POINT('Ctrl Pts',(-1.37346320103184,-1.,-3.59634627869117));
#56671=CARTESIAN_POINT('Ctrl Pts',(-1.37346320103184,1.,-3.59634627869117));
#56672=CARTESIAN_POINT('Ctrl Pts',(-1.37235053661,-1.,-3.5890185384643));
#56673=CARTESIAN_POINT('Ctrl Pts',(-1.37235053661,1.,-3.5890185384643));
#56674=CARTESIAN_POINT('Ctrl Pts',(-1.37122241663073,-1.,-3.58183885982745));
#56675=CARTESIAN_POINT('Ctrl Pts',(-1.37122241663073,1.,-3.58183885982745));
#56676=CARTESIAN_POINT('Ctrl Pts',(-1.37007229485646,-1.,-3.57479875549453));
#56677=CARTESIAN_POINT('Ctrl Pts',(-1.37007229485646,1.,-3.57479875549453));
#56678=CARTESIAN_POINT('Ctrl Pts',(-1.36886584973349,-1.,-3.56782080304554));
#56679=CARTESIAN_POINT('Ctrl Pts',(-1.36886584973349,1.,-3.56782080304554));
#56680=CARTESIAN_POINT('Ctrl Pts',(-1.36754771771174,-1.,-3.56077662028492));
#56681=CARTESIAN_POINT('Ctrl Pts',(-1.36754771771174,1.,-3.56077662028492));
#56682=CARTESIAN_POINT('Ctrl Pts',(-1.36606145456711,-1.,-3.55353883995793));
#56683=CARTESIAN_POINT('Ctrl Pts',(-1.36606145456711,1.,-3.55353883995793));
#56684=CARTESIAN_POINT('Ctrl Pts',(-1.36436666257567,-1.,-3.54602591832893));
#56685=CARTESIAN_POINT('Ctrl Pts',(-1.36436666257567,1.,-3.54602591832893));
#56686=CARTESIAN_POINT('Ctrl Pts',(-1.36245507339334,-1.,-3.53824396425032));
#56687=CARTESIAN_POINT('Ctrl Pts',(-1.36245507339334,1.,-3.53824396425032));
#56688=CARTESIAN_POINT('Ctrl Pts',(-1.36037259643827,-1.,-3.53034464961849));
#56689=CARTESIAN_POINT('Ctrl Pts',(-1.36037259643827,1.,-3.53034464961849));
#56690=CARTESIAN_POINT('Ctrl Pts',(-1.35821701528975,-1.,-3.52261776117121));
#56691=CARTESIAN_POINT('Ctrl Pts',(-1.35821701528975,1.,-3.52261776117121));
#56692=CARTESIAN_POINT('Ctrl Pts',(-1.35611275237288,-1.,-3.51542230699919));
#56693=CARTESIAN_POINT('Ctrl Pts',(-1.35611275237288,1.,-3.51542230699919));
#56694=CARTESIAN_POINT('Ctrl Pts',(-1.35419113576022,-1.,-3.50913227060177));
#56695=CARTESIAN_POINT('Ctrl Pts',(-1.35419113576022,1.,-3.50913227060177));
#56696=CARTESIAN_POINT('Ctrl Pts',(-1.3525703284343,-1.,-3.50408168106113));
#56697=CARTESIAN_POINT('Ctrl Pts',(-1.3525703284343,1.,-3.50408168106113));
#56698=CARTESIAN_POINT('Ctrl Pts',(-1.35133076331065,-1.,-3.50049707063673));
#56699=CARTESIAN_POINT('Ctrl Pts',(-1.35133076331065,1.,-3.50049707063673));
#56700=CARTESIAN_POINT('Ctrl Pts',(-1.35067437417289,-1.,-3.49888720256612));
#56701=CARTESIAN_POINT('Ctrl Pts',(-1.35067437417289,1.,-3.49888720256612));
#56702=CARTESIAN_POINT('Ctrl Pts',(-1.35037650302887,-1.,-3.49840357193384));
#56703=CARTESIAN_POINT('Ctrl Pts',(-1.35037650302887,1.,-3.49840357193384));
#56704=CARTESIAN_POINT('Ctrl Pts',(-1.35026426118351,-1.,-3.49840260053616));
#56705=CARTESIAN_POINT('Ctrl Pts',(-1.35026426118351,1.,-3.49840260053616));
#56706=CARTESIAN_POINT('Ctrl Pts',(-1.35022972712301,-1.,-3.49848248301936));
#56707=CARTESIAN_POINT('Ctrl Pts',(-1.35022972712301,1.,-3.49848248301936));
#56708=CARTESIAN_POINT('',(-1.36999806084572,1.,-3.97027773754922));
#56709=CARTESIAN_POINT('Ctrl Pts',(-1.36999806084572,1.,-3.97027773754922));
#56710=CARTESIAN_POINT('Ctrl Pts',(-1.37020239094758,1.,-3.9687184694173));
#56711=CARTESIAN_POINT('Ctrl Pts',(-1.37060761746027,1.,-3.96560037975788));
#56712=CARTESIAN_POINT('Ctrl Pts',(-1.37120515615663,1.,-3.96092458508407));
#56713=CARTESIAN_POINT('Ctrl Pts',(-1.37198126433139,1.,-3.95469287283105));
#56714=CARTESIAN_POINT('Ctrl Pts',(-1.37291699203423,1.,-3.94690771786926));
#56715=CARTESIAN_POINT('Ctrl Pts',(-1.37381821967499,1.,-3.93912709041791));
#56716=CARTESIAN_POINT('Ctrl Pts',(-1.37468482215784,1.,-3.93135106761941));
#56717=CARTESIAN_POINT('Ctrl Pts',(-1.37551664448057,1.,-3.92357976987132));
#56718=CARTESIAN_POINT('Ctrl Pts',(-1.37631350505516,1.,-3.91581337461825));
#56719=CARTESIAN_POINT('Ctrl Pts',(-1.3770751963376,1.,-3.90805209522729));
#56720=CARTESIAN_POINT('Ctrl Pts',(-1.3778014851263,1.,-3.90029615196255));
#56721=CARTESIAN_POINT('Ctrl Pts',(-1.37849211287981,1.,-3.89254574338385));
#56722=CARTESIAN_POINT('Ctrl Pts',(-1.37914679719446,1.,-3.88480102249461));
#56723=CARTESIAN_POINT('Ctrl Pts',(-1.37976523097187,1.,-3.87706205830865));
#56724=CARTESIAN_POINT('Ctrl Pts',(-1.38034709213129,1.,-3.86932885813403));
#56725=CARTESIAN_POINT('Ctrl Pts',(-1.38089205993067,1.,-3.86160143044187));
#56726=CARTESIAN_POINT('Ctrl Pts',(-1.38139983115075,1.,-3.85387983979557));
#56727=CARTESIAN_POINT('Ctrl Pts',(-1.38187013346089,1.,-3.84616425605705));
#56728=CARTESIAN_POINT('Ctrl Pts',(-1.38230274828774,1.,-3.83845502790609));
#56729=CARTESIAN_POINT('Ctrl Pts',(-1.38269750245086,1.,-3.83075266982138));
#56730=CARTESIAN_POINT('Ctrl Pts',(-1.38305421262724,1.,-3.82305771743715));
#56731=CARTESIAN_POINT('Ctrl Pts',(-1.38337263902766,1.,-3.81537060817765));
#56732=CARTESIAN_POINT('Ctrl Pts',(-1.38365244046226,1.,-3.80769156398429));
#56733=CARTESIAN_POINT('Ctrl Pts',(-1.38389311766701,1.,-3.80002044322169));
#56734=CARTESIAN_POINT('Ctrl Pts',(-1.38409399694589,1.,-3.79235669640907));
#56735=CARTESIAN_POINT('Ctrl Pts',(-1.38425435883773,1.,-3.78469969805134));
#56736=CARTESIAN_POINT('Ctrl Pts',(-1.38437354551435,1.,-3.77704902230441));
#56737=CARTESIAN_POINT('Ctrl Pts',(-1.38445107339517,1.,-3.76940473185775));
#56738=CARTESIAN_POINT('Ctrl Pts',(-1.38448675253343,1.,-3.76176768271347));
#56739=CARTESIAN_POINT('Ctrl Pts',(-1.38448077997155,1.,-3.75413976318727));
#56740=CARTESIAN_POINT('Ctrl Pts',(-1.38443344984389,1.,-3.7465231716786));
#56741=CARTESIAN_POINT('Ctrl Pts',(-1.38434489156456,1.,-3.73891976418099));
#56742=CARTESIAN_POINT('Ctrl Pts',(-1.38421479111531,1.,-3.73133035859283));
#56743=CARTESIAN_POINT('Ctrl Pts',(-1.3840421342895,1.,-3.72375409358805));
#56744=CARTESIAN_POINT('Ctrl Pts',(-1.38382489984585,1.,-3.7161876605181));
#56745=CARTESIAN_POINT('Ctrl Pts',(-1.38356065402122,1.,-3.70862680753343));
#56746=CARTESIAN_POINT('Ctrl Pts',(-1.38324717612862,1.,-3.70106792167894));
#56747=CARTESIAN_POINT('Ctrl Pts',(-1.38288311171649,1.,-3.69350967899523));
#56748=CARTESIAN_POINT('Ctrl Pts',(-1.38246852827185,1.,-3.68595444983844));
#56749=CARTESIAN_POINT('Ctrl Pts',(-1.38200574290626,1.,-3.6784103848243));
#56750=CARTESIAN_POINT('Ctrl Pts',(-1.38149812653876,1.,-3.67088843112282));
#56751=CARTESIAN_POINT('Ctrl Pts',(-1.38094856333558,1.,-3.66339848520874));
#56752=CARTESIAN_POINT('Ctrl Pts',(-1.38035791051215,1.,-3.65594554404396));
#56753=CARTESIAN_POINT('Ctrl Pts',(-1.37972372481598,1.,-3.64852652756444));
#56754=CARTESIAN_POINT('Ctrl Pts',(-1.37903818567347,1.,-3.64112507791112));
#56755=CARTESIAN_POINT('Ctrl Pts',(-1.37829035457324,1.,-3.63371727442448));
#56756=CARTESIAN_POINT('Ctrl Pts',(-1.37746987919868,1.,-3.62628098665112));
#56757=CARTESIAN_POINT('Ctrl Pts',(-1.37657053403102,1.,-3.61880481160408));
#56758=CARTESIAN_POINT('Ctrl Pts',(-1.37559314436641,1.,-3.61129546591082));
#56759=CARTESIAN_POINT('Ctrl Pts',(-1.37455051379642,1.,-3.60379020124038));
#56760=CARTESIAN_POINT('Ctrl Pts',(-1.37346320103184,1.,-3.59634627869117));
#56761=CARTESIAN_POINT('Ctrl Pts',(-1.37235053661,1.,-3.5890185384643));
#56762=CARTESIAN_POINT('Ctrl Pts',(-1.37122241663073,1.,-3.58183885982745));
#56763=CARTESIAN_POINT('Ctrl Pts',(-1.37007229485646,1.,-3.57479875549453));
#56764=CARTESIAN_POINT('Ctrl Pts',(-1.36886584973349,1.,-3.56782080304554));
#56765=CARTESIAN_POINT('Ctrl Pts',(-1.36754771771174,1.,-3.56077662028492));
#56766=CARTESIAN_POINT('Ctrl Pts',(-1.36606145456711,1.,-3.55353883995793));
#56767=CARTESIAN_POINT('Ctrl Pts',(-1.36436666257567,1.,-3.54602591832893));
#56768=CARTESIAN_POINT('Ctrl Pts',(-1.36245507339334,1.,-3.53824396425032));
#56769=CARTESIAN_POINT('Ctrl Pts',(-1.36037259643827,1.,-3.53034464961849));
#56770=CARTESIAN_POINT('Ctrl Pts',(-1.35821701528975,1.,-3.52261776117121));
#56771=CARTESIAN_POINT('Ctrl Pts',(-1.35611275237288,1.,-3.51542230699919));
#56772=CARTESIAN_POINT('Ctrl Pts',(-1.35419113576022,1.,-3.50913227060177));
#56773=CARTESIAN_POINT('Ctrl Pts',(-1.3525703284343,1.,-3.50408168106113));
#56774=CARTESIAN_POINT('Ctrl Pts',(-1.35142377279535,1.,-3.5007660381658));
#56775=CARTESIAN_POINT('Ctrl Pts',(-1.35080045218652,1.,-3.49920025459856));
#56776=CARTESIAN_POINT('Ctrl Pts',(-1.35049736560633,1.,-3.49861894124915));
#56777=CARTESIAN_POINT('Ctrl Pts',(-1.35036670893102,1.,-3.49847119623841));
#56778=CARTESIAN_POINT('Ctrl Pts',(-1.35032489087269,1.,-3.49844575334386));
#56779=CARTESIAN_POINT('',(-1.36999806084572,0.,-3.97027773754922));
#56780=CARTESIAN_POINT('Ctrl Pts',(-0.96399761336957,-1.,-3.62397690409552));
#56781=CARTESIAN_POINT('Ctrl Pts',(-0.96399761336957,1.,-3.62397690409552));
#56782=CARTESIAN_POINT('Ctrl Pts',(-0.963922720982576,-1.,-3.62393257642191));
#56783=CARTESIAN_POINT('Ctrl Pts',(-0.963922720982576,1.,-3.62393257642191));
#56784=CARTESIAN_POINT('Ctrl Pts',(-0.963832486396055,-1.,-3.62399933640277));
#56785=CARTESIAN_POINT('Ctrl Pts',(-0.963832486396055,1.,-3.62399933640277));
#56786=CARTESIAN_POINT('Ctrl Pts',(-0.963875774532103,-1.,-3.62456568607055));
#56787=CARTESIAN_POINT('Ctrl Pts',(-0.963875774532103,1.,-3.62456568607055));
#56788=CARTESIAN_POINT('Ctrl Pts',(-0.964291001274618,-1.,-3.62625391255277));
#56789=CARTESIAN_POINT('Ctrl Pts',(-0.964291001274618,1.,-3.62625391255277));
#56790=CARTESIAN_POINT('Ctrl Pts',(-0.965395153165716,-1.,-3.62988252139998));
#56791=CARTESIAN_POINT('Ctrl Pts',(-0.965395153165716,1.,-3.62988252139998));
#56792=CARTESIAN_POINT('Ctrl Pts',(-0.967052554540877,-1.,-3.6349212208096));
#56793=CARTESIAN_POINT('Ctrl Pts',(-0.967052554540877,1.,-3.6349212208096));
#56794=CARTESIAN_POINT('Ctrl Pts',(-0.969195124674829,-1.,-3.64113946505393));
#56795=CARTESIAN_POINT('Ctrl Pts',(-0.969195124674829,1.,-3.64113946505393));
#56796=CARTESIAN_POINT('Ctrl Pts',(-0.971722122060277,-1.,-3.64819756447072));
#56797=CARTESIAN_POINT('Ctrl Pts',(-0.971722122060277,1.,-3.64819756447072));
#56798=CARTESIAN_POINT('Ctrl Pts',(-0.974519971354139,-1.,-3.6557157673487));
#56799=CARTESIAN_POINT('Ctrl Pts',(-0.974519971354139,1.,-3.6557157673487));
#56800=CARTESIAN_POINT('Ctrl Pts',(-0.977478312751416,-1.,-3.66333049637403));
#56801=CARTESIAN_POINT('Ctrl Pts',(-0.977478312751416,1.,-3.66333049637403));
#56802=CARTESIAN_POINT('Ctrl Pts',(-0.980505922458494,-1.,-3.67074983340444));
#56803=CARTESIAN_POINT('Ctrl Pts',(-0.980505922458494,1.,-3.67074983340444));
#56804=CARTESIAN_POINT('Ctrl Pts',(-0.983550791470864,-1.,-3.67782408841876));
#56805=CARTESIAN_POINT('Ctrl Pts',(-0.983550791470864,1.,-3.67782408841876));
#56806=CARTESIAN_POINT('Ctrl Pts',(-0.986602639864286,-1.,-3.6845531792623));
#56807=CARTESIAN_POINT('Ctrl Pts',(-0.986602639864286,1.,-3.6845531792623));
#56808=CARTESIAN_POINT('Ctrl Pts',(-0.989676715398858,-1.,-3.69102682138955));
#56809=CARTESIAN_POINT('Ctrl Pts',(-0.989676715398858,1.,-3.69102682138955));
#56810=CARTESIAN_POINT('Ctrl Pts',(-0.992802218332104,-1.,-3.69738123415696));
#56811=CARTESIAN_POINT('Ctrl Pts',(-0.992802218332104,1.,-3.69738123415696));
#56812=CARTESIAN_POINT('Ctrl Pts',(-0.996009819772432,-1.,-3.70375282282107));
#56813=CARTESIAN_POINT('Ctrl Pts',(-0.996009819772432,1.,-3.70375282282107));
#56814=CARTESIAN_POINT('Ctrl Pts',(-0.999317260756344,-1.,-3.7102243971387));
#56815=CARTESIAN_POINT('Ctrl Pts',(-0.999317260756344,1.,-3.7102243971387));
#56816=CARTESIAN_POINT('Ctrl Pts',(-1.00272423396802,-1.,-3.71680667125047));
#56817=CARTESIAN_POINT('Ctrl Pts',(-1.00272423396802,1.,-3.71680667125047));
#56818=CARTESIAN_POINT('Ctrl Pts',(-1.00622000735696,-1.,-3.72346803750544));
#56819=CARTESIAN_POINT('Ctrl Pts',(-1.00622000735696,1.,-3.72346803750544));
#56820=CARTESIAN_POINT('Ctrl Pts',(-1.00978798539491,-1.,-3.73015276704407));
#56821=CARTESIAN_POINT('Ctrl Pts',(-1.00978798539491,1.,-3.73015276704407));
#56822=CARTESIAN_POINT('Ctrl Pts',(-1.01341114319906,-1.,-3.73680245055747));
#56823=CARTESIAN_POINT('Ctrl Pts',(-1.01341114319906,1.,-3.73680245055747));
#56824=CARTESIAN_POINT('Ctrl Pts',(-1.01707794311088,-1.,-3.74337942504993));
#56825=CARTESIAN_POINT('Ctrl Pts',(-1.01707794311088,1.,-3.74337942504993));
#56826=CARTESIAN_POINT('Ctrl Pts',(-1.02078510487439,-1.,-3.74987777155873));
#56827=CARTESIAN_POINT('Ctrl Pts',(-1.02078510487439,1.,-3.74987777155873));
#56828=CARTESIAN_POINT('Ctrl Pts',(-1.02453429444668,-1.,-3.75631037456224));
#56829=CARTESIAN_POINT('Ctrl Pts',(-1.02453429444668,1.,-3.75631037456224));
#56830=CARTESIAN_POINT('Ctrl Pts',(-1.02833014458184,-1.,-3.76270122291245));
#56831=CARTESIAN_POINT('Ctrl Pts',(-1.02833014458184,1.,-3.76270122291245));
#56832=CARTESIAN_POINT('Ctrl Pts',(-1.03217786604919,-1.,-3.76907609832516));
#56833=CARTESIAN_POINT('Ctrl Pts',(-1.03217786604919,1.,-3.76907609832516));
#56834=CARTESIAN_POINT('Ctrl Pts',(-1.03608074678008,-1.,-3.77545283140427));
#56835=CARTESIAN_POINT('Ctrl Pts',(-1.03608074678008,1.,-3.77545283140427));
#56836=CARTESIAN_POINT('Ctrl Pts',(-1.04003862055798,-1.,-3.7818353500817));
#56837=CARTESIAN_POINT('Ctrl Pts',(-1.04003862055798,1.,-3.7818353500817));
#56838=CARTESIAN_POINT('Ctrl Pts',(-1.04404924374422,-1.,-3.78821910787179));
#56839=CARTESIAN_POINT('Ctrl Pts',(-1.04404924374422,1.,-3.78821910787179));
#56840=CARTESIAN_POINT('Ctrl Pts',(-1.04810913267639,-1.,-3.79459440308786));
#56841=CARTESIAN_POINT('Ctrl Pts',(-1.04810913267639,1.,-3.79459440308786));
#56842=CARTESIAN_POINT('Ctrl Pts',(-1.05221457990016,-1.,-3.80095039790681));
#56843=CARTESIAN_POINT('Ctrl Pts',(-1.05221457990016,1.,-3.80095039790681));
#56844=CARTESIAN_POINT('Ctrl Pts',(-1.05636266918644,-1.,-3.80727913637791));
#56845=CARTESIAN_POINT('Ctrl Pts',(-1.05636266918644,1.,-3.80727913637791));
#56846=CARTESIAN_POINT('Ctrl Pts',(-1.06055206187299,-1.,-3.8135786611749));
#56847=CARTESIAN_POINT('Ctrl Pts',(-1.06055206187299,1.,-3.8135786611749));
#56848=CARTESIAN_POINT('Ctrl Pts',(-1.0647824403893,-1.,-3.81985083953012));
#56849=CARTESIAN_POINT('Ctrl Pts',(-1.0647824403893,1.,-3.81985083953012));
#56850=CARTESIAN_POINT('Ctrl Pts',(-1.06905413180359,-1.,-3.82609989967276));
#56851=CARTESIAN_POINT('Ctrl Pts',(-1.06905413180359,1.,-3.82609989967276));
#56852=CARTESIAN_POINT('Ctrl Pts',(-1.07336766633459,-1.,-3.83233071195144));
#56853=CARTESIAN_POINT('Ctrl Pts',(-1.07336766633459,1.,-3.83233071195144));
#56854=CARTESIAN_POINT('Ctrl Pts',(-1.07772335353858,-1.,-3.83854714117491));
#56855=CARTESIAN_POINT('Ctrl Pts',(-1.07772335353858,1.,-3.83854714117491));
#56856=CARTESIAN_POINT('Ctrl Pts',(-1.08212087917991,-1.,-3.8447504803063));
#56857=CARTESIAN_POINT('Ctrl Pts',(-1.08212087917991,1.,-3.8447504803063));
#56858=CARTESIAN_POINT('Ctrl Pts',(-1.08655950846384,-1.,-3.85094025222713));
#56859=CARTESIAN_POINT('Ctrl Pts',(-1.08655950846384,1.,-3.85094025222713));
#56860=CARTESIAN_POINT('Ctrl Pts',(-1.09103825516294,-1.,-3.85711487933931));
#56861=CARTESIAN_POINT('Ctrl Pts',(-1.09103825516294,1.,-3.85711487933931));
#56862=CARTESIAN_POINT('Ctrl Pts',(-1.09555606505013,-1.,-3.86327241021247));
#56863=CARTESIAN_POINT('Ctrl Pts',(-1.09555606505013,1.,-3.86327241021247));
#56864=CARTESIAN_POINT('Ctrl Pts',(-1.10011198761195,-1.,-3.86941120134849));
#56865=CARTESIAN_POINT('Ctrl Pts',(-1.10011198761195,1.,-3.86941120134849));
#56866=CARTESIAN_POINT('Ctrl Pts',(-1.10470536603287,-1.,-3.87553067187514));
#56867=CARTESIAN_POINT('Ctrl Pts',(-1.10470536603287,1.,-3.87553067187514));
#56868=CARTESIAN_POINT('Ctrl Pts',(-1.10933577224008,-1.,-3.88163105531724));
#56869=CARTESIAN_POINT('Ctrl Pts',(-1.10933577224008,1.,-3.88163105531724));
#56870=CARTESIAN_POINT('Ctrl Pts',(-1.11400292434429,-1.,-3.88771308285171));
#56871=CARTESIAN_POINT('Ctrl Pts',(-1.11400292434429,1.,-3.88771308285171));
#56872=CARTESIAN_POINT('Ctrl Pts',(-1.11870660794603,-1.,-3.89377768340344));
#56873=CARTESIAN_POINT('Ctrl Pts',(-1.11870660794603,1.,-3.89377768340344));
#56874=CARTESIAN_POINT('Ctrl Pts',(-1.12344660099043,-1.,-3.89982569750025));
#56875=CARTESIAN_POINT('Ctrl Pts',(-1.12344660099043,1.,-3.89982569750025));
#56876=CARTESIAN_POINT('Ctrl Pts',(-1.12822258281553,-1.,-3.90585753318737));
#56877=CARTESIAN_POINT('Ctrl Pts',(-1.12822258281553,1.,-3.90585753318737));
#56878=CARTESIAN_POINT('Ctrl Pts',(-1.13303414693896,-1.,-3.91187321145649));
#56879=CARTESIAN_POINT('Ctrl Pts',(-1.13303414693896,1.,-3.91187321145649));
#56880=CARTESIAN_POINT('Ctrl Pts',(-1.13788084225554,-1.,-3.91787251936827));
#56881=CARTESIAN_POINT('Ctrl Pts',(-1.13788084225554,1.,-3.91787251936827));
#56882=CARTESIAN_POINT('Ctrl Pts',(-1.14276220561593,-1.,-3.92385513133997));
#56883=CARTESIAN_POINT('Ctrl Pts',(-1.14276220561593,1.,-3.92385513133997));
#56884=CARTESIAN_POINT('Ctrl Pts',(-1.14767779451123,-1.,-3.92982073294257));
#56885=CARTESIAN_POINT('Ctrl Pts',(-1.14767779451123,1.,-3.92982073294257));
#56886=CARTESIAN_POINT('Ctrl Pts',(-1.1526272271632,-1.,-3.9357691705628));
#56887=CARTESIAN_POINT('Ctrl Pts',(-1.1526272271632,1.,-3.9357691705628));
#56888=CARTESIAN_POINT('Ctrl Pts',(-1.15761018340956,-1.,-3.94170046685203));
#56889=CARTESIAN_POINT('Ctrl Pts',(-1.15761018340956,1.,-3.94170046685203));
#56890=CARTESIAN_POINT('Ctrl Pts',(-1.16262637999157,-1.,-3.94761474780583));
#56891=CARTESIAN_POINT('Ctrl Pts',(-1.16262637999157,1.,-3.94761474780583));
#56892=CARTESIAN_POINT('Ctrl Pts',(-1.16767555244438,-1.,-3.95351219509876));
#56893=CARTESIAN_POINT('Ctrl Pts',(-1.16767555244438,1.,-3.95351219509876));
#56894=CARTESIAN_POINT('Ctrl Pts',(-1.17275743590361,-1.,-3.95939299213276));
#56895=CARTESIAN_POINT('Ctrl Pts',(-1.17275743590361,1.,-3.95939299213276));
#56896=CARTESIAN_POINT('Ctrl Pts',(-1.17787174135592,-1.,-3.96525726358159));
#56897=CARTESIAN_POINT('Ctrl Pts',(-1.17787174135592,1.,-3.96525726358159));
#56898=CARTESIAN_POINT('Ctrl Pts',(-1.18301815039831,-1.,-3.97110505165415));
#56899=CARTESIAN_POINT('Ctrl Pts',(-1.18301815039831,1.,-3.97110505165415));
#56900=CARTESIAN_POINT('Ctrl Pts',(-1.18819633715539,-1.,-3.97693634767754));
#56901=CARTESIAN_POINT('Ctrl Pts',(-1.18819633715539,1.,-3.97693634767754));
#56902=CARTESIAN_POINT('Ctrl Pts',(-1.19340598349475,-1.,-3.98275111052561));
#56903=CARTESIAN_POINT('Ctrl Pts',(-1.19340598349475,1.,-3.98275111052561));
#56904=CARTESIAN_POINT('Ctrl Pts',(-1.19864679609566,-1.,-3.98854928957189));
#56905=CARTESIAN_POINT('Ctrl Pts',(-1.19864679609566,1.,-3.98854928957189));
#56906=CARTESIAN_POINT('Ctrl Pts',(-1.20391852375139,-1.,-3.99433084799666));
#56907=CARTESIAN_POINT('Ctrl Pts',(-1.20391852375139,1.,-3.99433084799666));
#56908=CARTESIAN_POINT('Ctrl Pts',(-1.20922097029551,-1.,-4.00009577950721));
#56909=CARTESIAN_POINT('Ctrl Pts',(-1.20922097029551,1.,-4.00009577950721));
#56910=CARTESIAN_POINT('Ctrl Pts',(-1.21455398918133,-1.,-4.00584409522722));
#56911=CARTESIAN_POINT('Ctrl Pts',(-1.21455398918133,1.,-4.00584409522722));
#56912=CARTESIAN_POINT('Ctrl Pts',(-1.21884478244403,-1.,-4.01042947140789));
#56913=CARTESIAN_POINT('Ctrl Pts',(-1.21884478244403,1.,-4.01042947140789));
#56914=CARTESIAN_POINT('Ctrl Pts',(-1.22207656455845,-1.,-4.01386104433519));
#56915=CARTESIAN_POINT('Ctrl Pts',(-1.22207656455845,1.,-4.01386104433519));
#56916=CARTESIAN_POINT('Ctrl Pts',(-1.22423716681317,-1.,-4.01614544569895));
#56917=CARTESIAN_POINT('Ctrl Pts',(-1.22423716681317,1.,-4.01614544569895));
#56918=CARTESIAN_POINT('Ctrl Pts',(-1.22531898815164,-1.,-4.01728681790024));
#56919=CARTESIAN_POINT('Ctrl Pts',(-1.22531898815164,1.,-4.01728681790024));
#56920=CARTESIAN_POINT('',(-0.963899035118984,1.,-3.62400312501199));
#56921=CARTESIAN_POINT('Ctrl Pts',(-0.963899035118985,-1.,-3.62400312501199));
#56922=CARTESIAN_POINT('Ctrl Pts',(-0.963899035118985,-0.666666666666667,
-3.62400312501199));
#56923=CARTESIAN_POINT('Ctrl Pts',(-0.963899035118985,-0.333333333333333,
-3.62400312501199));
#56924=CARTESIAN_POINT('Ctrl Pts',(-0.963899035118985,0.333333333333333,
-3.62400312501199));
#56925=CARTESIAN_POINT('Ctrl Pts',(-0.963899035118986,0.666666666666667,
-3.62400312501199));
#56926=CARTESIAN_POINT('Ctrl Pts',(-0.963899035118986,1.,-3.62400312501199));
#56927=CARTESIAN_POINT('',(-1.22531898815164,1.,-4.01728681790024));
#56928=CARTESIAN_POINT('',(-1.22531898815164,0.,-4.01728681790024));
#56929=CARTESIAN_POINT('Ctrl Pts',(-0.963899035118985,1.,-3.62400312501199));
#56930=CARTESIAN_POINT('Ctrl Pts',(-0.963880158556713,1.,-3.62404828878375));
#56931=CARTESIAN_POINT('Ctrl Pts',(-0.963861297423579,1.,-3.62424461507455));
#56932=CARTESIAN_POINT('Ctrl Pts',(-0.963957782642589,1.,-3.62489305727516));
#56933=CARTESIAN_POINT('Ctrl Pts',(-0.964373850166081,1.,-3.62652618145252));
#56934=CARTESIAN_POINT('Ctrl Pts',(-0.965395153165716,1.,-3.62988252139998));
#56935=CARTESIAN_POINT('Ctrl Pts',(-0.967052554540877,1.,-3.6349212208096));
#56936=CARTESIAN_POINT('Ctrl Pts',(-0.969195124674829,1.,-3.64113946505393));
#56937=CARTESIAN_POINT('Ctrl Pts',(-0.971722122060277,1.,-3.64819756447072));
#56938=CARTESIAN_POINT('Ctrl Pts',(-0.974519971354139,1.,-3.6557157673487));
#56939=CARTESIAN_POINT('Ctrl Pts',(-0.977478312751416,1.,-3.66333049637403));
#56940=CARTESIAN_POINT('Ctrl Pts',(-0.980505922458494,1.,-3.67074983340444));
#56941=CARTESIAN_POINT('Ctrl Pts',(-0.983550791470864,1.,-3.67782408841876));
#56942=CARTESIAN_POINT('Ctrl Pts',(-0.986602639864286,1.,-3.6845531792623));
#56943=CARTESIAN_POINT('Ctrl Pts',(-0.989676715398858,1.,-3.69102682138955));
#56944=CARTESIAN_POINT('Ctrl Pts',(-0.992802218332104,1.,-3.69738123415696));
#56945=CARTESIAN_POINT('Ctrl Pts',(-0.996009819772432,1.,-3.70375282282107));
#56946=CARTESIAN_POINT('Ctrl Pts',(-0.999317260756344,1.,-3.7102243971387));
#56947=CARTESIAN_POINT('Ctrl Pts',(-1.00272423396802,1.,-3.71680667125047));
#56948=CARTESIAN_POINT('Ctrl Pts',(-1.00622000735696,1.,-3.72346803750544));
#56949=CARTESIAN_POINT('Ctrl Pts',(-1.00978798539491,1.,-3.73015276704407));
#56950=CARTESIAN_POINT('Ctrl Pts',(-1.01341114319906,1.,-3.73680245055747));
#56951=CARTESIAN_POINT('Ctrl Pts',(-1.01707794311088,1.,-3.74337942504993));
#56952=CARTESIAN_POINT('Ctrl Pts',(-1.02078510487439,1.,-3.74987777155873));
#56953=CARTESIAN_POINT('Ctrl Pts',(-1.02453429444668,1.,-3.75631037456224));
#56954=CARTESIAN_POINT('Ctrl Pts',(-1.02833014458184,1.,-3.76270122291245));
#56955=CARTESIAN_POINT('Ctrl Pts',(-1.03217786604919,1.,-3.76907609832516));
#56956=CARTESIAN_POINT('Ctrl Pts',(-1.03608074678008,1.,-3.77545283140427));
#56957=CARTESIAN_POINT('Ctrl Pts',(-1.04003862055798,1.,-3.7818353500817));
#56958=CARTESIAN_POINT('Ctrl Pts',(-1.04404924374422,1.,-3.78821910787179));
#56959=CARTESIAN_POINT('Ctrl Pts',(-1.04810913267639,1.,-3.79459440308786));
#56960=CARTESIAN_POINT('Ctrl Pts',(-1.05221457990016,1.,-3.80095039790681));
#56961=CARTESIAN_POINT('Ctrl Pts',(-1.05636266918644,1.,-3.80727913637791));
#56962=CARTESIAN_POINT('Ctrl Pts',(-1.06055206187299,1.,-3.8135786611749));
#56963=CARTESIAN_POINT('Ctrl Pts',(-1.0647824403893,1.,-3.81985083953012));
#56964=CARTESIAN_POINT('Ctrl Pts',(-1.06905413180359,1.,-3.82609989967276));
#56965=CARTESIAN_POINT('Ctrl Pts',(-1.07336766633459,1.,-3.83233071195144));
#56966=CARTESIAN_POINT('Ctrl Pts',(-1.07772335353858,1.,-3.83854714117491));
#56967=CARTESIAN_POINT('Ctrl Pts',(-1.08212087917991,1.,-3.8447504803063));
#56968=CARTESIAN_POINT('Ctrl Pts',(-1.08655950846384,1.,-3.85094025222713));
#56969=CARTESIAN_POINT('Ctrl Pts',(-1.09103825516294,1.,-3.85711487933931));
#56970=CARTESIAN_POINT('Ctrl Pts',(-1.09555606505013,1.,-3.86327241021247));
#56971=CARTESIAN_POINT('Ctrl Pts',(-1.10011198761195,1.,-3.86941120134849));
#56972=CARTESIAN_POINT('Ctrl Pts',(-1.10470536603287,1.,-3.87553067187514));
#56973=CARTESIAN_POINT('Ctrl Pts',(-1.10933577224008,1.,-3.88163105531724));
#56974=CARTESIAN_POINT('Ctrl Pts',(-1.11400292434429,1.,-3.88771308285171));
#56975=CARTESIAN_POINT('Ctrl Pts',(-1.11870660794603,1.,-3.89377768340344));
#56976=CARTESIAN_POINT('Ctrl Pts',(-1.12344660099043,1.,-3.89982569750025));
#56977=CARTESIAN_POINT('Ctrl Pts',(-1.12822258281553,1.,-3.90585753318737));
#56978=CARTESIAN_POINT('Ctrl Pts',(-1.13303414693896,1.,-3.91187321145649));
#56979=CARTESIAN_POINT('Ctrl Pts',(-1.13788084225554,1.,-3.91787251936827));
#56980=CARTESIAN_POINT('Ctrl Pts',(-1.14276220561593,1.,-3.92385513133997));
#56981=CARTESIAN_POINT('Ctrl Pts',(-1.14767779451123,1.,-3.92982073294257));
#56982=CARTESIAN_POINT('Ctrl Pts',(-1.1526272271632,1.,-3.9357691705628));
#56983=CARTESIAN_POINT('Ctrl Pts',(-1.15761018340956,1.,-3.94170046685203));
#56984=CARTESIAN_POINT('Ctrl Pts',(-1.16262637999157,1.,-3.94761474780583));
#56985=CARTESIAN_POINT('Ctrl Pts',(-1.16767555244438,1.,-3.95351219509876));
#56986=CARTESIAN_POINT('Ctrl Pts',(-1.17275743590361,1.,-3.95939299213276));
#56987=CARTESIAN_POINT('Ctrl Pts',(-1.17787174135592,1.,-3.96525726358159));
#56988=CARTESIAN_POINT('Ctrl Pts',(-1.18301815039831,1.,-3.97110505165415));
#56989=CARTESIAN_POINT('Ctrl Pts',(-1.18819633715539,1.,-3.97693634767754));
#56990=CARTESIAN_POINT('Ctrl Pts',(-1.19340598349475,1.,-3.98275111052561));
#56991=CARTESIAN_POINT('Ctrl Pts',(-1.19864679609566,1.,-3.98854928957189));
#56992=CARTESIAN_POINT('Ctrl Pts',(-1.20391852375139,1.,-3.99433084799666));
#56993=CARTESIAN_POINT('Ctrl Pts',(-1.20922097029551,1.,-4.00009577950721));
#56994=CARTESIAN_POINT('Ctrl Pts',(-1.21455398918133,1.,-4.00584409522722));
#56995=CARTESIAN_POINT('Ctrl Pts',(-1.21884478244403,1.,-4.01042947140789));
#56996=CARTESIAN_POINT('Ctrl Pts',(-1.22207656455845,1.,-4.01386104433519));
#56997=CARTESIAN_POINT('Ctrl Pts',(-1.22423716681317,1.,-4.01614544569895));
#56998=CARTESIAN_POINT('Ctrl Pts',(-1.22531898815164,1.,-4.01728681790024));
#56999=CARTESIAN_POINT('Origin',(-1.22531898815164,0.,-4.01728681790024));
#57000=CARTESIAN_POINT('',(-1.36999806084572,1.,-3.97027773754922));
#57001=CARTESIAN_POINT('Origin',(0.,0.,0.));
#57002=CARTESIAN_POINT('',(-0.786422660833743,1.,-3.66661143271648));
#57003=CARTESIAN_POINT('Origin',(0.,1.,0.));
#57004=CARTESIAN_POINT('Ctrl Pts',(-0.786422660833742,1.,-3.66661143271648));
#57005=CARTESIAN_POINT('Ctrl Pts',(-0.786422660833742,0.666666666666667,
-3.66661143271648));
#57006=CARTESIAN_POINT('Ctrl Pts',(-0.786422660833742,0.333333333333333,
-3.66661143271648));
#57007=CARTESIAN_POINT('Ctrl Pts',(-0.786422660833742,-0.333333333333333,
-3.66661143271648));
#57008=CARTESIAN_POINT('Ctrl Pts',(-0.786422660833742,-0.666666666666667,
-3.66661143271648));
#57009=CARTESIAN_POINT('Ctrl Pts',(-0.786422660833742,-1.,-3.66661143271648));
#57010=CARTESIAN_POINT('Ctrl Pts',(-0.732042837400619,-1.,-4.13571194405636));
#57011=CARTESIAN_POINT('Ctrl Pts',(-0.732042837400619,1.,-4.13571194405636));
#57012=CARTESIAN_POINT('Ctrl Pts',(-0.732488575135926,-1.,-4.13420383737278));
#57013=CARTESIAN_POINT('Ctrl Pts',(-0.732488575135926,1.,-4.13420383737278));
#57014=CARTESIAN_POINT('Ctrl Pts',(-0.733376589325634,-1.,-4.13118752796397));
#57015=CARTESIAN_POINT('Ctrl Pts',(-0.733376589325634,1.,-4.13118752796397));
#57016=CARTESIAN_POINT('Ctrl Pts',(-0.734698226767512,-1.,-4.12666277572794));
#57017=CARTESIAN_POINT('Ctrl Pts',(-0.734698226767512,1.,-4.12666277572794));
#57018=CARTESIAN_POINT('Ctrl Pts',(-0.736439634335347,-1.,-4.12062919626082));
#57019=CARTESIAN_POINT('Ctrl Pts',(-0.736439634335347,1.,-4.12062919626082));
#57020=CARTESIAN_POINT('Ctrl Pts',(-0.738581708229119,-1.,-4.11308626953795));
#57021=CARTESIAN_POINT('Ctrl Pts',(-0.738581708229119,1.,-4.11308626953795));
#57022=CARTESIAN_POINT('Ctrl Pts',(-0.740688998555152,-1.,-4.1055424175856));
#57023=CARTESIAN_POINT('Ctrl Pts',(-0.740688998555152,1.,-4.1055424175856));
#57024=CARTESIAN_POINT('Ctrl Pts',(-0.742761369690018,-1.,-4.09799769702712));
#57025=CARTESIAN_POINT('Ctrl Pts',(-0.742761369690018,1.,-4.09799769702712));
#57026=CARTESIAN_POINT('Ctrl Pts',(-0.744798649705514,-1.,-4.09045220253011));
#57027=CARTESIAN_POINT('Ctrl Pts',(-0.744798649705514,1.,-4.09045220253011));
#57028=CARTESIAN_POINT('Ctrl Pts',(-0.746800631490822,-1.,-4.08290608094789));
#57029=CARTESIAN_POINT('Ctrl Pts',(-0.746800631490822,1.,-4.08290608094789));
#57030=CARTESIAN_POINT('Ctrl Pts',(-0.748767076679177,-1.,-4.07535951055363));
#57031=CARTESIAN_POINT('Ctrl Pts',(-0.748767076679177,1.,-4.07535951055363));
#57032=CARTESIAN_POINT('Ctrl Pts',(-0.750697720483176,-1.,-4.06781267241886));
#57033=CARTESIAN_POINT('Ctrl Pts',(-0.750697720483176,1.,-4.06781267241886));
#57034=CARTESIAN_POINT('Ctrl Pts',(-0.752592276482869,-1.,-4.06026572221399));
#57035=CARTESIAN_POINT('Ctrl Pts',(-0.752592276482869,1.,-4.06026572221399));
#57036=CARTESIAN_POINT('Ctrl Pts',(-0.754450441816412,-1.,-4.05271876688106));
#57037=CARTESIAN_POINT('Ctrl Pts',(-0.754450441816412,1.,-4.05271876688106));
#57038=CARTESIAN_POINT('Ctrl Pts',(-0.756271902370187,-1.,-4.04517182654344));
#57039=CARTESIAN_POINT('Ctrl Pts',(-0.756271902370187,1.,-4.04517182654344));
#57040=CARTESIAN_POINT('Ctrl Pts',(-0.758056338885554,-1.,-4.03762485803468));
#57041=CARTESIAN_POINT('Ctrl Pts',(-0.758056338885554,1.,-4.03762485803468));
#57042=CARTESIAN_POINT('Ctrl Pts',(-0.759803433244166,-1.,-4.0300778195465));
#57043=CARTESIAN_POINT('Ctrl Pts',(-0.759803433244166,1.,-4.0300778195465));
#57044=CARTESIAN_POINT('Ctrl Pts',(-0.761512875859942,-1.,-4.02253072741347));
#57045=CARTESIAN_POINT('Ctrl Pts',(-0.761512875859942,1.,-4.02253072741347));
#57046=CARTESIAN_POINT('Ctrl Pts',(-0.763184371182827,-1.,-4.01498370680434));
#57047=CARTESIAN_POINT('Ctrl Pts',(-0.763184371182827,1.,-4.01498370680434));
#57048=CARTESIAN_POINT('Ctrl Pts',(-0.764817648784946,-1.,-4.00743706791366));
#57049=CARTESIAN_POINT('Ctrl Pts',(-0.764817648784946,1.,-4.00743706791366));
#57050=CARTESIAN_POINT('Ctrl Pts',(-0.766412457135786,-1.,-3.99989129179464));
#57051=CARTESIAN_POINT('Ctrl Pts',(-0.766412457135786,1.,-3.99989129179464));
#57052=CARTESIAN_POINT('Ctrl Pts',(-0.767968531377708,-1.,-3.99234687880892));
#57053=CARTESIAN_POINT('Ctrl Pts',(-0.767968531377708,1.,-3.99234687880892));
#57054=CARTESIAN_POINT('Ctrl Pts',(-0.769485566245459,-1.,-3.98480422348403));
#57055=CARTESIAN_POINT('Ctrl Pts',(-0.769485566245459,1.,-3.98480422348403));
#57056=CARTESIAN_POINT('Ctrl Pts',(-0.770963190030504,-1.,-3.97726349165507));
#57057=CARTESIAN_POINT('Ctrl Pts',(-0.770963190030504,1.,-3.97726349165507));
#57058=CARTESIAN_POINT('Ctrl Pts',(-0.772400931772239,-1.,-3.96972446532832));
#57059=CARTESIAN_POINT('Ctrl Pts',(-0.772400931772239,1.,-3.96972446532832));
#57060=CARTESIAN_POINT('Ctrl Pts',(-0.773798212026683,-1.,-3.96218649639876));
#57061=CARTESIAN_POINT('Ctrl Pts',(-0.773798212026683,1.,-3.96218649639876));
#57062=CARTESIAN_POINT('Ctrl Pts',(-0.775154418039441,-1.,-3.95464885452364));
#57063=CARTESIAN_POINT('Ctrl Pts',(-0.775154418039441,1.,-3.95464885452364));
#57064=CARTESIAN_POINT('Ctrl Pts',(-0.77646896669796,-1.,-3.94711101619471));
#57065=CARTESIAN_POINT('Ctrl Pts',(-0.77646896669796,1.,-3.94711101619471));
#57066=CARTESIAN_POINT('Ctrl Pts',(-0.77774137056855,-1.,-3.93957296768098));
#57067=CARTESIAN_POINT('Ctrl Pts',(-0.77774137056855,1.,-3.93957296768098));
#57068=CARTESIAN_POINT('Ctrl Pts',(-0.778971308134786,-1.,-3.93203552473153));
#57069=CARTESIAN_POINT('Ctrl Pts',(-0.778971308134786,1.,-3.93203552473153));
#57070=CARTESIAN_POINT('Ctrl Pts',(-0.780158678615507,-1.,-3.92450058323799));
#57071=CARTESIAN_POINT('Ctrl Pts',(-0.780158678615507,1.,-3.92450058323799));
#57072=CARTESIAN_POINT('Ctrl Pts',(-0.781303428618344,-1.,-3.9169703605466));
#57073=CARTESIAN_POINT('Ctrl Pts',(-0.781303428618344,1.,-3.9169703605466));
#57074=CARTESIAN_POINT('Ctrl Pts',(-0.782405395622759,-1.,-3.90944671004536));
#57075=CARTESIAN_POINT('Ctrl Pts',(-0.782405395622759,1.,-3.90944671004536));
#57076=CARTESIAN_POINT('Ctrl Pts',(-0.783464141529082,-1.,-3.90193039043971));
#57077=CARTESIAN_POINT('Ctrl Pts',(-0.783464141529082,1.,-3.90193039043971));
#57078=CARTESIAN_POINT('Ctrl Pts',(-0.784478799358336,-1.,-3.89442039235105));
#57079=CARTESIAN_POINT('Ctrl Pts',(-0.784478799358336,1.,-3.89442039235105));
#57080=CARTESIAN_POINT('Ctrl Pts',(-0.785447890340723,-1.,-3.88691313167399));
#57081=CARTESIAN_POINT('Ctrl Pts',(-0.785447890340723,1.,-3.88691313167399));
#57082=CARTESIAN_POINT('Ctrl Pts',(-0.786369675812592,-1.,-3.87940402818186));
#57083=CARTESIAN_POINT('Ctrl Pts',(-0.786369675812592,1.,-3.87940402818186));
#57084=CARTESIAN_POINT('Ctrl Pts',(-0.78724252761798,-1.,-3.87188916600905));
#57085=CARTESIAN_POINT('Ctrl Pts',(-0.78724252761798,1.,-3.87188916600905));
#57086=CARTESIAN_POINT('Ctrl Pts',(-0.788065315093771,-1.,-3.86436702561342));
#57087=CARTESIAN_POINT('Ctrl Pts',(-0.788065315093771,1.,-3.86436702561342));
#57088=CARTESIAN_POINT('Ctrl Pts',(-0.788837734090688,-1.,-3.85683995872536));
#57089=CARTESIAN_POINT('Ctrl Pts',(-0.788837734090688,1.,-3.85683995872536));
#57090=CARTESIAN_POINT('Ctrl Pts',(-0.789560798155619,-1.,-3.8493163780891));
#57091=CARTESIAN_POINT('Ctrl Pts',(-0.789560798155619,1.,-3.8493163780891));
#57092=CARTESIAN_POINT('Ctrl Pts',(-0.790236124191289,-1.,-3.84180762342476));
#57093=CARTESIAN_POINT('Ctrl Pts',(-0.790236124191289,1.,-3.84180762342476));
#57094=CARTESIAN_POINT('Ctrl Pts',(-0.79086501270534,-1.,-3.83432392054804));
#57095=CARTESIAN_POINT('Ctrl Pts',(-0.79086501270534,1.,-3.83432392054804));
#57096=CARTESIAN_POINT('Ctrl Pts',(-0.791447528662381,-1.,-3.82687033899799));
#57097=CARTESIAN_POINT('Ctrl Pts',(-0.791447528662381,1.,-3.82687033899799));
#57098=CARTESIAN_POINT('Ctrl Pts',(-0.791981740718606,-1.,-3.81944345442237));
#57099=CARTESIAN_POINT('Ctrl Pts',(-0.791981740718606,1.,-3.81944345442237));
#57100=CARTESIAN_POINT('Ctrl Pts',(-0.792462483517568,-1.,-3.81202588694726));
#57101=CARTESIAN_POINT('Ctrl Pts',(-0.792462483517568,1.,-3.81202588694726));
#57102=CARTESIAN_POINT('Ctrl Pts',(-0.792882695234693,-1.,-3.80459229925598));
#57103=CARTESIAN_POINT('Ctrl Pts',(-0.792882695234693,1.,-3.80459229925598));
#57104=CARTESIAN_POINT('Ctrl Pts',(-0.7932356129732,-1.,-3.79711921389862));
#57105=CARTESIAN_POINT('Ctrl Pts',(-0.7932356129732,1.,-3.79711921389862));
#57106=CARTESIAN_POINT('Ctrl Pts',(-0.793516871680966,-1.,-3.78959439439222));
#57107=CARTESIAN_POINT('Ctrl Pts',(-0.793516871680966,1.,-3.78959439439222));
#57108=CARTESIAN_POINT('Ctrl Pts',(-0.793726235781339,-1.,-3.78202460377617));
#57109=CARTESIAN_POINT('Ctrl Pts',(-0.793726235781339,1.,-3.78202460377617));
#57110=CARTESIAN_POINT('Ctrl Pts',(-0.793870523787515,-1.,-3.77444863801264));
#57111=CARTESIAN_POINT('Ctrl Pts',(-0.793870523787515,1.,-3.77444863801264));
#57112=CARTESIAN_POINT('Ctrl Pts',(-0.793961083689141,-1.,-3.76692626931184));
#57113=CARTESIAN_POINT('Ctrl Pts',(-0.793961083689141,1.,-3.76692626931184));
#57114=CARTESIAN_POINT('Ctrl Pts',(-0.794008429135047,-1.,-3.75951468666325));
#57115=CARTESIAN_POINT('Ctrl Pts',(-0.794008429135047,1.,-3.75951468666325));
#57116=CARTESIAN_POINT('Ctrl Pts',(-0.794017347371441,-1.,-3.75224692493895));
#57117=CARTESIAN_POINT('Ctrl Pts',(-0.794017347371441,1.,-3.75224692493895));
#57118=CARTESIAN_POINT('Ctrl Pts',(-0.79398270045988,-1.,-3.74511357728827));
#57119=CARTESIAN_POINT('Ctrl Pts',(-0.79398270045988,1.,-3.74511357728827));
#57120=CARTESIAN_POINT('Ctrl Pts',(-0.79388270093679,-1.,-3.73803280541576));
#57121=CARTESIAN_POINT('Ctrl Pts',(-0.79388270093679,1.,-3.73803280541576));
#57122=CARTESIAN_POINT('Ctrl Pts',(-0.793682750269347,-1.,-3.7308691469564));
#57123=CARTESIAN_POINT('Ctrl Pts',(-0.793682750269347,1.,-3.7308691469564));
#57124=CARTESIAN_POINT('Ctrl Pts',(-0.79334702378387,-1.,-3.7234879729357));
#57125=CARTESIAN_POINT('Ctrl Pts',(-0.79334702378387,1.,-3.7234879729357));
#57126=CARTESIAN_POINT('Ctrl Pts',(-0.792848377370115,-1.,-3.7158024239604));
#57127=CARTESIAN_POINT('Ctrl Pts',(-0.792848377370115,1.,-3.7158024239604));
#57128=CARTESIAN_POINT('Ctrl Pts',(-0.792177688845968,-1.,-3.70781724021879));
#57129=CARTESIAN_POINT('Ctrl Pts',(-0.792177688845968,1.,-3.70781724021879));
#57130=CARTESIAN_POINT('Ctrl Pts',(-0.791356575696509,-1.,-3.69968940808982));
#57131=CARTESIAN_POINT('Ctrl Pts',(-0.791356575696509,1.,-3.69968940808982));
#57132=CARTESIAN_POINT('Ctrl Pts',(-0.79043628498958,-1.,-3.69172044327754));
#57133=CARTESIAN_POINT('Ctrl Pts',(-0.79043628498958,1.,-3.69172044327754));
#57134=CARTESIAN_POINT('Ctrl Pts',(-0.789483546065158,-1.,-3.68428439784285));
#57135=CARTESIAN_POINT('Ctrl Pts',(-0.789483546065158,1.,-3.68428439784285));
#57136=CARTESIAN_POINT('Ctrl Pts',(-0.788569566220662,-1.,-3.67777119516438));
#57137=CARTESIAN_POINT('Ctrl Pts',(-0.788569566220662,1.,-3.67777119516438));
#57138=CARTESIAN_POINT('Ctrl Pts',(-0.787758799995426,-1.,-3.672529236635));
#57139=CARTESIAN_POINT('Ctrl Pts',(-0.787758799995426,1.,-3.672529236635));
#57140=CARTESIAN_POINT('Ctrl Pts',(-0.787095252589508,-1.,-3.66879484800625));
#57141=CARTESIAN_POINT('Ctrl Pts',(-0.787095252589508,1.,-3.66879484800625));
#57142=CARTESIAN_POINT('Ctrl Pts',(-0.786698783541658,-1.,-3.66710211819938));
#57143=CARTESIAN_POINT('Ctrl Pts',(-0.786698783541658,1.,-3.66710211819938));
#57144=CARTESIAN_POINT('Ctrl Pts',(-0.786480236184947,-1.,-3.66657784454965));
#57145=CARTESIAN_POINT('Ctrl Pts',(-0.786480236184947,1.,-3.66657784454965));
#57146=CARTESIAN_POINT('Ctrl Pts',(-0.786369528183039,-1.,-3.66655932661846));
#57147=CARTESIAN_POINT('Ctrl Pts',(-0.786369528183039,1.,-3.66655932661846));
#57148=CARTESIAN_POINT('Ctrl Pts',(-0.786322922920599,-1.,-3.66663282329846));
#57149=CARTESIAN_POINT('Ctrl Pts',(-0.786322922920599,1.,-3.66663282329846));
#57150=CARTESIAN_POINT('',(-0.732042837400619,1.,-4.13571194405636));
#57151=CARTESIAN_POINT('Ctrl Pts',(-0.732042837400619,1.,-4.13571194405636));
#57152=CARTESIAN_POINT('Ctrl Pts',(-0.732488575135926,1.,-4.13420383737278));
#57153=CARTESIAN_POINT('Ctrl Pts',(-0.733376589325634,1.,-4.13118752796397));
#57154=CARTESIAN_POINT('Ctrl Pts',(-0.734698226767512,1.,-4.12666277572794));
#57155=CARTESIAN_POINT('Ctrl Pts',(-0.736439634335347,1.,-4.12062919626082));
#57156=CARTESIAN_POINT('Ctrl Pts',(-0.738581708229119,1.,-4.11308626953795));
#57157=CARTESIAN_POINT('Ctrl Pts',(-0.740688998555152,1.,-4.1055424175856));
#57158=CARTESIAN_POINT('Ctrl Pts',(-0.742761369690018,1.,-4.09799769702712));
#57159=CARTESIAN_POINT('Ctrl Pts',(-0.744798649705514,1.,-4.09045220253011));
#57160=CARTESIAN_POINT('Ctrl Pts',(-0.746800631490822,1.,-4.08290608094789));
#57161=CARTESIAN_POINT('Ctrl Pts',(-0.748767076679177,1.,-4.07535951055363));
#57162=CARTESIAN_POINT('Ctrl Pts',(-0.750697720483176,1.,-4.06781267241886));
#57163=CARTESIAN_POINT('Ctrl Pts',(-0.752592276482869,1.,-4.06026572221399));
#57164=CARTESIAN_POINT('Ctrl Pts',(-0.754450441816412,1.,-4.05271876688106));
#57165=CARTESIAN_POINT('Ctrl Pts',(-0.756271902370187,1.,-4.04517182654344));
#57166=CARTESIAN_POINT('Ctrl Pts',(-0.758056338885554,1.,-4.03762485803468));
#57167=CARTESIAN_POINT('Ctrl Pts',(-0.759803433244166,1.,-4.0300778195465));
#57168=CARTESIAN_POINT('Ctrl Pts',(-0.761512875859942,1.,-4.02253072741347));
#57169=CARTESIAN_POINT('Ctrl Pts',(-0.763184371182827,1.,-4.01498370680434));
#57170=CARTESIAN_POINT('Ctrl Pts',(-0.764817648784946,1.,-4.00743706791366));
#57171=CARTESIAN_POINT('Ctrl Pts',(-0.766412457135786,1.,-3.99989129179464));
#57172=CARTESIAN_POINT('Ctrl Pts',(-0.767968531377708,1.,-3.99234687880892));
#57173=CARTESIAN_POINT('Ctrl Pts',(-0.769485566245459,1.,-3.98480422348403));
#57174=CARTESIAN_POINT('Ctrl Pts',(-0.770963190030504,1.,-3.97726349165507));
#57175=CARTESIAN_POINT('Ctrl Pts',(-0.772400931772239,1.,-3.96972446532832));
#57176=CARTESIAN_POINT('Ctrl Pts',(-0.773798212026683,1.,-3.96218649639876));
#57177=CARTESIAN_POINT('Ctrl Pts',(-0.775154418039441,1.,-3.95464885452364));
#57178=CARTESIAN_POINT('Ctrl Pts',(-0.77646896669796,1.,-3.94711101619471));
#57179=CARTESIAN_POINT('Ctrl Pts',(-0.77774137056855,1.,-3.93957296768098));
#57180=CARTESIAN_POINT('Ctrl Pts',(-0.778971308134786,1.,-3.93203552473153));
#57181=CARTESIAN_POINT('Ctrl Pts',(-0.780158678615507,1.,-3.92450058323799));
#57182=CARTESIAN_POINT('Ctrl Pts',(-0.781303428618344,1.,-3.9169703605466));
#57183=CARTESIAN_POINT('Ctrl Pts',(-0.782405395622759,1.,-3.90944671004536));
#57184=CARTESIAN_POINT('Ctrl Pts',(-0.783464141529082,1.,-3.90193039043971));
#57185=CARTESIAN_POINT('Ctrl Pts',(-0.784478799358336,1.,-3.89442039235105));
#57186=CARTESIAN_POINT('Ctrl Pts',(-0.785447890340723,1.,-3.88691313167399));
#57187=CARTESIAN_POINT('Ctrl Pts',(-0.786369675812592,1.,-3.87940402818186));
#57188=CARTESIAN_POINT('Ctrl Pts',(-0.78724252761798,1.,-3.87188916600905));
#57189=CARTESIAN_POINT('Ctrl Pts',(-0.788065315093771,1.,-3.86436702561342));
#57190=CARTESIAN_POINT('Ctrl Pts',(-0.788837734090688,1.,-3.85683995872536));
#57191=CARTESIAN_POINT('Ctrl Pts',(-0.789560798155619,1.,-3.8493163780891));
#57192=CARTESIAN_POINT('Ctrl Pts',(-0.790236124191289,1.,-3.84180762342476));
#57193=CARTESIAN_POINT('Ctrl Pts',(-0.79086501270534,1.,-3.83432392054804));
#57194=CARTESIAN_POINT('Ctrl Pts',(-0.791447528662381,1.,-3.82687033899799));
#57195=CARTESIAN_POINT('Ctrl Pts',(-0.791981740718606,1.,-3.81944345442237));
#57196=CARTESIAN_POINT('Ctrl Pts',(-0.792462483517568,1.,-3.81202588694726));
#57197=CARTESIAN_POINT('Ctrl Pts',(-0.792882695234693,1.,-3.80459229925598));
#57198=CARTESIAN_POINT('Ctrl Pts',(-0.7932356129732,1.,-3.79711921389862));
#57199=CARTESIAN_POINT('Ctrl Pts',(-0.793516871680966,1.,-3.78959439439222));
#57200=CARTESIAN_POINT('Ctrl Pts',(-0.793726235781339,1.,-3.78202460377617));
#57201=CARTESIAN_POINT('Ctrl Pts',(-0.793870523787515,1.,-3.77444863801264));
#57202=CARTESIAN_POINT('Ctrl Pts',(-0.793961083689141,1.,-3.76692626931184));
#57203=CARTESIAN_POINT('Ctrl Pts',(-0.794008429135047,1.,-3.75951468666325));
#57204=CARTESIAN_POINT('Ctrl Pts',(-0.794017347371441,1.,-3.75224692493895));
#57205=CARTESIAN_POINT('Ctrl Pts',(-0.79398270045988,1.,-3.74511357728827));
#57206=CARTESIAN_POINT('Ctrl Pts',(-0.79388270093679,1.,-3.73803280541576));
#57207=CARTESIAN_POINT('Ctrl Pts',(-0.793682750269347,1.,-3.7308691469564));
#57208=CARTESIAN_POINT('Ctrl Pts',(-0.79334702378387,1.,-3.7234879729357));
#57209=CARTESIAN_POINT('Ctrl Pts',(-0.792848377370115,1.,-3.7158024239604));
#57210=CARTESIAN_POINT('Ctrl Pts',(-0.792177688845968,1.,-3.70781724021879));
#57211=CARTESIAN_POINT('Ctrl Pts',(-0.791356575696509,1.,-3.69968940808982));
#57212=CARTESIAN_POINT('Ctrl Pts',(-0.79043628498958,1.,-3.69172044327754));
#57213=CARTESIAN_POINT('Ctrl Pts',(-0.789483546065158,1.,-3.68428439784285));
#57214=CARTESIAN_POINT('Ctrl Pts',(-0.788569566220662,1.,-3.67777119516438));
#57215=CARTESIAN_POINT('Ctrl Pts',(-0.787758799995426,1.,-3.672529236635));
#57216=CARTESIAN_POINT('Ctrl Pts',(-0.787145041181589,1.,-3.66907505398769));
#57217=CARTESIAN_POINT('Ctrl Pts',(-0.7867743371985,1.,-3.66743103898844));
#57218=CARTESIAN_POINT('Ctrl Pts',(-0.78656591955989,1.,-3.66680946938396));
#57219=CARTESIAN_POINT('Ctrl Pts',(-0.786459983896781,1.,-3.66664310415236));
#57220=CARTESIAN_POINT('Ctrl Pts',(-0.786422660833743,1.,-3.66661143271648));
#57221=CARTESIAN_POINT('',(-0.732042837400619,0.,-4.13571194405636));
#57222=CARTESIAN_POINT('Ctrl Pts',(-0.385214314776329,-1.,-3.73016218570874));
#57223=CARTESIAN_POINT('Ctrl Pts',(-0.385214314776329,1.,-3.73016218570874));
#57224=CARTESIAN_POINT('Ctrl Pts',(-0.385147278814804,-1.,-3.73010668803185));
#57225=CARTESIAN_POINT('Ctrl Pts',(-0.385147278814804,1.,-3.73010668803185));
#57226=CARTESIAN_POINT('Ctrl Pts',(-0.385047711603887,-1.,-3.73015851028729));
#57227=CARTESIAN_POINT('Ctrl Pts',(-0.385047711603887,1.,-3.73015851028729));
#57228=CARTESIAN_POINT('Ctrl Pts',(-0.385001870183841,-1.,-3.73072465900727));
#57229=CARTESIAN_POINT('Ctrl Pts',(-0.385001870183841,1.,-3.73072465900727));
#57230=CARTESIAN_POINT('Ctrl Pts',(-0.385147887989515,-1.,-3.73245705639337));
#57231=CARTESIAN_POINT('Ctrl Pts',(-0.385147887989515,1.,-3.73245705639337));
#57232=CARTESIAN_POINT('Ctrl Pts',(-0.385670806454744,-1.,-3.73621371845475));
#57233=CARTESIAN_POINT('Ctrl Pts',(-0.385670806454744,1.,-3.73621371845475));
#57234=CARTESIAN_POINT('Ctrl Pts',(-0.386519576222035,-1.,-3.74144965781088));
#57235=CARTESIAN_POINT('Ctrl Pts',(-0.386519576222035,1.,-3.74144965781088));
#57236=CARTESIAN_POINT('Ctrl Pts',(-0.387663020050396,-1.,-3.74792651696269));
#57237=CARTESIAN_POINT('Ctrl Pts',(-0.387663020050396,1.,-3.74792651696269));
#57238=CARTESIAN_POINT('Ctrl Pts',(-0.389054775898251,-1.,-3.75529302894757));
#57239=CARTESIAN_POINT('Ctrl Pts',(-0.389054775898251,1.,-3.75529302894757));
#57240=CARTESIAN_POINT('Ctrl Pts',(-0.390642072979259,-1.,-3.76315635032993));
#57241=CARTESIAN_POINT('Ctrl Pts',(-0.390642072979259,1.,-3.76315635032993));
#57242=CARTESIAN_POINT('Ctrl Pts',(-0.392372786223347,-1.,-3.77114011595892));
#57243=CARTESIAN_POINT('Ctrl Pts',(-0.392372786223347,1.,-3.77114011595892));
#57244=CARTESIAN_POINT('Ctrl Pts',(-0.394202481011595,-1.,-3.77894173114368));
#57245=CARTESIAN_POINT('Ctrl Pts',(-0.394202481011595,1.,-3.77894173114368));
#57246=CARTESIAN_POINT('Ctrl Pts',(-0.396103205335029,-1.,-3.78640521279479));
#57247=CARTESIAN_POINT('Ctrl Pts',(-0.396103205335029,1.,-3.78640521279479));
#57248=CARTESIAN_POINT('Ctrl Pts',(-0.398064818684158,-1.,-3.79352887163457));
#57249=CARTESIAN_POINT('Ctrl Pts',(-0.398064818684158,1.,-3.79352887163457));
#57250=CARTESIAN_POINT('Ctrl Pts',(-0.400088346504727,-1.,-3.80040370384659));
#57251=CARTESIAN_POINT('Ctrl Pts',(-0.400088346504727,1.,-3.80040370384659));
#57252=CARTESIAN_POINT('Ctrl Pts',(-0.402181320148475,-1.,-3.80716881962763));
#57253=CARTESIAN_POINT('Ctrl Pts',(-0.402181320148475,1.,-3.80716881962763));
#57254=CARTESIAN_POINT('Ctrl Pts',(-0.404352694628236,-1.,-3.81396374287762));
#57255=CARTESIAN_POINT('Ctrl Pts',(-0.404352694628236,1.,-3.81396374287762));
#57256=CARTESIAN_POINT('Ctrl Pts',(-0.406607038258906,-1.,-3.82087303913741));
#57257=CARTESIAN_POINT('Ctrl Pts',(-0.406607038258906,1.,-3.82087303913741));
#57258=CARTESIAN_POINT('Ctrl Pts',(-0.408942371447377,-1.,-3.82790724256397));
#57259=CARTESIAN_POINT('Ctrl Pts',(-0.408942371447377,1.,-3.82790724256397));
#57260=CARTESIAN_POINT('Ctrl Pts',(-0.41135303879846,-1.,-3.83503345578645));
#57261=CARTESIAN_POINT('Ctrl Pts',(-0.41135303879846,1.,-3.83503345578645));
#57262=CARTESIAN_POINT('Ctrl Pts',(-0.413831367016727,-1.,-3.84219403994742));
#57263=CARTESIAN_POINT('Ctrl Pts',(-0.413831367016727,1.,-3.84219403994742));
#57264=CARTESIAN_POINT('Ctrl Pts',(-0.41636967805292,-1.,-3.8493286415751));
#57265=CARTESIAN_POINT('Ctrl Pts',(-0.41636967805292,1.,-3.8493286415751));
#57266=CARTESIAN_POINT('Ctrl Pts',(-0.41896246808681,-1.,-3.85639825648031));
#57267=CARTESIAN_POINT('Ctrl Pts',(-0.41896246808681,1.,-3.85639825648031));
#57268=CARTESIAN_POINT('Ctrl Pts',(-0.421607423177576,-1.,-3.86339652542749));
#57269=CARTESIAN_POINT('Ctrl Pts',(-0.421607423177576,1.,-3.86339652542749));
#57270=CARTESIAN_POINT('Ctrl Pts',(-0.424304173195142,-1.,-3.87033643487882));
#57271=CARTESIAN_POINT('Ctrl Pts',(-0.424304173195142,1.,-3.87033643487882));
#57272=CARTESIAN_POINT('Ctrl Pts',(-0.427053541173469,-1.,-3.87724240306609));
#57273=CARTESIAN_POINT('Ctrl Pts',(-0.427053541173469,1.,-3.87724240306609));
#57274=CARTESIAN_POINT('Ctrl Pts',(-0.429856640579734,-1.,-3.88414070943334));
#57275=CARTESIAN_POINT('Ctrl Pts',(-0.429856640579734,1.,-3.88414070943334));
#57276=CARTESIAN_POINT('Ctrl Pts',(-0.432713929544439,-1.,-3.89104947940592));
#57277=CARTESIAN_POINT('Ctrl Pts',(-0.432713929544439,1.,-3.89104947940592));
#57278=CARTESIAN_POINT('Ctrl Pts',(-0.435624629433506,-1.,-3.8979725665544));
#57279=CARTESIAN_POINT('Ctrl Pts',(-0.435624629433506,1.,-3.8979725665544));
#57280=CARTESIAN_POINT('Ctrl Pts',(-0.438587235458233,-1.,-3.90490512938546));
#57281=CARTESIAN_POINT('Ctrl Pts',(-0.438587235458233,1.,-3.90490512938546));
#57282=CARTESIAN_POINT('Ctrl Pts',(-0.441599824524047,-1.,-3.91183704069146));
#57283=CARTESIAN_POINT('Ctrl Pts',(-0.441599824524047,1.,-3.91183704069146));
#57284=CARTESIAN_POINT('Ctrl Pts',(-0.444660430230593,-1.,-3.91875701610721));
#57285=CARTESIAN_POINT('Ctrl Pts',(-0.444660430230593,1.,-3.91875701610721));
#57286=CARTESIAN_POINT('Ctrl Pts',(-0.447767416837297,-1.,-3.92565674143424));
#57287=CARTESIAN_POINT('Ctrl Pts',(-0.447767416837297,1.,-3.92565674143424));
#57288=CARTESIAN_POINT('Ctrl Pts',(-0.450919768356347,-1.,-3.93253407403128));
#57289=CARTESIAN_POINT('Ctrl Pts',(-0.450919768356347,1.,-3.93253407403128));
#57290=CARTESIAN_POINT('Ctrl Pts',(-0.454116879027576,-1.,-3.93939080846298));
#57291=CARTESIAN_POINT('Ctrl Pts',(-0.454116879027576,1.,-3.93939080846298));
#57292=CARTESIAN_POINT('Ctrl Pts',(-0.457358410451674,-1.,-3.94623117206675));
#57293=CARTESIAN_POINT('Ctrl Pts',(-0.457358410451674,1.,-3.94623117206675));
#57294=CARTESIAN_POINT('Ctrl Pts',(-0.460644124429119,-1.,-3.95306005817363));
#57295=CARTESIAN_POINT('Ctrl Pts',(-0.460644124429119,1.,-3.95306005817363));
#57296=CARTESIAN_POINT('Ctrl Pts',(-0.463973722115744,-1.,-3.95988133243543));
#57297=CARTESIAN_POINT('Ctrl Pts',(-0.463973722115744,1.,-3.95988133243543));
#57298=CARTESIAN_POINT('Ctrl Pts',(-0.467346690880672,-1.,-3.96669622273946));
#57299=CARTESIAN_POINT('Ctrl Pts',(-0.467346690880672,1.,-3.96669622273946));
#57300=CARTESIAN_POINT('Ctrl Pts',(-0.470762379613477,-1.,-3.97350414289415));
#57301=CARTESIAN_POINT('Ctrl Pts',(-0.470762379613477,1.,-3.97350414289415));
#57302=CARTESIAN_POINT('Ctrl Pts',(-0.474220061019542,-1.,-3.9803033804443));
#57303=CARTESIAN_POINT('Ctrl Pts',(-0.474220061019542,1.,-3.9803033804443));
#57304=CARTESIAN_POINT('Ctrl Pts',(-0.477718999122033,-1.,-3.98709184306743));
#57305=CARTESIAN_POINT('Ctrl Pts',(-0.477718999122033,1.,-3.98709184306743));
#57306=CARTESIAN_POINT('Ctrl Pts',(-0.481258512209638,-1.,-3.99386775880655));
#57307=CARTESIAN_POINT('Ctrl Pts',(-0.481258512209638,1.,-3.99386775880655));
#57308=CARTESIAN_POINT('Ctrl Pts',(-0.484838042421754,-1.,-4.00063045119234));
#57309=CARTESIAN_POINT('Ctrl Pts',(-0.484838042421754,1.,-4.00063045119234));
#57310=CARTESIAN_POINT('Ctrl Pts',(-0.488457130424531,-1.,-4.0073800839092));
#57311=CARTESIAN_POINT('Ctrl Pts',(-0.488457130424531,1.,-4.0073800839092));
#57312=CARTESIAN_POINT('Ctrl Pts',(-0.492115383417931,-1.,-4.01411733503486));
#57313=CARTESIAN_POINT('Ctrl Pts',(-0.492115383417931,1.,-4.01411733503486));
#57314=CARTESIAN_POINT('Ctrl Pts',(-0.495812444326223,-1.,-4.02084308851813));
#57315=CARTESIAN_POINT('Ctrl Pts',(-0.495812444326223,1.,-4.02084308851813));
#57316=CARTESIAN_POINT('Ctrl Pts',(-0.49954796234089,-1.,-4.0275581398015));
#57317=CARTESIAN_POINT('Ctrl Pts',(-0.49954796234089,1.,-4.0275581398015));
#57318=CARTESIAN_POINT('Ctrl Pts',(-0.503321556915514,-1.,-4.0342628417439));
#57319=CARTESIAN_POINT('Ctrl Pts',(-0.503321556915514,1.,-4.0342628417439));
#57320=CARTESIAN_POINT('Ctrl Pts',(-0.507132823288362,-1.,-4.04095715149074));
#57321=CARTESIAN_POINT('Ctrl Pts',(-0.507132823288362,1.,-4.04095715149074));
#57322=CARTESIAN_POINT('Ctrl Pts',(-0.510981349219174,-1.,-4.04764078815591));
#57323=CARTESIAN_POINT('Ctrl Pts',(-0.510981349219174,1.,-4.04764078815591));
#57324=CARTESIAN_POINT('Ctrl Pts',(-0.514866728193104,-1.,-4.05431335771261));
#57325=CARTESIAN_POINT('Ctrl Pts',(-0.514866728193104,1.,-4.05431335771261));
#57326=CARTESIAN_POINT('Ctrl Pts',(-0.51878857233681,-1.,-4.06097448037934));
#57327=CARTESIAN_POINT('Ctrl Pts',(-0.51878857233681,1.,-4.06097448037934));
#57328=CARTESIAN_POINT('Ctrl Pts',(-0.522746528602768,-1.,-4.06762394471075));
#57329=CARTESIAN_POINT('Ctrl Pts',(-0.522746528602768,1.,-4.06762394471075));
#57330=CARTESIAN_POINT('Ctrl Pts',(-0.526740277227,-1.,-4.07426172299496));
#57331=CARTESIAN_POINT('Ctrl Pts',(-0.526740277227,1.,-4.07426172299496));
#57332=CARTESIAN_POINT('Ctrl Pts',(-0.530769518728075,-1.,-4.08088789536488));
#57333=CARTESIAN_POINT('Ctrl Pts',(-0.530769518728075,1.,-4.08088789536488));
#57334=CARTESIAN_POINT('Ctrl Pts',(-0.534833963476999,-1.,-4.08750259988693));
#57335=CARTESIAN_POINT('Ctrl Pts',(-0.534833963476999,1.,-4.08750259988693));
#57336=CARTESIAN_POINT('Ctrl Pts',(-0.538933321179921,-1.,-4.09410597627116));
#57337=CARTESIAN_POINT('Ctrl Pts',(-0.538933321179921,1.,-4.09410597627116));
#57338=CARTESIAN_POINT('Ctrl Pts',(-0.543067286878457,-1.,-4.10069810244473));
#57339=CARTESIAN_POINT('Ctrl Pts',(-0.543067286878457,1.,-4.10069810244473));
#57340=CARTESIAN_POINT('Ctrl Pts',(-0.54723553948676,-1.,-4.1072789702877));
#57341=CARTESIAN_POINT('Ctrl Pts',(-0.54723553948676,1.,-4.1072789702877));
#57342=CARTESIAN_POINT('Ctrl Pts',(-0.551437758498247,-1.,-4.11384852025578));
#57343=CARTESIAN_POINT('Ctrl Pts',(-0.551437758498247,1.,-4.11384852025578));
#57344=CARTESIAN_POINT('Ctrl Pts',(-0.555673636130778,-1.,-4.1204066619623));
#57345=CARTESIAN_POINT('Ctrl Pts',(-0.555673636130778,1.,-4.1204066619623));
#57346=CARTESIAN_POINT('Ctrl Pts',(-0.559942890594628,-1.,-4.12695329951859));
#57347=CARTESIAN_POINT('Ctrl Pts',(-0.559942890594628,1.,-4.12695329951859));
#57348=CARTESIAN_POINT('Ctrl Pts',(-0.564245279535705,-1.,-4.13348835726086));
#57349=CARTESIAN_POINT('Ctrl Pts',(-0.564245279535705,1.,-4.13348835726086));
#57350=CARTESIAN_POINT('Ctrl Pts',(-0.568580610187116,-1.,-4.14001179828669));
#57351=CARTESIAN_POINT('Ctrl Pts',(-0.568580610187116,1.,-4.14001179828669));
#57352=CARTESIAN_POINT('Ctrl Pts',(-0.572948736066277,-1.,-4.14652361065787));
#57353=CARTESIAN_POINT('Ctrl Pts',(-0.572948736066277,1.,-4.14652361065787));
#57354=CARTESIAN_POINT('Ctrl Pts',(-0.576469391673917,-1.,-4.1517237611974));
#57355=CARTESIAN_POINT('Ctrl Pts',(-0.576469391673917,1.,-4.1517237611974));
#57356=CARTESIAN_POINT('Ctrl Pts',(-0.579124568912543,-1.,-4.15561864787379));
#57357=CARTESIAN_POINT('Ctrl Pts',(-0.579124568912543,1.,-4.15561864787379));
#57358=CARTESIAN_POINT('Ctrl Pts',(-0.580901211462913,-1.,-4.15821291712391));
#57359=CARTESIAN_POINT('Ctrl Pts',(-0.580901211462913,1.,-4.15821291712391));
#57360=CARTESIAN_POINT('Ctrl Pts',(-0.581791163835814,-1.,-4.15950947128175));
#57361=CARTESIAN_POINT('Ctrl Pts',(-0.581791163835814,1.,-4.15950947128175));
#57362=CARTESIAN_POINT('',(-0.385112848332548,1.,-3.73017266276632));
#57363=CARTESIAN_POINT('Ctrl Pts',(-0.385112848332549,-1.,-3.73017266276632));
#57364=CARTESIAN_POINT('Ctrl Pts',(-0.385112848332549,-0.666666666666667,
-3.73017266276632));
#57365=CARTESIAN_POINT('Ctrl Pts',(-0.385112848332549,-0.333333333333333,
-3.73017266276632));
#57366=CARTESIAN_POINT('Ctrl Pts',(-0.385112848332549,0.333333333333333,
-3.73017266276632));
#57367=CARTESIAN_POINT('Ctrl Pts',(-0.385112848332549,0.666666666666667,
-3.73017266276632));
#57368=CARTESIAN_POINT('Ctrl Pts',(-0.385112848332549,1.,-3.73017266276632));
#57369=CARTESIAN_POINT('',(-0.581791163835814,1.,-4.15950947128175));
#57370=CARTESIAN_POINT('',(-0.581791163835814,0.,-4.15950947128175));
#57371=CARTESIAN_POINT('Ctrl Pts',(-0.385112848332549,1.,-3.73017266276632));
#57372=CARTESIAN_POINT('Ctrl Pts',(-0.385087139001609,1.,-3.73021431755218));
#57373=CARTESIAN_POINT('Ctrl Pts',(-0.385037797882046,1.,-3.73040527620929));
#57374=CARTESIAN_POINT('Ctrl Pts',(-0.385031656499142,1.,-3.731060828624));
#57375=CARTESIAN_POINT('Ctrl Pts',(-0.385187124633965,1.,-3.73273893363318));
#57376=CARTESIAN_POINT('Ctrl Pts',(-0.385670806454744,1.,-3.73621371845475));
#57377=CARTESIAN_POINT('Ctrl Pts',(-0.386519576222035,1.,-3.74144965781088));
#57378=CARTESIAN_POINT('Ctrl Pts',(-0.387663020050396,1.,-3.74792651696269));
#57379=CARTESIAN_POINT('Ctrl Pts',(-0.389054775898251,1.,-3.75529302894757));
#57380=CARTESIAN_POINT('Ctrl Pts',(-0.390642072979259,1.,-3.76315635032993));
#57381=CARTESIAN_POINT('Ctrl Pts',(-0.392372786223347,1.,-3.77114011595892));
#57382=CARTESIAN_POINT('Ctrl Pts',(-0.394202481011595,1.,-3.77894173114368));
#57383=CARTESIAN_POINT('Ctrl Pts',(-0.396103205335029,1.,-3.78640521279479));
#57384=CARTESIAN_POINT('Ctrl Pts',(-0.398064818684158,1.,-3.79352887163457));
#57385=CARTESIAN_POINT('Ctrl Pts',(-0.400088346504727,1.,-3.80040370384659));
#57386=CARTESIAN_POINT('Ctrl Pts',(-0.402181320148475,1.,-3.80716881962763));
#57387=CARTESIAN_POINT('Ctrl Pts',(-0.404352694628236,1.,-3.81396374287762));
#57388=CARTESIAN_POINT('Ctrl Pts',(-0.406607038258906,1.,-3.82087303913741));
#57389=CARTESIAN_POINT('Ctrl Pts',(-0.408942371447377,1.,-3.82790724256397));
#57390=CARTESIAN_POINT('Ctrl Pts',(-0.41135303879846,1.,-3.83503345578645));
#57391=CARTESIAN_POINT('Ctrl Pts',(-0.413831367016727,1.,-3.84219403994742));
#57392=CARTESIAN_POINT('Ctrl Pts',(-0.41636967805292,1.,-3.8493286415751));
#57393=CARTESIAN_POINT('Ctrl Pts',(-0.41896246808681,1.,-3.85639825648031));
#57394=CARTESIAN_POINT('Ctrl Pts',(-0.421607423177576,1.,-3.86339652542749));
#57395=CARTESIAN_POINT('Ctrl Pts',(-0.424304173195142,1.,-3.87033643487882));
#57396=CARTESIAN_POINT('Ctrl Pts',(-0.427053541173469,1.,-3.87724240306609));
#57397=CARTESIAN_POINT('Ctrl Pts',(-0.429856640579734,1.,-3.88414070943334));
#57398=CARTESIAN_POINT('Ctrl Pts',(-0.432713929544439,1.,-3.89104947940592));
#57399=CARTESIAN_POINT('Ctrl Pts',(-0.435624629433506,1.,-3.8979725665544));
#57400=CARTESIAN_POINT('Ctrl Pts',(-0.438587235458233,1.,-3.90490512938546));
#57401=CARTESIAN_POINT('Ctrl Pts',(-0.441599824524047,1.,-3.91183704069146));
#57402=CARTESIAN_POINT('Ctrl Pts',(-0.444660430230593,1.,-3.91875701610721));
#57403=CARTESIAN_POINT('Ctrl Pts',(-0.447767416837297,1.,-3.92565674143424));
#57404=CARTESIAN_POINT('Ctrl Pts',(-0.450919768356347,1.,-3.93253407403128));
#57405=CARTESIAN_POINT('Ctrl Pts',(-0.454116879027576,1.,-3.93939080846298));
#57406=CARTESIAN_POINT('Ctrl Pts',(-0.457358410451674,1.,-3.94623117206675));
#57407=CARTESIAN_POINT('Ctrl Pts',(-0.460644124429119,1.,-3.95306005817363));
#57408=CARTESIAN_POINT('Ctrl Pts',(-0.463973722115744,1.,-3.95988133243543));
#57409=CARTESIAN_POINT('Ctrl Pts',(-0.467346690880672,1.,-3.96669622273946));
#57410=CARTESIAN_POINT('Ctrl Pts',(-0.470762379613477,1.,-3.97350414289415));
#57411=CARTESIAN_POINT('Ctrl Pts',(-0.474220061019542,1.,-3.9803033804443));
#57412=CARTESIAN_POINT('Ctrl Pts',(-0.477718999122033,1.,-3.98709184306743));
#57413=CARTESIAN_POINT('Ctrl Pts',(-0.481258512209638,1.,-3.99386775880655));
#57414=CARTESIAN_POINT('Ctrl Pts',(-0.484838042421754,1.,-4.00063045119234));
#57415=CARTESIAN_POINT('Ctrl Pts',(-0.488457130424531,1.,-4.0073800839092));
#57416=CARTESIAN_POINT('Ctrl Pts',(-0.492115383417931,1.,-4.01411733503486));
#57417=CARTESIAN_POINT('Ctrl Pts',(-0.495812444326223,1.,-4.02084308851813));
#57418=CARTESIAN_POINT('Ctrl Pts',(-0.49954796234089,1.,-4.0275581398015));
#57419=CARTESIAN_POINT('Ctrl Pts',(-0.503321556915514,1.,-4.0342628417439));
#57420=CARTESIAN_POINT('Ctrl Pts',(-0.507132823288362,1.,-4.04095715149074));
#57421=CARTESIAN_POINT('Ctrl Pts',(-0.510981349219174,1.,-4.04764078815591));
#57422=CARTESIAN_POINT('Ctrl Pts',(-0.514866728193104,1.,-4.05431335771261));
#57423=CARTESIAN_POINT('Ctrl Pts',(-0.51878857233681,1.,-4.06097448037934));
#57424=CARTESIAN_POINT('Ctrl Pts',(-0.522746528602768,1.,-4.06762394471075));
#57425=CARTESIAN_POINT('Ctrl Pts',(-0.526740277227,1.,-4.07426172299496));
#57426=CARTESIAN_POINT('Ctrl Pts',(-0.530769518728075,1.,-4.08088789536488));
#57427=CARTESIAN_POINT('Ctrl Pts',(-0.534833963476999,1.,-4.08750259988693));
#57428=CARTESIAN_POINT('Ctrl Pts',(-0.538933321179921,1.,-4.09410597627116));
#57429=CARTESIAN_POINT('Ctrl Pts',(-0.543067286878457,1.,-4.10069810244473));
#57430=CARTESIAN_POINT('Ctrl Pts',(-0.54723553948676,1.,-4.1072789702877));
#57431=CARTESIAN_POINT('Ctrl Pts',(-0.551437758498247,1.,-4.11384852025578));
#57432=CARTESIAN_POINT('Ctrl Pts',(-0.555673636130778,1.,-4.1204066619623));
#57433=CARTESIAN_POINT('Ctrl Pts',(-0.559942890594628,1.,-4.12695329951859));
#57434=CARTESIAN_POINT('Ctrl Pts',(-0.564245279535705,1.,-4.13348835726086));
#57435=CARTESIAN_POINT('Ctrl Pts',(-0.568580610187116,1.,-4.14001179828669));
#57436=CARTESIAN_POINT('Ctrl Pts',(-0.572948736066277,1.,-4.14652361065787));
#57437=CARTESIAN_POINT('Ctrl Pts',(-0.576469391673917,1.,-4.1517237611974));
#57438=CARTESIAN_POINT('Ctrl Pts',(-0.579124568912543,1.,-4.15561864787379));
#57439=CARTESIAN_POINT('Ctrl Pts',(-0.580901211462913,1.,-4.15821291712391));
#57440=CARTESIAN_POINT('Ctrl Pts',(-0.581791163835814,1.,-4.15950947128175));
#57441=CARTESIAN_POINT('Origin',(-0.581791163835814,0.,-4.15950947128175));
#57442=CARTESIAN_POINT('',(-0.732042837400619,1.,-4.13571194405636));
#57443=CARTESIAN_POINT('Origin',(0.,0.,0.));
#57444=CARTESIAN_POINT('',(-0.203156094897896,1.,-3.74449296982994));
#57445=CARTESIAN_POINT('Origin',(0.,1.,0.));
#57446=CARTESIAN_POINT('Ctrl Pts',(-0.203156094897896,1.,-3.74449296982994));
#57447=CARTESIAN_POINT('Ctrl Pts',(-0.203156094897896,0.666666666666667,
-3.74449296982994));
#57448=CARTESIAN_POINT('Ctrl Pts',(-0.203156094897896,0.333333333333333,
-3.74449296982994));
#57449=CARTESIAN_POINT('Ctrl Pts',(-0.203156094897896,-0.333333333333333,
-3.74449296982994));
#57450=CARTESIAN_POINT('Ctrl Pts',(-0.203156094897896,-0.666666666666667,
-3.74449296982994));
#57451=CARTESIAN_POINT('Ctrl Pts',(-0.203156094897896,-1.,-3.74449296982994));
#57452=CARTESIAN_POINT('Ctrl Pts',(-0.0760622897878238,-1.,-4.19931119685982));
#57453=CARTESIAN_POINT('Ctrl Pts',(-0.0760622897878238,1.,-4.19931119685982));
#57454=CARTESIAN_POINT('Ctrl Pts',(-0.0767384596142197,-1.,-4.19789138621624));
#57455=CARTESIAN_POINT('Ctrl Pts',(-0.0767384596142197,1.,-4.19789138621624));
#57456=CARTESIAN_POINT('Ctrl Pts',(-0.0780873956244405,-1.,-4.19505112860624));
#57457=CARTESIAN_POINT('Ctrl Pts',(-0.0780873956244405,1.,-4.19505112860624));
#57458=CARTESIAN_POINT('Ctrl Pts',(-0.0801005887117605,-1.,-4.19078883322483));
#57459=CARTESIAN_POINT('Ctrl Pts',(-0.0801005887117605,1.,-4.19078883322483));
#57460=CARTESIAN_POINT('Ctrl Pts',(-0.0827644164389512,-1.,-4.1851019532944));
#57461=CARTESIAN_POINT('Ctrl Pts',(-0.0827644164389512,1.,-4.1851019532944));
#57462=CARTESIAN_POINT('Ctrl Pts',(-0.0860600915552517,-1.,-4.17798698669991));
#57463=CARTESIAN_POINT('Ctrl Pts',(-0.0860600915552517,1.,-4.17798698669991));
#57464=CARTESIAN_POINT('Ctrl Pts',(-0.089321556085033,-1.,-4.17086566491823));
#57465=CARTESIAN_POINT('Ctrl Pts',(-0.089321556085033,1.,-4.17086566491823));
#57466=CARTESIAN_POINT('Ctrl Pts',(-0.0925486672167692,-1.,-4.16373802265942));
#57467=CARTESIAN_POINT('Ctrl Pts',(-0.0925486672167692,1.,-4.16373802265942));
#57468=CARTESIAN_POINT('Ctrl Pts',(-0.095741240329707,-1.,-4.15660412653006));
#57469=CARTESIAN_POINT('Ctrl Pts',(-0.095741240329707,1.,-4.15660412653006));
#57470=CARTESIAN_POINT('Ctrl Pts',(-0.0988990478899814,-1.,-4.1494640891762));
#57471=CARTESIAN_POINT('Ctrl Pts',(-0.0988990478899814,1.,-4.1494640891762));
#57472=CARTESIAN_POINT('Ctrl Pts',(-0.102021826577454,-1.,-4.14231804938737));
#57473=CARTESIAN_POINT('Ctrl Pts',(-0.102021826577454,1.,-4.14231804938737));
#57474=CARTESIAN_POINT('Ctrl Pts',(-0.105109286538864,-1.,-4.13516614458396));
#57475=CARTESIAN_POINT('Ctrl Pts',(-0.105109286538864,1.,-4.13516614458396));
#57476=CARTESIAN_POINT('Ctrl Pts',(-0.10816112052835,-1.,-4.12800848371386));
#57477=CARTESIAN_POINT('Ctrl Pts',(-0.10816112052835,1.,-4.12800848371386));
#57478=CARTESIAN_POINT('Ctrl Pts',(-0.111177012683377,-1.,-4.12084512502444));
#57479=CARTESIAN_POINT('Ctrl Pts',(-0.111177012683377,1.,-4.12084512502444));
#57480=CARTESIAN_POINT('Ctrl Pts',(-0.114156649609602,-1.,-4.11367603925313));
#57481=CARTESIAN_POINT('Ctrl Pts',(-0.114156649609602,1.,-4.11367603925313));
#57482=CARTESIAN_POINT('Ctrl Pts',(-0.117099722731705,-1.,-4.10650113382187));
#57483=CARTESIAN_POINT('Ctrl Pts',(-0.117099722731705,1.,-4.10650113382187));
#57484=CARTESIAN_POINT('Ctrl Pts',(-0.120005924388162,-1.,-4.09932031767243));
#57485=CARTESIAN_POINT('Ctrl Pts',(-0.120005924388162,1.,-4.09932031767243));
#57486=CARTESIAN_POINT('Ctrl Pts',(-0.122874946249119,-1.,-4.09213355850836));
#57487=CARTESIAN_POINT('Ctrl Pts',(-0.122874946249119,1.,-4.09213355850836));
#57488=CARTESIAN_POINT('Ctrl Pts',(-0.125706476822529,-1.,-4.08494093372315));
#57489=CARTESIAN_POINT('Ctrl Pts',(-0.125706476822529,1.,-4.08494093372315));
#57490=CARTESIAN_POINT('Ctrl Pts',(-0.128500200484814,-1.,-4.07774270738809));
#57491=CARTESIAN_POINT('Ctrl Pts',(-0.128500200484814,1.,-4.07774270738809));
#57492=CARTESIAN_POINT('Ctrl Pts',(-0.131255793548914,-1.,-4.07053931528579));
#57493=CARTESIAN_POINT('Ctrl Pts',(-0.131255793548914,1.,-4.07053931528579));
#57494=CARTESIAN_POINT('Ctrl Pts',(-0.133972916144225,-1.,-4.06333121018476));
#57495=CARTESIAN_POINT('Ctrl Pts',(-0.133972916144225,1.,-4.06333121018476));
#57496=CARTESIAN_POINT('Ctrl Pts',(-0.136651205046111,-1.,-4.05611873400122));
#57497=CARTESIAN_POINT('Ctrl Pts',(-0.136651205046111,1.,-4.05611873400122));
#57498=CARTESIAN_POINT('Ctrl Pts',(-0.13929026718006,-1.,-4.04890199238056));
#57499=CARTESIAN_POINT('Ctrl Pts',(-0.13929026718006,1.,-4.04890199238056));
#57500=CARTESIAN_POINT('Ctrl Pts',(-0.141889671485508,-1.,-4.04168069633842));
#57501=CARTESIAN_POINT('Ctrl Pts',(-0.141889671485508,1.,-4.04168069633842));
#57502=CARTESIAN_POINT('Ctrl Pts',(-0.144448947038352,-1.,-4.03445411510403));
#57503=CARTESIAN_POINT('Ctrl Pts',(-0.144448947038352,1.,-4.03445411510403));
#57504=CARTESIAN_POINT('Ctrl Pts',(-0.146967602878999,-1.,-4.02722143147048));
#57505=CARTESIAN_POINT('Ctrl Pts',(-0.146967602878999,1.,-4.02722143147048));
#57506=CARTESIAN_POINT('Ctrl Pts',(-0.149445144968708,-1.,-4.01998203715588));
#57507=CARTESIAN_POINT('Ctrl Pts',(-0.149445144968708,1.,-4.01998203715588));
#57508=CARTESIAN_POINT('Ctrl Pts',(-0.151881094022909,-1.,-4.01273584234684));
#57509=CARTESIAN_POINT('Ctrl Pts',(-0.151881094022909,1.,-4.01273584234684));
#57510=CARTESIAN_POINT('Ctrl Pts',(-0.15427500487231,-1.,-4.00548360245297));
#57511=CARTESIAN_POINT('Ctrl Pts',(-0.15427500487231,1.,-4.00548360245297));
#57512=CARTESIAN_POINT('Ctrl Pts',(-0.156626481393736,-1.,-3.99822717425869));
#57513=CARTESIAN_POINT('Ctrl Pts',(-0.156626481393736,1.,-3.99822717425869));
#57514=CARTESIAN_POINT('Ctrl Pts',(-0.158935123982796,-1.,-3.99096873945862));
#57515=CARTESIAN_POINT('Ctrl Pts',(-0.158935123982796,1.,-3.99096873945862));
#57516=CARTESIAN_POINT('Ctrl Pts',(-0.161200482186088,-1.,-3.98371010319866));
#57517=CARTESIAN_POINT('Ctrl Pts',(-0.161200482186088,1.,-3.98371010319866));
#57518=CARTESIAN_POINT('Ctrl Pts',(-0.163422004609999,-1.,-3.97645194630944));
#57519=CARTESIAN_POINT('Ctrl Pts',(-0.163422004609999,1.,-3.97645194630944));
#57520=CARTESIAN_POINT('Ctrl Pts',(-0.165598992851098,-1.,-3.9691931362141));
#57521=CARTESIAN_POINT('Ctrl Pts',(-0.165598992851098,1.,-3.9691931362141));
#57522=CARTESIAN_POINT('Ctrl Pts',(-0.167730547023312,-1.,-3.96192990160296));
#57523=CARTESIAN_POINT('Ctrl Pts',(-0.167730547023312,1.,-3.96192990160296));
#57524=CARTESIAN_POINT('Ctrl Pts',(-0.16981566637413,-1.,-3.95465744665263));
#57525=CARTESIAN_POINT('Ctrl Pts',(-0.16981566637413,1.,-3.95465744665263));
#57526=CARTESIAN_POINT('Ctrl Pts',(-0.171853355369233,-1.,-3.94737164900861));
#57527=CARTESIAN_POINT('Ctrl Pts',(-0.171853355369233,1.,-3.94737164900861));
#57528=CARTESIAN_POINT('Ctrl Pts',(-0.173842734974607,-1.,-3.94007083096214));
#57529=CARTESIAN_POINT('Ctrl Pts',(-0.173842734974607,1.,-3.94007083096214));
#57530=CARTESIAN_POINT('Ctrl Pts',(-0.175783136893873,-1.,-3.93275726771049));
#57531=CARTESIAN_POINT('Ctrl Pts',(-0.175783136893873,1.,-3.93275726771049));
#57532=CARTESIAN_POINT('Ctrl Pts',(-0.177674246152328,-1.,-3.92543942697672));
#57533=CARTESIAN_POINT('Ctrl Pts',(-0.177674246152328,1.,-3.92543942697672));
#57534=CARTESIAN_POINT('Ctrl Pts',(-0.179515885822895,-1.,-3.91812876180948));
#57535=CARTESIAN_POINT('Ctrl Pts',(-0.179515885822895,1.,-3.91812876180948));
#57536=CARTESIAN_POINT('Ctrl Pts',(-0.181307740731796,-1.,-3.91083557557193));
#57537=CARTESIAN_POINT('Ctrl Pts',(-0.181307740731796,1.,-3.91083557557193));
#57538=CARTESIAN_POINT('Ctrl Pts',(-0.183049081993193,-1.,-3.90356488555138));
#57539=CARTESIAN_POINT('Ctrl Pts',(-0.183049081993193,1.,-3.90356488555138));
#57540=CARTESIAN_POINT('Ctrl Pts',(-0.184738537728035,-1.,-3.89631300742633));
#57541=CARTESIAN_POINT('Ctrl Pts',(-0.184738537728035,1.,-3.89631300742633));
#57542=CARTESIAN_POINT('Ctrl Pts',(-0.186373724985263,-1.,-3.88906196725817));
#57543=CARTESIAN_POINT('Ctrl Pts',(-0.186373724985263,1.,-3.88906196725817));
#57544=CARTESIAN_POINT('Ctrl Pts',(-0.187951632512663,-1.,-3.88178563496187));
#57545=CARTESIAN_POINT('Ctrl Pts',(-0.187951632512663,1.,-3.88178563496187));
#57546=CARTESIAN_POINT('Ctrl Pts',(-0.189469253358254,-1.,-3.87445976418377));
#57547=CARTESIAN_POINT('Ctrl Pts',(-0.189469253358254,1.,-3.87445976418377));
#57548=CARTESIAN_POINT('Ctrl Pts',(-0.190924190418613,-1.,-3.8670715862477));
#57549=CARTESIAN_POINT('Ctrl Pts',(-0.190924190418613,1.,-3.8670715862477));
#57550=CARTESIAN_POINT('Ctrl Pts',(-0.19231515304498,-1.,-3.85962774407652));
#57551=CARTESIAN_POINT('Ctrl Pts',(-0.19231515304498,1.,-3.85962774407652));
#57552=CARTESIAN_POINT('Ctrl Pts',(-0.193642806777748,-1.,-3.85216762264019));
#57553=CARTESIAN_POINT('Ctrl Pts',(-0.193642806777748,1.,-3.85216762264019));
#57554=CARTESIAN_POINT('Ctrl Pts',(-0.194909009460255,-1.,-3.84475203347052));
#57555=CARTESIAN_POINT('Ctrl Pts',(-0.194909009460255,1.,-3.84475203347052));
#57556=CARTESIAN_POINT('Ctrl Pts',(-0.19611519897189,-1.,-3.83743910616265));
#57557=CARTESIAN_POINT('Ctrl Pts',(-0.19611519897189,1.,-3.83743910616265));
#57558=CARTESIAN_POINT('Ctrl Pts',(-0.197260935827375,-1.,-3.83026221776488));
#57559=CARTESIAN_POINT('Ctrl Pts',(-0.197260935827375,1.,-3.83026221776488));
#57560=CARTESIAN_POINT('Ctrl Pts',(-0.19834261690047,-1.,-3.82321127348981));
#57561=CARTESIAN_POINT('Ctrl Pts',(-0.19834261690047,1.,-3.82321127348981));
#57562=CARTESIAN_POINT('Ctrl Pts',(-0.199351525297396,-1.,-3.81620203429702));
#57563=CARTESIAN_POINT('Ctrl Pts',(-0.199351525297396,1.,-3.81620203429702));
#57564=CARTESIAN_POINT('Ctrl Pts',(-0.20027467943329,-1.,-3.80909529318501));
#57565=CARTESIAN_POINT('Ctrl Pts',(-0.20027467943329,1.,-3.80909529318501));
#57566=CARTESIAN_POINT('Ctrl Pts',(-0.201097756307252,-1.,-3.80175247447171));
#57567=CARTESIAN_POINT('Ctrl Pts',(-0.201097756307252,1.,-3.80175247447171));
#57568=CARTESIAN_POINT('Ctrl Pts',(-0.201807533800799,-1.,-3.79408354187274));
#57569=CARTESIAN_POINT('Ctrl Pts',(-0.201807533800799,1.,-3.79408354187274));
#57570=CARTESIAN_POINT('Ctrl Pts',(-0.202394260512193,-1.,-3.78609175019317));
#57571=CARTESIAN_POINT('Ctrl Pts',(-0.202394260512193,1.,-3.78609175019317));
#57572=CARTESIAN_POINT('Ctrl Pts',(-0.202854729699197,-1.,-3.77793553476879));
#57573=CARTESIAN_POINT('Ctrl Pts',(-0.202854729699197,1.,-3.77793553476879));
#57574=CARTESIAN_POINT('Ctrl Pts',(-0.203192390045337,-1.,-3.76992071595267));
#57575=CARTESIAN_POINT('Ctrl Pts',(-0.203192390045337,1.,-3.76992071595267));
#57576=CARTESIAN_POINT('Ctrl Pts',(-0.203414634707646,-1.,-3.76242717937273));
#57577=CARTESIAN_POINT('Ctrl Pts',(-0.203414634707646,1.,-3.76242717937273));
#57578=CARTESIAN_POINT('Ctrl Pts',(-0.203530796848404,-1.,-3.75585118707924));
#57579=CARTESIAN_POINT('Ctrl Pts',(-0.203530796848404,1.,-3.75585118707924));
#57580=CARTESIAN_POINT('Ctrl Pts',(-0.203550035479097,-1.,-3.75054693397716));
#57581=CARTESIAN_POINT('Ctrl Pts',(-0.203550035479097,1.,-3.75054693397716));
#57582=CARTESIAN_POINT('Ctrl Pts',(-0.20347884453023,-1.,-3.74675472018582));
#57583=CARTESIAN_POINT('Ctrl Pts',(-0.20347884453023,1.,-3.74675472018582));
#57584=CARTESIAN_POINT('Ctrl Pts',(-0.203352057956055,-1.,-3.7450208092684));
#57585=CARTESIAN_POINT('Ctrl Pts',(-0.203352057956055,1.,-3.7450208092684));
#57586=CARTESIAN_POINT('Ctrl Pts',(-0.203218215747895,-1.,-3.74446880195845));
#57587=CARTESIAN_POINT('Ctrl Pts',(-0.203218215747895,1.,-3.74446880195845));
#57588=CARTESIAN_POINT('Ctrl Pts',(-0.20311176758786,-1.,-3.74443319346666));
#57589=CARTESIAN_POINT('Ctrl Pts',(-0.20311176758786,1.,-3.74443319346666));
#57590=CARTESIAN_POINT('Ctrl Pts',(-0.203054238699719,-1.,-3.74449849461127));
#57591=CARTESIAN_POINT('Ctrl Pts',(-0.203054238699719,1.,-3.74449849461127));
#57592=CARTESIAN_POINT('',(-0.0760622897878238,1.,-4.19931119685982));
#57593=CARTESIAN_POINT('Ctrl Pts',(-0.0760622897878238,1.,-4.19931119685982));
#57594=CARTESIAN_POINT('Ctrl Pts',(-0.0767384596142197,1.,-4.19789138621624));
#57595=CARTESIAN_POINT('Ctrl Pts',(-0.0780873956244405,1.,-4.19505112860624));
#57596=CARTESIAN_POINT('Ctrl Pts',(-0.0801005887117605,1.,-4.19078883322483));
#57597=CARTESIAN_POINT('Ctrl Pts',(-0.0827644164389512,1.,-4.1851019532944));
#57598=CARTESIAN_POINT('Ctrl Pts',(-0.0860600915552517,1.,-4.17798698669991));
#57599=CARTESIAN_POINT('Ctrl Pts',(-0.089321556085033,1.,-4.17086566491823));
#57600=CARTESIAN_POINT('Ctrl Pts',(-0.0925486672167692,1.,-4.16373802265942));
#57601=CARTESIAN_POINT('Ctrl Pts',(-0.095741240329707,1.,-4.15660412653006));
#57602=CARTESIAN_POINT('Ctrl Pts',(-0.0988990478899814,1.,-4.1494640891762));
#57603=CARTESIAN_POINT('Ctrl Pts',(-0.102021826577454,1.,-4.14231804938737));
#57604=CARTESIAN_POINT('Ctrl Pts',(-0.105109286538864,1.,-4.13516614458396));
#57605=CARTESIAN_POINT('Ctrl Pts',(-0.10816112052835,1.,-4.12800848371386));
#57606=CARTESIAN_POINT('Ctrl Pts',(-0.111177012683377,1.,-4.12084512502444));
#57607=CARTESIAN_POINT('Ctrl Pts',(-0.114156649609602,1.,-4.11367603925313));
#57608=CARTESIAN_POINT('Ctrl Pts',(-0.117099722731705,1.,-4.10650113382187));
#57609=CARTESIAN_POINT('Ctrl Pts',(-0.120005924388162,1.,-4.09932031767243));
#57610=CARTESIAN_POINT('Ctrl Pts',(-0.122874946249119,1.,-4.09213355850836));
#57611=CARTESIAN_POINT('Ctrl Pts',(-0.125706476822529,1.,-4.08494093372315));
#57612=CARTESIAN_POINT('Ctrl Pts',(-0.128500200484814,1.,-4.07774270738809));
#57613=CARTESIAN_POINT('Ctrl Pts',(-0.131255793548914,1.,-4.07053931528579));
#57614=CARTESIAN_POINT('Ctrl Pts',(-0.133972916144225,1.,-4.06333121018476));
#57615=CARTESIAN_POINT('Ctrl Pts',(-0.136651205046111,1.,-4.05611873400122));
#57616=CARTESIAN_POINT('Ctrl Pts',(-0.13929026718006,1.,-4.04890199238056));
#57617=CARTESIAN_POINT('Ctrl Pts',(-0.141889671485508,1.,-4.04168069633842));
#57618=CARTESIAN_POINT('Ctrl Pts',(-0.144448947038352,1.,-4.03445411510403));
#57619=CARTESIAN_POINT('Ctrl Pts',(-0.146967602878999,1.,-4.02722143147048));
#57620=CARTESIAN_POINT('Ctrl Pts',(-0.149445144968708,1.,-4.01998203715588));
#57621=CARTESIAN_POINT('Ctrl Pts',(-0.151881094022909,1.,-4.01273584234684));
#57622=CARTESIAN_POINT('Ctrl Pts',(-0.15427500487231,1.,-4.00548360245297));
#57623=CARTESIAN_POINT('Ctrl Pts',(-0.156626481393736,1.,-3.99822717425869));
#57624=CARTESIAN_POINT('Ctrl Pts',(-0.158935123982796,1.,-3.99096873945862));
#57625=CARTESIAN_POINT('Ctrl Pts',(-0.161200482186088,1.,-3.98371010319866));
#57626=CARTESIAN_POINT('Ctrl Pts',(-0.163422004609999,1.,-3.97645194630944));
#57627=CARTESIAN_POINT('Ctrl Pts',(-0.165598992851098,1.,-3.9691931362141));
#57628=CARTESIAN_POINT('Ctrl Pts',(-0.167730547023312,1.,-3.96192990160296));
#57629=CARTESIAN_POINT('Ctrl Pts',(-0.16981566637413,1.,-3.95465744665263));
#57630=CARTESIAN_POINT('Ctrl Pts',(-0.171853355369233,1.,-3.94737164900861));
#57631=CARTESIAN_POINT('Ctrl Pts',(-0.173842734974607,1.,-3.94007083096214));
#57632=CARTESIAN_POINT('Ctrl Pts',(-0.175783136893873,1.,-3.93275726771049));
#57633=CARTESIAN_POINT('Ctrl Pts',(-0.177674246152328,1.,-3.92543942697672));
#57634=CARTESIAN_POINT('Ctrl Pts',(-0.179515885822895,1.,-3.91812876180948));
#57635=CARTESIAN_POINT('Ctrl Pts',(-0.181307740731796,1.,-3.91083557557193));
#57636=CARTESIAN_POINT('Ctrl Pts',(-0.183049081993193,1.,-3.90356488555138));
#57637=CARTESIAN_POINT('Ctrl Pts',(-0.184738537728035,1.,-3.89631300742633));
#57638=CARTESIAN_POINT('Ctrl Pts',(-0.186373724985263,1.,-3.88906196725817));
#57639=CARTESIAN_POINT('Ctrl Pts',(-0.187951632512663,1.,-3.88178563496187));
#57640=CARTESIAN_POINT('Ctrl Pts',(-0.189469253358254,1.,-3.87445976418377));
#57641=CARTESIAN_POINT('Ctrl Pts',(-0.190924190418613,1.,-3.8670715862477));
#57642=CARTESIAN_POINT('Ctrl Pts',(-0.19231515304498,1.,-3.85962774407652));
#57643=CARTESIAN_POINT('Ctrl Pts',(-0.193642806777748,1.,-3.85216762264019));
#57644=CARTESIAN_POINT('Ctrl Pts',(-0.194909009460255,1.,-3.84475203347052));
#57645=CARTESIAN_POINT('Ctrl Pts',(-0.19611519897189,1.,-3.83743910616265));
#57646=CARTESIAN_POINT('Ctrl Pts',(-0.197260935827375,1.,-3.83026221776488));
#57647=CARTESIAN_POINT('Ctrl Pts',(-0.19834261690047,1.,-3.82321127348981));
#57648=CARTESIAN_POINT('Ctrl Pts',(-0.199351525297396,1.,-3.81620203429702));
#57649=CARTESIAN_POINT('Ctrl Pts',(-0.20027467943329,1.,-3.80909529318501));
#57650=CARTESIAN_POINT('Ctrl Pts',(-0.201097756307252,1.,-3.80175247447171));
#57651=CARTESIAN_POINT('Ctrl Pts',(-0.201807533800799,1.,-3.79408354187274));
#57652=CARTESIAN_POINT('Ctrl Pts',(-0.202394260512193,1.,-3.78609175019317));
#57653=CARTESIAN_POINT('Ctrl Pts',(-0.202854729699197,1.,-3.77793553476879));
#57654=CARTESIAN_POINT('Ctrl Pts',(-0.203192390045337,1.,-3.76992071595267));
#57655=CARTESIAN_POINT('Ctrl Pts',(-0.203414634707646,1.,-3.76242717937273));
#57656=CARTESIAN_POINT('Ctrl Pts',(-0.203530796848404,1.,-3.75585118707924));
#57657=CARTESIAN_POINT('Ctrl Pts',(-0.203550035479097,1.,-3.75054693397716));
#57658=CARTESIAN_POINT('Ctrl Pts',(-0.203484186269315,1.,-3.74703926501843));
#57659=CARTESIAN_POINT('Ctrl Pts',(-0.203375226874331,1.,-3.74535749969262));
#57660=CARTESIAN_POINT('Ctrl Pts',(-0.203266610111264,1.,-3.74471097893961));
#57661=CARTESIAN_POINT('Ctrl Pts',(-0.203188003947965,1.,-3.74453008995129));
#57662=CARTESIAN_POINT('Ctrl Pts',(-0.203156094897896,1.,-3.74449296982994));
#57663=CARTESIAN_POINT('',(-0.0760622897878238,0.,-4.19931119685982));
#57664=CARTESIAN_POINT('Ctrl Pts',(0.20305423869972,-1.,-3.74449849461127));
#57665=CARTESIAN_POINT('Ctrl Pts',(0.20305423869972,1.,-3.74449849461127));
#57666=CARTESIAN_POINT('Ctrl Pts',(0.203111767587923,-1.,-3.7444331934681));
#57667=CARTESIAN_POINT('Ctrl Pts',(0.203111767587923,1.,-3.7444331934681));
#57668=CARTESIAN_POINT('Ctrl Pts',(0.203218215748058,-1.,-3.7444688019622));
#57669=CARTESIAN_POINT('Ctrl Pts',(0.203218215748058,1.,-3.7444688019622));
#57670=CARTESIAN_POINT('Ctrl Pts',(0.203352057956297,-1.,-3.74502080927395));
#57671=CARTESIAN_POINT('Ctrl Pts',(0.203352057956297,1.,-3.74502080927395));
#57672=CARTESIAN_POINT('Ctrl Pts',(0.203478844530447,-1.,-3.7467547201908));
#57673=CARTESIAN_POINT('Ctrl Pts',(0.203478844530447,1.,-3.7467547201908));
#57674=CARTESIAN_POINT('Ctrl Pts',(0.203550035479166,-1.,-3.75054693397875));
#57675=CARTESIAN_POINT('Ctrl Pts',(0.203550035479166,1.,-3.75054693397875));
#57676=CARTESIAN_POINT('Ctrl Pts',(0.203530796848321,-1.,-3.75585118707734));
#57677=CARTESIAN_POINT('Ctrl Pts',(0.203530796848321,1.,-3.75585118707734));
#57678=CARTESIAN_POINT('Ctrl Pts',(0.203414634707478,-1.,-3.76242717936885));
#57679=CARTESIAN_POINT('Ctrl Pts',(0.203414634707478,1.,-3.76242717936885));
#57680=CARTESIAN_POINT('Ctrl Pts',(0.203192390045164,-1.,-3.7699207159487));
#57681=CARTESIAN_POINT('Ctrl Pts',(0.203192390045164,1.,-3.7699207159487));
#57682=CARTESIAN_POINT('Ctrl Pts',(0.202854729699081,-1.,-3.77793553476614));
#57683=CARTESIAN_POINT('Ctrl Pts',(0.202854729699081,1.,-3.77793553476614));
#57684=CARTESIAN_POINT('Ctrl Pts',(0.20239426051216,-1.,-3.78609175019242));
#57685=CARTESIAN_POINT('Ctrl Pts',(0.20239426051216,1.,-3.78609175019242));
#57686=CARTESIAN_POINT('Ctrl Pts',(0.201807533800837,-1.,-3.7940835418736));
#57687=CARTESIAN_POINT('Ctrl Pts',(0.201807533800837,1.,-3.7940835418736));
#57688=CARTESIAN_POINT('Ctrl Pts',(0.201097756307326,-1.,-3.80175247447337));
#57689=CARTESIAN_POINT('Ctrl Pts',(0.201097756307326,1.,-3.80175247447337));
#57690=CARTESIAN_POINT('Ctrl Pts',(0.200274679433364,-1.,-3.80909529318669));
#57691=CARTESIAN_POINT('Ctrl Pts',(0.200274679433364,1.,-3.80909529318669));
#57692=CARTESIAN_POINT('Ctrl Pts',(0.199351525297447,-1.,-3.81620203429815));
#57693=CARTESIAN_POINT('Ctrl Pts',(0.199351525297447,1.,-3.81620203429815));
#57694=CARTESIAN_POINT('Ctrl Pts',(0.198342616900486,-1.,-3.82321127349016));
#57695=CARTESIAN_POINT('Ctrl Pts',(0.198342616900486,1.,-3.82321127349016));
#57696=CARTESIAN_POINT('Ctrl Pts',(0.197260935827361,-1.,-3.83026221776456));
#57697=CARTESIAN_POINT('Ctrl Pts',(0.197260935827361,1.,-3.83026221776456));
#57698=CARTESIAN_POINT('Ctrl Pts',(0.196115198971859,-1.,-3.83743910616195));
#57699=CARTESIAN_POINT('Ctrl Pts',(0.196115198971859,1.,-3.83743910616195));
#57700=CARTESIAN_POINT('Ctrl Pts',(0.19490900946022,-1.,-3.84475203346977));
#57701=CARTESIAN_POINT('Ctrl Pts',(0.19490900946022,1.,-3.84475203346977));
#57702=CARTESIAN_POINT('Ctrl Pts',(0.193642806777723,-1.,-3.85216762263966));
#57703=CARTESIAN_POINT('Ctrl Pts',(0.193642806777723,1.,-3.85216762263966));
#57704=CARTESIAN_POINT('Ctrl Pts',(0.19231515304497,-1.,-3.85962774407633));
#57705=CARTESIAN_POINT('Ctrl Pts',(0.19231515304497,1.,-3.85962774407633));
#57706=CARTESIAN_POINT('Ctrl Pts',(0.19092419041862,-1.,-3.86707158624783));
#57707=CARTESIAN_POINT('Ctrl Pts',(0.19092419041862,1.,-3.86707158624783));
#57708=CARTESIAN_POINT('Ctrl Pts',(0.189469253358272,-1.,-3.87445976418412));
#57709=CARTESIAN_POINT('Ctrl Pts',(0.189469253358272,1.,-3.87445976418412));
#57710=CARTESIAN_POINT('Ctrl Pts',(0.187951632512685,-1.,-3.88178563496228));
#57711=CARTESIAN_POINT('Ctrl Pts',(0.187951632512685,1.,-3.88178563496228));
#57712=CARTESIAN_POINT('Ctrl Pts',(0.18637372498528,-1.,-3.88906196725848));
#57713=CARTESIAN_POINT('Ctrl Pts',(0.18637372498528,1.,-3.88906196725848));
#57714=CARTESIAN_POINT('Ctrl Pts',(0.184738537728043,-1.,-3.89631300742646));
#57715=CARTESIAN_POINT('Ctrl Pts',(0.184738537728043,1.,-3.89631300742646));
#57716=CARTESIAN_POINT('Ctrl Pts',(0.18304908199319,-1.,-3.90356488555132));
#57717=CARTESIAN_POINT('Ctrl Pts',(0.18304908199319,1.,-3.90356488555132));
#57718=CARTESIAN_POINT('Ctrl Pts',(0.181307740731785,-1.,-3.91083557557175));
#57719=CARTESIAN_POINT('Ctrl Pts',(0.181307740731785,1.,-3.91083557557175));
#57720=CARTESIAN_POINT('Ctrl Pts',(0.179515885822881,-1.,-3.91812876180926));
#57721=CARTESIAN_POINT('Ctrl Pts',(0.179515885822881,1.,-3.91812876180926));
#57722=CARTESIAN_POINT('Ctrl Pts',(0.177674246152317,-1.,-3.92543942697655));
#57723=CARTESIAN_POINT('Ctrl Pts',(0.177674246152317,1.,-3.92543942697655));
#57724=CARTESIAN_POINT('Ctrl Pts',(0.175783136893868,-1.,-3.93275726771042));
#57725=CARTESIAN_POINT('Ctrl Pts',(0.175783136893868,1.,-3.93275726771042));
#57726=CARTESIAN_POINT('Ctrl Pts',(0.173842734974609,-1.,-3.94007083096217));
#57727=CARTESIAN_POINT('Ctrl Pts',(0.173842734974609,1.,-3.94007083096217));
#57728=CARTESIAN_POINT('Ctrl Pts',(0.17185335536924,-1.,-3.94737164900868));
#57729=CARTESIAN_POINT('Ctrl Pts',(0.17185335536924,1.,-3.94737164900868));
#57730=CARTESIAN_POINT('Ctrl Pts',(0.169815666374139,-1.,-3.95465744665268));
#57731=CARTESIAN_POINT('Ctrl Pts',(0.169815666374139,1.,-3.95465744665268));
#57732=CARTESIAN_POINT('Ctrl Pts',(0.167730547023319,-1.,-3.96192990160296));
#57733=CARTESIAN_POINT('Ctrl Pts',(0.167730547023319,1.,-3.96192990160296));
#57734=CARTESIAN_POINT('Ctrl Pts',(0.165598992851102,-1.,-3.96919313621407));
#57735=CARTESIAN_POINT('Ctrl Pts',(0.165598992851102,1.,-3.96919313621407));
#57736=CARTESIAN_POINT('Ctrl Pts',(0.163422004609999,-1.,-3.97645194630943));
#57737=CARTESIAN_POINT('Ctrl Pts',(0.163422004609999,1.,-3.97645194630943));
#57738=CARTESIAN_POINT('Ctrl Pts',(0.161200482186084,-1.,-3.98371010319872));
#57739=CARTESIAN_POINT('Ctrl Pts',(0.161200482186084,1.,-3.98371010319872));
#57740=CARTESIAN_POINT('Ctrl Pts',(0.158935123982793,-1.,-3.99096873945878));
#57741=CARTESIAN_POINT('Ctrl Pts',(0.158935123982793,1.,-3.99096873945878));
#57742=CARTESIAN_POINT('Ctrl Pts',(0.156626481393734,-1.,-3.99822717425893));
#57743=CARTESIAN_POINT('Ctrl Pts',(0.156626481393734,1.,-3.99822717425893));
#57744=CARTESIAN_POINT('Ctrl Pts',(0.15427500487231,-1.,-4.00548360245319));
#57745=CARTESIAN_POINT('Ctrl Pts',(0.15427500487231,1.,-4.00548360245319));
#57746=CARTESIAN_POINT('Ctrl Pts',(0.15188109402291,-1.,-4.01273584234689));
#57747=CARTESIAN_POINT('Ctrl Pts',(0.15188109402291,1.,-4.01273584234689));
#57748=CARTESIAN_POINT('Ctrl Pts',(0.149445144968707,-1.,-4.01998203715564));
#57749=CARTESIAN_POINT('Ctrl Pts',(0.149445144968707,1.,-4.01998203715564));
#57750=CARTESIAN_POINT('Ctrl Pts',(0.146967602878994,-1.,-4.02722143146994));
#57751=CARTESIAN_POINT('Ctrl Pts',(0.146967602878994,1.,-4.02722143146994));
#57752=CARTESIAN_POINT('Ctrl Pts',(0.144448947038344,-1.,-4.03445411510333));
#57753=CARTESIAN_POINT('Ctrl Pts',(0.144448947038344,1.,-4.03445411510333));
#57754=CARTESIAN_POINT('Ctrl Pts',(0.1418896714855,-1.,-4.04168069633781));
#57755=CARTESIAN_POINT('Ctrl Pts',(0.1418896714855,1.,-4.04168069633781));
#57756=CARTESIAN_POINT('Ctrl Pts',(0.139290267180057,-1.,-4.04890199238036));
#57757=CARTESIAN_POINT('Ctrl Pts',(0.139290267180057,1.,-4.04890199238036));
#57758=CARTESIAN_POINT('Ctrl Pts',(0.136651205046119,-1.,-4.05611873400172));
#57759=CARTESIAN_POINT('Ctrl Pts',(0.136651205046119,1.,-4.05611873400172));
#57760=CARTESIAN_POINT('Ctrl Pts',(0.133972916144245,-1.,-4.06333121018596));
#57761=CARTESIAN_POINT('Ctrl Pts',(0.133972916144245,1.,-4.06333121018596));
#57762=CARTESIAN_POINT('Ctrl Pts',(0.13125579354894,-1.,-4.0705393152874));
#57763=CARTESIAN_POINT('Ctrl Pts',(0.13125579354894,1.,-4.0705393152874));
#57764=CARTESIAN_POINT('Ctrl Pts',(0.128500200484837,-1.,-4.07774270738954));
#57765=CARTESIAN_POINT('Ctrl Pts',(0.128500200484837,1.,-4.07774270738954));
#57766=CARTESIAN_POINT('Ctrl Pts',(0.12570647682254,-1.,-4.08494093372377));
#57767=CARTESIAN_POINT('Ctrl Pts',(0.12570647682254,1.,-4.08494093372377));
#57768=CARTESIAN_POINT('Ctrl Pts',(0.122874946249107,-1.,-4.09213355850756));
#57769=CARTESIAN_POINT('Ctrl Pts',(0.122874946249107,1.,-4.09213355850756));
#57770=CARTESIAN_POINT('Ctrl Pts',(0.120005924388124,-1.,-4.09932031767002));
#57771=CARTESIAN_POINT('Ctrl Pts',(0.120005924388124,1.,-4.09932031767002));
#57772=CARTESIAN_POINT('Ctrl Pts',(0.117099722731648,-1.,-4.10650113381833));
#57773=CARTESIAN_POINT('Ctrl Pts',(0.117099722731648,1.,-4.10650113381833));
#57774=CARTESIAN_POINT('Ctrl Pts',(0.114156649609545,-1.,-4.11367603924961));
#57775=CARTESIAN_POINT('Ctrl Pts',(0.114156649609545,1.,-4.11367603924961));
#57776=CARTESIAN_POINT('Ctrl Pts',(0.111177012683346,-1.,-4.1208451250225));
#57777=CARTESIAN_POINT('Ctrl Pts',(0.111177012683346,1.,-4.1208451250225));
#57778=CARTESIAN_POINT('Ctrl Pts',(0.108161120528369,-1.,-4.12800848371504));
#57779=CARTESIAN_POINT('Ctrl Pts',(0.108161120528369,1.,-4.12800848371504));
#57780=CARTESIAN_POINT('Ctrl Pts',(0.105109286538945,-1.,-4.13516614458895));
#57781=CARTESIAN_POINT('Ctrl Pts',(0.105109286538945,1.,-4.13516614458895));
#57782=CARTESIAN_POINT('Ctrl Pts',(0.102021826577584,-1.,-4.14231804939538));
#57783=CARTESIAN_POINT('Ctrl Pts',(0.102021826577584,1.,-4.14231804939538));
#57784=CARTESIAN_POINT('Ctrl Pts',(0.0988990478901223,-1.,-4.14946408918485));
#57785=CARTESIAN_POINT('Ctrl Pts',(0.0988990478901223,1.,-4.14946408918485));
#57786=CARTESIAN_POINT('Ctrl Pts',(0.0957412403298004,-1.,-4.15660412653577));
#57787=CARTESIAN_POINT('Ctrl Pts',(0.0957412403298004,1.,-4.15660412653577));
#57788=CARTESIAN_POINT('Ctrl Pts',(0.0925486672167528,-1.,-4.16373802265839));
#57789=CARTESIAN_POINT('Ctrl Pts',(0.0925486672167528,1.,-4.16373802265839));
#57790=CARTESIAN_POINT('Ctrl Pts',(0.0893215560848647,-1.,-4.17086566490794));
#57791=CARTESIAN_POINT('Ctrl Pts',(0.0893215560848647,1.,-4.17086566490794));
#57792=CARTESIAN_POINT('Ctrl Pts',(0.0860600915549394,-1.,-4.17798698668094));
#57793=CARTESIAN_POINT('Ctrl Pts',(0.0860600915549394,1.,-4.17798698668094));
#57794=CARTESIAN_POINT('Ctrl Pts',(0.0827644164385676,-1.,-4.18510195327123));
#57795=CARTESIAN_POINT('Ctrl Pts',(0.0827644164385676,1.,-4.18510195327123));
#57796=CARTESIAN_POINT('Ctrl Pts',(0.0801005887114317,-1.,-4.19078883320504));
#57797=CARTESIAN_POINT('Ctrl Pts',(0.0801005887114317,1.,-4.19078883320504));
#57798=CARTESIAN_POINT('Ctrl Pts',(0.0780873956242395,-1.,-4.19505112859416));
#57799=CARTESIAN_POINT('Ctrl Pts',(0.0780873956242395,1.,-4.19505112859416));
#57800=CARTESIAN_POINT('Ctrl Pts',(0.0767384596141462,-1.,-4.1978913862118));
#57801=CARTESIAN_POINT('Ctrl Pts',(0.0767384596141462,1.,-4.1978913862118));
#57802=CARTESIAN_POINT('Ctrl Pts',(0.0760622897878244,-1.,-4.19931119685982));
#57803=CARTESIAN_POINT('Ctrl Pts',(0.0760622897878244,1.,-4.19931119685982));
#57804=CARTESIAN_POINT('',(0.203156094896102,1.,-3.74449296983004));
#57805=CARTESIAN_POINT('Ctrl Pts',(0.2031560948961,-1.,-3.74449296983004));
#57806=CARTESIAN_POINT('Ctrl Pts',(0.2031560948961,-0.666666666666667,-3.74449296983004));
#57807=CARTESIAN_POINT('Ctrl Pts',(0.2031560948961,-0.333333333333333,-3.74449296983004));
#57808=CARTESIAN_POINT('Ctrl Pts',(0.2031560948961,0.333333333333333,-3.74449296983004));
#57809=CARTESIAN_POINT('Ctrl Pts',(0.203156094896101,0.666666666666667,
-3.74449296983004));
#57810=CARTESIAN_POINT('Ctrl Pts',(0.203156094896101,1.,-3.74449296983004));
#57811=CARTESIAN_POINT('',(0.0760622897878244,1.,-4.19931119685982));
#57812=CARTESIAN_POINT('',(0.0760622897878244,0.,-4.19931119685982));
#57813=CARTESIAN_POINT('Ctrl Pts',(0.203156094896101,1.,-3.74449296983004));
#57814=CARTESIAN_POINT('Ctrl Pts',(0.203188003946657,1.,-3.74453008995093));
#57815=CARTESIAN_POINT('Ctrl Pts',(0.203266610110531,1.,-3.74471097893845));
#57816=CARTESIAN_POINT('Ctrl Pts',(0.203375226874121,1.,-3.74535749969115));
#57817=CARTESIAN_POINT('Ctrl Pts',(0.203484186269415,1.,-3.74703926501752));
#57818=CARTESIAN_POINT('Ctrl Pts',(0.203550035479166,1.,-3.75054693397875));
#57819=CARTESIAN_POINT('Ctrl Pts',(0.203530796848321,1.,-3.75585118707734));
#57820=CARTESIAN_POINT('Ctrl Pts',(0.203414634707478,1.,-3.76242717936885));
#57821=CARTESIAN_POINT('Ctrl Pts',(0.203192390045164,1.,-3.7699207159487));
#57822=CARTESIAN_POINT('Ctrl Pts',(0.202854729699081,1.,-3.77793553476614));
#57823=CARTESIAN_POINT('Ctrl Pts',(0.20239426051216,1.,-3.78609175019242));
#57824=CARTESIAN_POINT('Ctrl Pts',(0.201807533800837,1.,-3.7940835418736));
#57825=CARTESIAN_POINT('Ctrl Pts',(0.201097756307326,1.,-3.80175247447337));
#57826=CARTESIAN_POINT('Ctrl Pts',(0.200274679433364,1.,-3.80909529318669));
#57827=CARTESIAN_POINT('Ctrl Pts',(0.199351525297447,1.,-3.81620203429815));
#57828=CARTESIAN_POINT('Ctrl Pts',(0.198342616900486,1.,-3.82321127349016));
#57829=CARTESIAN_POINT('Ctrl Pts',(0.197260935827361,1.,-3.83026221776456));
#57830=CARTESIAN_POINT('Ctrl Pts',(0.196115198971859,1.,-3.83743910616195));
#57831=CARTESIAN_POINT('Ctrl Pts',(0.19490900946022,1.,-3.84475203346977));
#57832=CARTESIAN_POINT('Ctrl Pts',(0.193642806777723,1.,-3.85216762263966));
#57833=CARTESIAN_POINT('Ctrl Pts',(0.19231515304497,1.,-3.85962774407633));
#57834=CARTESIAN_POINT('Ctrl Pts',(0.19092419041862,1.,-3.86707158624783));
#57835=CARTESIAN_POINT('Ctrl Pts',(0.189469253358272,1.,-3.87445976418412));
#57836=CARTESIAN_POINT('Ctrl Pts',(0.187951632512685,1.,-3.88178563496228));
#57837=CARTESIAN_POINT('Ctrl Pts',(0.18637372498528,1.,-3.88906196725848));
#57838=CARTESIAN_POINT('Ctrl Pts',(0.184738537728043,1.,-3.89631300742646));
#57839=CARTESIAN_POINT('Ctrl Pts',(0.18304908199319,1.,-3.90356488555132));
#57840=CARTESIAN_POINT('Ctrl Pts',(0.181307740731785,1.,-3.91083557557175));
#57841=CARTESIAN_POINT('Ctrl Pts',(0.179515885822881,1.,-3.91812876180926));
#57842=CARTESIAN_POINT('Ctrl Pts',(0.177674246152317,1.,-3.92543942697655));
#57843=CARTESIAN_POINT('Ctrl Pts',(0.175783136893868,1.,-3.93275726771042));
#57844=CARTESIAN_POINT('Ctrl Pts',(0.173842734974609,1.,-3.94007083096217));
#57845=CARTESIAN_POINT('Ctrl Pts',(0.17185335536924,1.,-3.94737164900868));
#57846=CARTESIAN_POINT('Ctrl Pts',(0.169815666374139,1.,-3.95465744665268));
#57847=CARTESIAN_POINT('Ctrl Pts',(0.167730547023319,1.,-3.96192990160296));
#57848=CARTESIAN_POINT('Ctrl Pts',(0.165598992851102,1.,-3.96919313621407));
#57849=CARTESIAN_POINT('Ctrl Pts',(0.163422004609999,1.,-3.97645194630943));
#57850=CARTESIAN_POINT('Ctrl Pts',(0.161200482186084,1.,-3.98371010319872));
#57851=CARTESIAN_POINT('Ctrl Pts',(0.158935123982793,1.,-3.99096873945878));
#57852=CARTESIAN_POINT('Ctrl Pts',(0.156626481393734,1.,-3.99822717425893));
#57853=CARTESIAN_POINT('Ctrl Pts',(0.15427500487231,1.,-4.00548360245319));
#57854=CARTESIAN_POINT('Ctrl Pts',(0.15188109402291,1.,-4.01273584234689));
#57855=CARTESIAN_POINT('Ctrl Pts',(0.149445144968707,1.,-4.01998203715564));
#57856=CARTESIAN_POINT('Ctrl Pts',(0.146967602878994,1.,-4.02722143146994));
#57857=CARTESIAN_POINT('Ctrl Pts',(0.144448947038344,1.,-4.03445411510333));
#57858=CARTESIAN_POINT('Ctrl Pts',(0.1418896714855,1.,-4.04168069633781));
#57859=CARTESIAN_POINT('Ctrl Pts',(0.139290267180057,1.,-4.04890199238036));
#57860=CARTESIAN_POINT('Ctrl Pts',(0.136651205046119,1.,-4.05611873400172));
#57861=CARTESIAN_POINT('Ctrl Pts',(0.133972916144245,1.,-4.06333121018596));
#57862=CARTESIAN_POINT('Ctrl Pts',(0.13125579354894,1.,-4.0705393152874));
#57863=CARTESIAN_POINT('Ctrl Pts',(0.128500200484837,1.,-4.07774270738954));
#57864=CARTESIAN_POINT('Ctrl Pts',(0.12570647682254,1.,-4.08494093372377));
#57865=CARTESIAN_POINT('Ctrl Pts',(0.122874946249107,1.,-4.09213355850756));
#57866=CARTESIAN_POINT('Ctrl Pts',(0.120005924388124,1.,-4.09932031767002));
#57867=CARTESIAN_POINT('Ctrl Pts',(0.117099722731648,1.,-4.10650113381833));
#57868=CARTESIAN_POINT('Ctrl Pts',(0.114156649609545,1.,-4.11367603924961));
#57869=CARTESIAN_POINT('Ctrl Pts',(0.111177012683346,1.,-4.1208451250225));
#57870=CARTESIAN_POINT('Ctrl Pts',(0.108161120528369,1.,-4.12800848371504));
#57871=CARTESIAN_POINT('Ctrl Pts',(0.105109286538945,1.,-4.13516614458895));
#57872=CARTESIAN_POINT('Ctrl Pts',(0.102021826577584,1.,-4.14231804939538));
#57873=CARTESIAN_POINT('Ctrl Pts',(0.0988990478901223,1.,-4.14946408918485));
#57874=CARTESIAN_POINT('Ctrl Pts',(0.0957412403298004,1.,-4.15660412653577));
#57875=CARTESIAN_POINT('Ctrl Pts',(0.0925486672167528,1.,-4.16373802265839));
#57876=CARTESIAN_POINT('Ctrl Pts',(0.0893215560848647,1.,-4.17086566490794));
#57877=CARTESIAN_POINT('Ctrl Pts',(0.0860600915549394,1.,-4.17798698668094));
#57878=CARTESIAN_POINT('Ctrl Pts',(0.0827644164385676,1.,-4.18510195327123));
#57879=CARTESIAN_POINT('Ctrl Pts',(0.0801005887114317,1.,-4.19078883320504));
#57880=CARTESIAN_POINT('Ctrl Pts',(0.0780873956242395,1.,-4.19505112859416));
#57881=CARTESIAN_POINT('Ctrl Pts',(0.0767384596141462,1.,-4.1978913862118));
#57882=CARTESIAN_POINT('Ctrl Pts',(0.0760622897878244,1.,-4.19931119685982));
#57883=CARTESIAN_POINT('Origin',(0.0760622897878244,0.,-4.19931119685982));
#57884=CARTESIAN_POINT('',(-0.0760622897878238,1.,-4.19931119685982));
#57885=CARTESIAN_POINT('Origin',(0.,0.,0.));
#57886=CARTESIAN_POINT('',(0.385112848330761,1.,-3.73017266276651));
#57887=CARTESIAN_POINT('Origin',(0.,1.,0.));
#57888=CARTESIAN_POINT('Ctrl Pts',(0.385112848330762,1.,-3.73017266276651));
#57889=CARTESIAN_POINT('Ctrl Pts',(0.385112848330762,0.666666666666667,
-3.73017266276651));
#57890=CARTESIAN_POINT('Ctrl Pts',(0.385112848330762,0.333333333333333,
-3.73017266276651));
#57891=CARTESIAN_POINT('Ctrl Pts',(0.385112848330762,-0.333333333333333,
-3.73017266276651));
#57892=CARTESIAN_POINT('Ctrl Pts',(0.385112848330762,-0.666666666666667,
-3.73017266276651));
#57893=CARTESIAN_POINT('Ctrl Pts',(0.385112848330762,-1.,-3.73017266276651));
#57894=CARTESIAN_POINT('Ctrl Pts',(0.581791163835815,-1.,-4.15950947128175));
#57895=CARTESIAN_POINT('Ctrl Pts',(0.581791163835815,1.,-4.15950947128175));
#57896=CARTESIAN_POINT('Ctrl Pts',(0.580901211463535,-1.,-4.1582129171283));
#57897=CARTESIAN_POINT('Ctrl Pts',(0.580901211463535,1.,-4.1582129171283));
#57898=CARTESIAN_POINT('Ctrl Pts',(0.579124568914235,-1.,-4.15561864788576));
#57899=CARTESIAN_POINT('Ctrl Pts',(0.579124568914235,1.,-4.15561864788576));
#57900=CARTESIAN_POINT('Ctrl Pts',(0.576469391676688,-1.,-4.151723761217));
#57901=CARTESIAN_POINT('Ctrl Pts',(0.576469391676688,1.,-4.151723761217));
#57902=CARTESIAN_POINT('Ctrl Pts',(0.572948736069522,-1.,-4.14652361068081));
#57903=CARTESIAN_POINT('Ctrl Pts',(0.572948736069522,1.,-4.14652361068081));
#57904=CARTESIAN_POINT('Ctrl Pts',(0.568580610189774,-1.,-4.14001179830547));
#57905=CARTESIAN_POINT('Ctrl Pts',(0.568580610189774,1.,-4.14001179830547));
#57906=CARTESIAN_POINT('Ctrl Pts',(0.564245279537148,-1.,-4.13348835727104));
#57907=CARTESIAN_POINT('Ctrl Pts',(0.564245279537148,1.,-4.13348835727104));
#57908=CARTESIAN_POINT('Ctrl Pts',(0.559942890594773,-1.,-4.12695329951961));
#57909=CARTESIAN_POINT('Ctrl Pts',(0.559942890594773,1.,-4.12695329951961));
#57910=CARTESIAN_POINT('Ctrl Pts',(0.555673636129977,-1.,-4.12040666195664));
#57911=CARTESIAN_POINT('Ctrl Pts',(0.555673636129977,1.,-4.12040666195664));
#57912=CARTESIAN_POINT('Ctrl Pts',(0.551437758497032,-1.,-4.11384852024721));
#57913=CARTESIAN_POINT('Ctrl Pts',(0.551437758497032,1.,-4.11384852024721));
#57914=CARTESIAN_POINT('Ctrl Pts',(0.547235539485636,-1.,-4.10727897027977));
#57915=CARTESIAN_POINT('Ctrl Pts',(0.547235539485636,1.,-4.10727897027977));
#57916=CARTESIAN_POINT('Ctrl Pts',(0.543067286877757,-1.,-4.10069810243979));
#57917=CARTESIAN_POINT('Ctrl Pts',(0.543067286877757,1.,-4.10069810243979));
#57918=CARTESIAN_POINT('Ctrl Pts',(0.538933321179755,-1.,-4.09410597627));
#57919=CARTESIAN_POINT('Ctrl Pts',(0.538933321179755,1.,-4.09410597627));
#57920=CARTESIAN_POINT('Ctrl Pts',(0.534833963477273,-1.,-4.08750259988885));
#57921=CARTESIAN_POINT('Ctrl Pts',(0.534833963477273,1.,-4.08750259988885));
#57922=CARTESIAN_POINT('Ctrl Pts',(0.53076951872857,-1.,-4.08088789536836));
#57923=CARTESIAN_POINT('Ctrl Pts',(0.53076951872857,1.,-4.08088789536836));
#57924=CARTESIAN_POINT('Ctrl Pts',(0.526740277227498,-1.,-4.07426172299847));
#57925=CARTESIAN_POINT('Ctrl Pts',(0.526740277227498,1.,-4.07426172299847));
#57926=CARTESIAN_POINT('Ctrl Pts',(0.522746528603107,-1.,-4.06762394471314));
#57927=CARTESIAN_POINT('Ctrl Pts',(0.522746528603107,1.,-4.06762394471314));
#57928=CARTESIAN_POINT('Ctrl Pts',(0.518788572336923,-1.,-4.06097448038013));
#57929=CARTESIAN_POINT('Ctrl Pts',(0.518788572336923,1.,-4.06097448038013));
#57930=CARTESIAN_POINT('Ctrl Pts',(0.514866728193016,-1.,-4.05431335771199));
#57931=CARTESIAN_POINT('Ctrl Pts',(0.514866728193016,1.,-4.05431335771199));
#57932=CARTESIAN_POINT('Ctrl Pts',(0.51098134921897,-1.,-4.04764078815447));
#57933=CARTESIAN_POINT('Ctrl Pts',(0.51098134921897,1.,-4.04764078815447));
#57934=CARTESIAN_POINT('Ctrl Pts',(0.507132823288136,-1.,-4.04095715148915));
#57935=CARTESIAN_POINT('Ctrl Pts',(0.507132823288136,1.,-4.04095715148915));
#57936=CARTESIAN_POINT('Ctrl Pts',(0.503321556915346,-1.,-4.03426284174272));
#57937=CARTESIAN_POINT('Ctrl Pts',(0.503321556915346,1.,-4.03426284174272));
#57938=CARTESIAN_POINT('Ctrl Pts',(0.499547962340821,-1.,-4.02755813980101));
#57939=CARTESIAN_POINT('Ctrl Pts',(0.499547962340821,1.,-4.02755813980101));
#57940=CARTESIAN_POINT('Ctrl Pts',(0.495812444326251,-1.,-4.02084308851832));
#57941=CARTESIAN_POINT('Ctrl Pts',(0.495812444326251,1.,-4.02084308851832));
#57942=CARTESIAN_POINT('Ctrl Pts',(0.492115383418018,-1.,-4.01411733503546));
#57943=CARTESIAN_POINT('Ctrl Pts',(0.492115383418018,1.,-4.01411733503546));
#57944=CARTESIAN_POINT('Ctrl Pts',(0.488457130424633,-1.,-4.0073800839099));
#57945=CARTESIAN_POINT('Ctrl Pts',(0.488457130424633,1.,-4.0073800839099));
#57946=CARTESIAN_POINT('Ctrl Pts',(0.484838042421834,-1.,-4.00063045119288));
#57947=CARTESIAN_POINT('Ctrl Pts',(0.484838042421834,1.,-4.00063045119288));
#57948=CARTESIAN_POINT('Ctrl Pts',(0.481258512209675,-1.,-3.99386775880679));
#57949=CARTESIAN_POINT('Ctrl Pts',(0.481258512209675,1.,-3.99386775880679));
#57950=CARTESIAN_POINT('Ctrl Pts',(0.477718999122027,-1.,-3.98709184306738));
#57951=CARTESIAN_POINT('Ctrl Pts',(0.477718999122027,1.,-3.98709184306738));
#57952=CARTESIAN_POINT('Ctrl Pts',(0.474220061019509,-1.,-3.98030338044409));
#57953=CARTESIAN_POINT('Ctrl Pts',(0.474220061019509,1.,-3.98030338044409));
#57954=CARTESIAN_POINT('Ctrl Pts',(0.470762379613439,-1.,-3.97350414289392));
#57955=CARTESIAN_POINT('Ctrl Pts',(0.470762379613439,1.,-3.97350414289392));
#57956=CARTESIAN_POINT('Ctrl Pts',(0.467346690880643,-1.,-3.9666962227393));
#57957=CARTESIAN_POINT('Ctrl Pts',(0.467346690880643,1.,-3.9666962227393));
#57958=CARTESIAN_POINT('Ctrl Pts',(0.463973722115733,-1.,-3.95988133243538));
#57959=CARTESIAN_POINT('Ctrl Pts',(0.463973722115733,1.,-3.95988133243538));
#57960=CARTESIAN_POINT('Ctrl Pts',(0.460644124429121,-1.,-3.95306005817364));
#57961=CARTESIAN_POINT('Ctrl Pts',(0.460644124429121,1.,-3.95306005817364));
#57962=CARTESIAN_POINT('Ctrl Pts',(0.457358410451682,-1.,-3.94623117206678));
#57963=CARTESIAN_POINT('Ctrl Pts',(0.457358410451682,1.,-3.94623117206678));
#57964=CARTESIAN_POINT('Ctrl Pts',(0.454116879027584,-1.,-3.93939080846298));
#57965=CARTESIAN_POINT('Ctrl Pts',(0.454116879027584,1.,-3.93939080846298));
#57966=CARTESIAN_POINT('Ctrl Pts',(0.450919768356348,-1.,-3.93253407403123));
#57967=CARTESIAN_POINT('Ctrl Pts',(0.450919768356348,1.,-3.93253407403123));
#57968=CARTESIAN_POINT('Ctrl Pts',(0.447767416837292,-1.,-3.92565674143416));
#57969=CARTESIAN_POINT('Ctrl Pts',(0.447767416837292,1.,-3.92565674143416));
#57970=CARTESIAN_POINT('Ctrl Pts',(0.44466043023059,-1.,-3.91875701610719));
#57971=CARTESIAN_POINT('Ctrl Pts',(0.44466043023059,1.,-3.91875701610719));
#57972=CARTESIAN_POINT('Ctrl Pts',(0.441599824524054,-1.,-3.91183704069153));
#57973=CARTESIAN_POINT('Ctrl Pts',(0.441599824524054,1.,-3.91183704069153));
#57974=CARTESIAN_POINT('Ctrl Pts',(0.438587235458249,-1.,-3.90490512938563));
#57975=CARTESIAN_POINT('Ctrl Pts',(0.438587235458249,1.,-3.90490512938563));
#57976=CARTESIAN_POINT('Ctrl Pts',(0.435624629433527,-1.,-3.89797256655462));
#57977=CARTESIAN_POINT('Ctrl Pts',(0.435624629433527,1.,-3.89797256655462));
#57978=CARTESIAN_POINT('Ctrl Pts',(0.432713929544458,-1.,-3.89104947940611));
#57979=CARTESIAN_POINT('Ctrl Pts',(0.432713929544458,1.,-3.89104947940611));
#57980=CARTESIAN_POINT('Ctrl Pts',(0.429856640579741,-1.,-3.88414070943341));
#57981=CARTESIAN_POINT('Ctrl Pts',(0.429856640579741,1.,-3.88414070943341));
#57982=CARTESIAN_POINT('Ctrl Pts',(0.427053541173457,-1.,-3.87724240306597));
#57983=CARTESIAN_POINT('Ctrl Pts',(0.427053541173457,1.,-3.87724240306597));
#57984=CARTESIAN_POINT('Ctrl Pts',(0.42430417319511,-1.,-3.87033643487851));
#57985=CARTESIAN_POINT('Ctrl Pts',(0.42430417319511,1.,-3.87033643487851));
#57986=CARTESIAN_POINT('Ctrl Pts',(0.421607423177534,-1.,-3.86339652542709));
#57987=CARTESIAN_POINT('Ctrl Pts',(0.421607423177534,1.,-3.86339652542709));
#57988=CARTESIAN_POINT('Ctrl Pts',(0.418962468086773,-1.,-3.85639825647996));
#57989=CARTESIAN_POINT('Ctrl Pts',(0.418962468086773,1.,-3.85639825647996));
#57990=CARTESIAN_POINT('Ctrl Pts',(0.416369678052906,-1.,-3.84932864157497));
#57991=CARTESIAN_POINT('Ctrl Pts',(0.416369678052906,1.,-3.84932864157497));
#57992=CARTESIAN_POINT('Ctrl Pts',(0.413831367016748,-1.,-3.84219403994762));
#57993=CARTESIAN_POINT('Ctrl Pts',(0.413831367016748,1.,-3.84219403994762));
#57994=CARTESIAN_POINT('Ctrl Pts',(0.411353038798518,-1.,-3.83503345578698));
#57995=CARTESIAN_POINT('Ctrl Pts',(0.411353038798518,1.,-3.83503345578698));
#57996=CARTESIAN_POINT('Ctrl Pts',(0.408942371447459,-1.,-3.82790724256471));
#57997=CARTESIAN_POINT('Ctrl Pts',(0.408942371447459,1.,-3.82790724256471));
#57998=CARTESIAN_POINT('Ctrl Pts',(0.406607038258985,-1.,-3.8208730391381));
#57999=CARTESIAN_POINT('Ctrl Pts',(0.406607038258985,1.,-3.8208730391381));
#58000=CARTESIAN_POINT('Ctrl Pts',(0.404352694628273,-1.,-3.81396374287793));
#58001=CARTESIAN_POINT('Ctrl Pts',(0.404352694628273,1.,-3.81396374287793));
#58002=CARTESIAN_POINT('Ctrl Pts',(0.402181320148435,-1.,-3.80716881962728));
#58003=CARTESIAN_POINT('Ctrl Pts',(0.402181320148435,1.,-3.80716881962728));
#58004=CARTESIAN_POINT('Ctrl Pts',(0.4000883465046,-1.,-3.80040370384546));
#58005=CARTESIAN_POINT('Ctrl Pts',(0.4000883465046,1.,-3.80040370384546));
#58006=CARTESIAN_POINT('Ctrl Pts',(0.398064818683969,-1.,-3.7935288716329));
#58007=CARTESIAN_POINT('Ctrl Pts',(0.398064818683969,1.,-3.7935288716329));
#58008=CARTESIAN_POINT('Ctrl Pts',(0.39610320533484,-1.,-3.78640521279313));
#58009=CARTESIAN_POINT('Ctrl Pts',(0.39610320533484,1.,-3.78640521279313));
#58010=CARTESIAN_POINT('Ctrl Pts',(0.394202481011499,-1.,-3.77894173114283));
#58011=CARTESIAN_POINT('Ctrl Pts',(0.394202481011499,1.,-3.77894173114283));
#58012=CARTESIAN_POINT('Ctrl Pts',(0.392372786223432,-1.,-3.77114011595967));
#58013=CARTESIAN_POINT('Ctrl Pts',(0.392372786223432,1.,-3.77114011595967));
#58014=CARTESIAN_POINT('Ctrl Pts',(0.390642072979559,-1.,-3.76315635033257));
#58015=CARTESIAN_POINT('Ctrl Pts',(0.390642072979559,1.,-3.76315635033257));
#58016=CARTESIAN_POINT('Ctrl Pts',(0.389054775898701,-1.,-3.75529302895152));
#58017=CARTESIAN_POINT('Ctrl Pts',(0.389054775898701,1.,-3.75529302895152));
#58018=CARTESIAN_POINT('Ctrl Pts',(0.387663020050836,-1.,-3.74792651696654));
#58019=CARTESIAN_POINT('Ctrl Pts',(0.387663020050836,1.,-3.74792651696654));
#58020=CARTESIAN_POINT('Ctrl Pts',(0.386519576222251,-1.,-3.74144965781276));
#58021=CARTESIAN_POINT('Ctrl Pts',(0.386519576222251,1.,-3.74144965781276));
#58022=CARTESIAN_POINT('Ctrl Pts',(0.385670806454565,-1.,-3.73621371845318));
#58023=CARTESIAN_POINT('Ctrl Pts',(0.385670806454565,1.,-3.73621371845318));
#58024=CARTESIAN_POINT('Ctrl Pts',(0.385147887988951,-1.,-3.73245705638843));
#58025=CARTESIAN_POINT('Ctrl Pts',(0.385147887988951,1.,-3.73245705638843));
#58026=CARTESIAN_POINT('Ctrl Pts',(0.385001870183213,-1.,-3.73072465900175));
#58027=CARTESIAN_POINT('Ctrl Pts',(0.385001870183213,1.,-3.73072465900175));
#58028=CARTESIAN_POINT('Ctrl Pts',(0.385047711603462,-1.,-3.73015851028356));
#58029=CARTESIAN_POINT('Ctrl Pts',(0.385047711603462,1.,-3.73015851028356));
#58030=CARTESIAN_POINT('Ctrl Pts',(0.385147278814642,-1.,-3.73010668803042));
#58031=CARTESIAN_POINT('Ctrl Pts',(0.385147278814642,1.,-3.73010668803042));
#58032=CARTESIAN_POINT('Ctrl Pts',(0.385214314776329,-1.,-3.73016218570874));
#58033=CARTESIAN_POINT('Ctrl Pts',(0.385214314776329,1.,-3.73016218570874));
#58034=CARTESIAN_POINT('',(0.581791163835815,1.,-4.15950947128175));
#58035=CARTESIAN_POINT('Ctrl Pts',(0.581791163835815,1.,-4.15950947128175));
#58036=CARTESIAN_POINT('Ctrl Pts',(0.580901211463535,1.,-4.1582129171283));
#58037=CARTESIAN_POINT('Ctrl Pts',(0.579124568914235,1.,-4.15561864788576));
#58038=CARTESIAN_POINT('Ctrl Pts',(0.576469391676688,1.,-4.151723761217));
#58039=CARTESIAN_POINT('Ctrl Pts',(0.572948736069522,1.,-4.14652361068081));
#58040=CARTESIAN_POINT('Ctrl Pts',(0.568580610189774,1.,-4.14001179830547));
#58041=CARTESIAN_POINT('Ctrl Pts',(0.564245279537148,1.,-4.13348835727104));
#58042=CARTESIAN_POINT('Ctrl Pts',(0.559942890594773,1.,-4.12695329951961));
#58043=CARTESIAN_POINT('Ctrl Pts',(0.555673636129977,1.,-4.12040666195664));
#58044=CARTESIAN_POINT('Ctrl Pts',(0.551437758497032,1.,-4.11384852024721));
#58045=CARTESIAN_POINT('Ctrl Pts',(0.547235539485636,1.,-4.10727897027977));
#58046=CARTESIAN_POINT('Ctrl Pts',(0.543067286877757,1.,-4.10069810243979));
#58047=CARTESIAN_POINT('Ctrl Pts',(0.538933321179755,1.,-4.09410597627));
#58048=CARTESIAN_POINT('Ctrl Pts',(0.534833963477273,1.,-4.08750259988885));
#58049=CARTESIAN_POINT('Ctrl Pts',(0.53076951872857,1.,-4.08088789536836));
#58050=CARTESIAN_POINT('Ctrl Pts',(0.526740277227498,1.,-4.07426172299847));
#58051=CARTESIAN_POINT('Ctrl Pts',(0.522746528603107,1.,-4.06762394471314));
#58052=CARTESIAN_POINT('Ctrl Pts',(0.518788572336923,1.,-4.06097448038013));
#58053=CARTESIAN_POINT('Ctrl Pts',(0.514866728193016,1.,-4.05431335771199));
#58054=CARTESIAN_POINT('Ctrl Pts',(0.51098134921897,1.,-4.04764078815447));
#58055=CARTESIAN_POINT('Ctrl Pts',(0.507132823288136,1.,-4.04095715148915));
#58056=CARTESIAN_POINT('Ctrl Pts',(0.503321556915346,1.,-4.03426284174272));
#58057=CARTESIAN_POINT('Ctrl Pts',(0.499547962340821,1.,-4.02755813980101));
#58058=CARTESIAN_POINT('Ctrl Pts',(0.495812444326251,1.,-4.02084308851832));
#58059=CARTESIAN_POINT('Ctrl Pts',(0.492115383418018,1.,-4.01411733503546));
#58060=CARTESIAN_POINT('Ctrl Pts',(0.488457130424633,1.,-4.0073800839099));
#58061=CARTESIAN_POINT('Ctrl Pts',(0.484838042421834,1.,-4.00063045119288));
#58062=CARTESIAN_POINT('Ctrl Pts',(0.481258512209675,1.,-3.99386775880679));
#58063=CARTESIAN_POINT('Ctrl Pts',(0.477718999122027,1.,-3.98709184306738));
#58064=CARTESIAN_POINT('Ctrl Pts',(0.474220061019509,1.,-3.98030338044409));
#58065=CARTESIAN_POINT('Ctrl Pts',(0.470762379613439,1.,-3.97350414289392));
#58066=CARTESIAN_POINT('Ctrl Pts',(0.467346690880643,1.,-3.9666962227393));
#58067=CARTESIAN_POINT('Ctrl Pts',(0.463973722115733,1.,-3.95988133243538));
#58068=CARTESIAN_POINT('Ctrl Pts',(0.460644124429121,1.,-3.95306005817364));
#58069=CARTESIAN_POINT('Ctrl Pts',(0.457358410451682,1.,-3.94623117206678));
#58070=CARTESIAN_POINT('Ctrl Pts',(0.454116879027584,1.,-3.93939080846298));
#58071=CARTESIAN_POINT('Ctrl Pts',(0.450919768356348,1.,-3.93253407403123));
#58072=CARTESIAN_POINT('Ctrl Pts',(0.447767416837292,1.,-3.92565674143416));
#58073=CARTESIAN_POINT('Ctrl Pts',(0.44466043023059,1.,-3.91875701610719));
#58074=CARTESIAN_POINT('Ctrl Pts',(0.441599824524054,1.,-3.91183704069153));
#58075=CARTESIAN_POINT('Ctrl Pts',(0.438587235458249,1.,-3.90490512938563));
#58076=CARTESIAN_POINT('Ctrl Pts',(0.435624629433527,1.,-3.89797256655462));
#58077=CARTESIAN_POINT('Ctrl Pts',(0.432713929544458,1.,-3.89104947940611));
#58078=CARTESIAN_POINT('Ctrl Pts',(0.429856640579741,1.,-3.88414070943341));
#58079=CARTESIAN_POINT('Ctrl Pts',(0.427053541173457,1.,-3.87724240306597));
#58080=CARTESIAN_POINT('Ctrl Pts',(0.42430417319511,1.,-3.87033643487851));
#58081=CARTESIAN_POINT('Ctrl Pts',(0.421607423177534,1.,-3.86339652542709));
#58082=CARTESIAN_POINT('Ctrl Pts',(0.418962468086773,1.,-3.85639825647996));
#58083=CARTESIAN_POINT('Ctrl Pts',(0.416369678052906,1.,-3.84932864157497));
#58084=CARTESIAN_POINT('Ctrl Pts',(0.413831367016748,1.,-3.84219403994762));
#58085=CARTESIAN_POINT('Ctrl Pts',(0.411353038798518,1.,-3.83503345578698));
#58086=CARTESIAN_POINT('Ctrl Pts',(0.408942371447459,1.,-3.82790724256471));
#58087=CARTESIAN_POINT('Ctrl Pts',(0.406607038258985,1.,-3.8208730391381));
#58088=CARTESIAN_POINT('Ctrl Pts',(0.404352694628273,1.,-3.81396374287793));
#58089=CARTESIAN_POINT('Ctrl Pts',(0.402181320148435,1.,-3.80716881962728));
#58090=CARTESIAN_POINT('Ctrl Pts',(0.4000883465046,1.,-3.80040370384546));
#58091=CARTESIAN_POINT('Ctrl Pts',(0.398064818683969,1.,-3.7935288716329));
#58092=CARTESIAN_POINT('Ctrl Pts',(0.39610320533484,1.,-3.78640521279313));
#58093=CARTESIAN_POINT('Ctrl Pts',(0.394202481011499,1.,-3.77894173114283));
#58094=CARTESIAN_POINT('Ctrl Pts',(0.392372786223432,1.,-3.77114011595967));
#58095=CARTESIAN_POINT('Ctrl Pts',(0.390642072979559,1.,-3.76315635033257));
#58096=CARTESIAN_POINT('Ctrl Pts',(0.389054775898701,1.,-3.75529302895152));
#58097=CARTESIAN_POINT('Ctrl Pts',(0.387663020050836,1.,-3.74792651696654));
#58098=CARTESIAN_POINT('Ctrl Pts',(0.386519576222251,1.,-3.74144965781276));
#58099=CARTESIAN_POINT('Ctrl Pts',(0.385670806454565,1.,-3.73621371845318));
#58100=CARTESIAN_POINT('Ctrl Pts',(0.385187124634206,1.,-3.73273893363406));
#58101=CARTESIAN_POINT('Ctrl Pts',(0.385031656499163,1.,-3.73106082862548));
#58102=CARTESIAN_POINT('Ctrl Pts',(0.385037797881504,1.,-3.73040527621055));
#58103=CARTESIAN_POINT('Ctrl Pts',(0.385087139000374,1.,-3.73021431755274));
#58104=CARTESIAN_POINT('Ctrl Pts',(0.385112848330761,1.,-3.73017266276651));
#58105=CARTESIAN_POINT('',(0.581791163835815,0.,-4.15950947128175));
#58106=CARTESIAN_POINT('Ctrl Pts',(0.786322922920599,-1.,-3.66663282329846));
#58107=CARTESIAN_POINT('Ctrl Pts',(0.786322922920599,1.,-3.66663282329846));
#58108=CARTESIAN_POINT('Ctrl Pts',(0.786369528183326,-1.,-3.66655932661986));
#58109=CARTESIAN_POINT('Ctrl Pts',(0.786369528183326,1.,-3.66655932661986));
#58110=CARTESIAN_POINT('Ctrl Pts',(0.786480236185696,-1.,-3.66657784455334));
#58111=CARTESIAN_POINT('Ctrl Pts',(0.786480236185696,1.,-3.66657784455334));
#58112=CARTESIAN_POINT('Ctrl Pts',(0.786698783542764,-1.,-3.66710211820482));
#58113=CARTESIAN_POINT('Ctrl Pts',(0.786698783542764,1.,-3.66710211820482));
#58114=CARTESIAN_POINT('Ctrl Pts',(0.787095252590501,-1.,-3.66879484801113));
#58115=CARTESIAN_POINT('Ctrl Pts',(0.787095252590501,1.,-3.66879484801113));
#58116=CARTESIAN_POINT('Ctrl Pts',(0.787758799995742,-1.,-3.67252923663655));
#58117=CARTESIAN_POINT('Ctrl Pts',(0.787758799995742,1.,-3.67252923663655));
#58118=CARTESIAN_POINT('Ctrl Pts',(0.788569566220285,-1.,-3.67777119516252));
#58119=CARTESIAN_POINT('Ctrl Pts',(0.788569566220285,1.,-3.67777119516252));
#58120=CARTESIAN_POINT('Ctrl Pts',(0.789483546064386,-1.,-3.68428439783905));
#58121=CARTESIAN_POINT('Ctrl Pts',(0.789483546064386,1.,-3.68428439783905));
#58122=CARTESIAN_POINT('Ctrl Pts',(0.790436284988787,-1.,-3.69172044327364));
#58123=CARTESIAN_POINT('Ctrl Pts',(0.790436284988787,1.,-3.69172044327364));
#58124=CARTESIAN_POINT('Ctrl Pts',(0.79135657569598,-1.,-3.69968940808721));
#58125=CARTESIAN_POINT('Ctrl Pts',(0.79135657569598,1.,-3.69968940808721));
#58126=CARTESIAN_POINT('Ctrl Pts',(0.792177688845817,-1.,-3.70781724021806));
#58127=CARTESIAN_POINT('Ctrl Pts',(0.792177688845817,1.,-3.70781724021806));
#58128=CARTESIAN_POINT('Ctrl Pts',(0.792848377370287,-1.,-3.71580242396124));
#58129=CARTESIAN_POINT('Ctrl Pts',(0.792848377370287,1.,-3.71580242396124));
#58130=CARTESIAN_POINT('Ctrl Pts',(0.793347023784204,-1.,-3.72348797293734));
#58131=CARTESIAN_POINT('Ctrl Pts',(0.793347023784204,1.,-3.72348797293734));
#58132=CARTESIAN_POINT('Ctrl Pts',(0.793682750269684,-1.,-3.73086914695805));
#58133=CARTESIAN_POINT('Ctrl Pts',(0.793682750269684,1.,-3.73086914695805));
#58134=CARTESIAN_POINT('Ctrl Pts',(0.793882700937016,-1.,-3.73803280541687));
#58135=CARTESIAN_POINT('Ctrl Pts',(0.793882700937016,1.,-3.73803280541687));
#58136=CARTESIAN_POINT('Ctrl Pts',(0.793982700459951,-1.,-3.74511357728861));
#58137=CARTESIAN_POINT('Ctrl Pts',(0.793982700459951,1.,-3.74511357728861));
#58138=CARTESIAN_POINT('Ctrl Pts',(0.794017347371377,-1.,-3.75224692493864));
#58139=CARTESIAN_POINT('Ctrl Pts',(0.794017347371377,1.,-3.75224692493864));
#58140=CARTESIAN_POINT('Ctrl Pts',(0.794008429134907,-1.,-3.75951468666257));
#58141=CARTESIAN_POINT('Ctrl Pts',(0.794008429134907,1.,-3.75951468666257));
#58142=CARTESIAN_POINT('Ctrl Pts',(0.793961083688991,-1.,-3.76692626931111));
#58143=CARTESIAN_POINT('Ctrl Pts',(0.793961083688991,1.,-3.76692626931111));
#58144=CARTESIAN_POINT('Ctrl Pts',(0.793870523787407,-1.,-3.77444863801212));
#58145=CARTESIAN_POINT('Ctrl Pts',(0.793870523787407,1.,-3.77444863801212));
#58146=CARTESIAN_POINT('Ctrl Pts',(0.7937262357813,-1.,-3.78202460377598));
#58147=CARTESIAN_POINT('Ctrl Pts',(0.7937262357813,1.,-3.78202460377598));
#58148=CARTESIAN_POINT('Ctrl Pts',(0.793516871680993,-1.,-3.78959439439235));
#58149=CARTESIAN_POINT('Ctrl Pts',(0.793516871680993,1.,-3.78959439439235));
#58150=CARTESIAN_POINT('Ctrl Pts',(0.793235612973273,-1.,-3.79711921389897));
#58151=CARTESIAN_POINT('Ctrl Pts',(0.793235612973273,1.,-3.79711921389897));
#58152=CARTESIAN_POINT('Ctrl Pts',(0.792882695234777,-1.,-3.80459229925637));
#58153=CARTESIAN_POINT('Ctrl Pts',(0.792882695234777,1.,-3.80459229925637));
#58154=CARTESIAN_POINT('Ctrl Pts',(0.792462483517634,-1.,-3.81202588694756));
#58155=CARTESIAN_POINT('Ctrl Pts',(0.792462483517634,1.,-3.81202588694756));
#58156=CARTESIAN_POINT('Ctrl Pts',(0.791981740718634,-1.,-3.81944345442249));
#58157=CARTESIAN_POINT('Ctrl Pts',(0.791981740718634,1.,-3.81944345442249));
#58158=CARTESIAN_POINT('Ctrl Pts',(0.791447528662369,-1.,-3.82687033899792));
#58159=CARTESIAN_POINT('Ctrl Pts',(0.791447528662369,1.,-3.82687033899792));
#58160=CARTESIAN_POINT('Ctrl Pts',(0.7908650127053,-1.,-3.83432392054786));
#58161=CARTESIAN_POINT('Ctrl Pts',(0.7908650127053,1.,-3.83432392054786));
#58162=CARTESIAN_POINT('Ctrl Pts',(0.790236124191242,-1.,-3.84180762342454));
#58163=CARTESIAN_POINT('Ctrl Pts',(0.790236124191242,1.,-3.84180762342454));
#58164=CARTESIAN_POINT('Ctrl Pts',(0.789560798155582,-1.,-3.84931637808894));
#58165=CARTESIAN_POINT('Ctrl Pts',(0.789560798155582,1.,-3.84931637808894));
#58166=CARTESIAN_POINT('Ctrl Pts',(0.788837734090671,-1.,-3.85683995872529));
#58167=CARTESIAN_POINT('Ctrl Pts',(0.788837734090671,1.,-3.85683995872529));
#58168=CARTESIAN_POINT('Ctrl Pts',(0.788065315093777,-1.,-3.86436702561345));
#58169=CARTESIAN_POINT('Ctrl Pts',(0.788065315093777,1.,-3.86436702561345));
#58170=CARTESIAN_POINT('Ctrl Pts',(0.787242527617999,-1.,-3.87188916600912));
#58171=CARTESIAN_POINT('Ctrl Pts',(0.787242527617999,1.,-3.87188916600912));
#58172=CARTESIAN_POINT('Ctrl Pts',(0.786369675812608,-1.,-3.8794040281819));
#58173=CARTESIAN_POINT('Ctrl Pts',(0.786369675812608,1.,-3.8794040281819));
#58174=CARTESIAN_POINT('Ctrl Pts',(0.78544789034073,-1.,-3.88691313167398));
#58175=CARTESIAN_POINT('Ctrl Pts',(0.78544789034073,1.,-3.88691313167398));
#58176=CARTESIAN_POINT('Ctrl Pts',(0.784478799358336,-1.,-3.89442039235103));
#58177=CARTESIAN_POINT('Ctrl Pts',(0.784478799358336,1.,-3.89442039235103));
#58178=CARTESIAN_POINT('Ctrl Pts',(0.783464141529081,-1.,-3.9019303904397));
#58179=CARTESIAN_POINT('Ctrl Pts',(0.783464141529081,1.,-3.9019303904397));
#58180=CARTESIAN_POINT('Ctrl Pts',(0.782405395622764,-1.,-3.90944671004542));
#58181=CARTESIAN_POINT('Ctrl Pts',(0.782405395622764,1.,-3.90944671004542));
#58182=CARTESIAN_POINT('Ctrl Pts',(0.781303428618366,-1.,-3.91697036054676));
#58183=CARTESIAN_POINT('Ctrl Pts',(0.781303428618366,1.,-3.91697036054676));
#58184=CARTESIAN_POINT('Ctrl Pts',(0.780158678615542,-1.,-3.92450058323823));
#58185=CARTESIAN_POINT('Ctrl Pts',(0.780158678615542,1.,-3.92450058323823));
#58186=CARTESIAN_POINT('Ctrl Pts',(0.77897130813482,-1.,-3.93203552473174));
#58187=CARTESIAN_POINT('Ctrl Pts',(0.77897130813482,1.,-3.93203552473174));
#58188=CARTESIAN_POINT('Ctrl Pts',(0.777741370568558,-1.,-3.93957296768103));
#58189=CARTESIAN_POINT('Ctrl Pts',(0.777741370568558,1.,-3.93957296768103));
#58190=CARTESIAN_POINT('Ctrl Pts',(0.776468966697921,-1.,-3.94711101619447));
#58191=CARTESIAN_POINT('Ctrl Pts',(0.776468966697921,1.,-3.94711101619447));
#58192=CARTESIAN_POINT('Ctrl Pts',(0.775154418039351,-1.,-3.9546488545231));
#58193=CARTESIAN_POINT('Ctrl Pts',(0.775154418039351,1.,-3.9546488545231));
#58194=CARTESIAN_POINT('Ctrl Pts',(0.773798212026565,-1.,-3.96218649639807));
#58195=CARTESIAN_POINT('Ctrl Pts',(0.773798212026565,1.,-3.96218649639807));
#58196=CARTESIAN_POINT('Ctrl Pts',(0.772400931772136,-1.,-3.96972446532772));
#58197=CARTESIAN_POINT('Ctrl Pts',(0.772400931772136,1.,-3.96972446532772));
#58198=CARTESIAN_POINT('Ctrl Pts',(0.77096319003047,-1.,-3.97726349165488));
#58199=CARTESIAN_POINT('Ctrl Pts',(0.77096319003047,1.,-3.97726349165488));
#58200=CARTESIAN_POINT('Ctrl Pts',(0.769485566245544,-1.,-3.98480422348451));
#58201=CARTESIAN_POINT('Ctrl Pts',(0.769485566245544,1.,-3.98480422348451));
#58202=CARTESIAN_POINT('Ctrl Pts',(0.767968531377914,-1.,-3.9923468788101));
#58203=CARTESIAN_POINT('Ctrl Pts',(0.767968531377914,1.,-3.9923468788101));
#58204=CARTESIAN_POINT('Ctrl Pts',(0.766412457136063,-1.,-3.99989129179622));
#58205=CARTESIAN_POINT('Ctrl Pts',(0.766412457136063,1.,-3.99989129179622));
#58206=CARTESIAN_POINT('Ctrl Pts',(0.764817648785197,-1.,-4.00743706791509));
#58207=CARTESIAN_POINT('Ctrl Pts',(0.764817648785197,1.,-4.00743706791509));
#58208=CARTESIAN_POINT('Ctrl Pts',(0.763184371182935,-1.,-4.01498370680496));
#58209=CARTESIAN_POINT('Ctrl Pts',(0.763184371182935,1.,-4.01498370680496));
#58210=CARTESIAN_POINT('Ctrl Pts',(0.761512875859804,-1.,-4.02253072741268));
#58211=CARTESIAN_POINT('Ctrl Pts',(0.761512875859804,1.,-4.02253072741268));
#58212=CARTESIAN_POINT('Ctrl Pts',(0.759803433243751,-1.,-4.03007781954412));
#58213=CARTESIAN_POINT('Ctrl Pts',(0.759803433243751,1.,-4.03007781954412));
#58214=CARTESIAN_POINT('Ctrl Pts',(0.758056338884944,-1.,-4.03762485803119));
#58215=CARTESIAN_POINT('Ctrl Pts',(0.758056338884944,1.,-4.03762485803119));
#58216=CARTESIAN_POINT('Ctrl Pts',(0.75627190236958,-1.,-4.04517182653997));
#58217=CARTESIAN_POINT('Ctrl Pts',(0.75627190236958,1.,-4.04517182653997));
#58218=CARTESIAN_POINT('Ctrl Pts',(0.754450441816078,-1.,-4.05271876687915));
#58219=CARTESIAN_POINT('Ctrl Pts',(0.754450441816078,1.,-4.05271876687915));
#58220=CARTESIAN_POINT('Ctrl Pts',(0.752592276483072,-1.,-4.06026572221515));
#58221=CARTESIAN_POINT('Ctrl Pts',(0.752592276483072,1.,-4.06026572221515));
#58222=CARTESIAN_POINT('Ctrl Pts',(0.750697720484036,-1.,-4.06781267242378));
#58223=CARTESIAN_POINT('Ctrl Pts',(0.750697720484036,1.,-4.06781267242378));
#58224=CARTESIAN_POINT('Ctrl Pts',(0.748767076680557,-1.,-4.07535951056152));
#58225=CARTESIAN_POINT('Ctrl Pts',(0.748767076680557,1.,-4.07535951056152));
#58226=CARTESIAN_POINT('Ctrl Pts',(0.746800631492315,-1.,-4.08290608095642));
#58227=CARTESIAN_POINT('Ctrl Pts',(0.746800631492315,1.,-4.08290608095642));
#58228=CARTESIAN_POINT('Ctrl Pts',(0.7447986497065,-1.,-4.09045220253573));
#58229=CARTESIAN_POINT('Ctrl Pts',(0.7447986497065,1.,-4.09045220253573));
#58230=CARTESIAN_POINT('Ctrl Pts',(0.742761369689841,-1.,-4.09799769702611));
#58231=CARTESIAN_POINT('Ctrl Pts',(0.742761369689841,1.,-4.09799769702611));
#58232=CARTESIAN_POINT('Ctrl Pts',(0.740688998553376,-1.,-4.10554241757547));
#58233=CARTESIAN_POINT('Ctrl Pts',(0.740688998553376,1.,-4.10554241757547));
#58234=CARTESIAN_POINT('Ctrl Pts',(0.738581708225843,-1.,-4.11308626951927));
#58235=CARTESIAN_POINT('Ctrl Pts',(0.738581708225843,1.,-4.11308626951927));
#58236=CARTESIAN_POINT('Ctrl Pts',(0.736439634331344,-1.,-4.120629196238));
#58237=CARTESIAN_POINT('Ctrl Pts',(0.736439634331344,1.,-4.120629196238));
#58238=CARTESIAN_POINT('Ctrl Pts',(0.734698226764092,-1.,-4.12666277570844));
#58239=CARTESIAN_POINT('Ctrl Pts',(0.734698226764092,1.,-4.12666277570844));
#58240=CARTESIAN_POINT('Ctrl Pts',(0.733376589323546,-1.,-4.13118752795207));
#58241=CARTESIAN_POINT('Ctrl Pts',(0.733376589323546,1.,-4.13118752795207));
#58242=CARTESIAN_POINT('Ctrl Pts',(0.732488575135159,-1.,-4.1342038373684));
#58243=CARTESIAN_POINT('Ctrl Pts',(0.732488575135159,1.,-4.1342038373684));
#58244=CARTESIAN_POINT('Ctrl Pts',(0.73204283740062,-1.,-4.13571194405636));
#58245=CARTESIAN_POINT('Ctrl Pts',(0.73204283740062,1.,-4.13571194405636));
#58246=CARTESIAN_POINT('',(0.786422660831986,1.,-3.66661143271685));
#58247=CARTESIAN_POINT('Ctrl Pts',(0.786422660831985,-1.,-3.66661143271685));
#58248=CARTESIAN_POINT('Ctrl Pts',(0.786422660831985,-0.666666666666667,
-3.66661143271685));
#58249=CARTESIAN_POINT('Ctrl Pts',(0.786422660831985,-0.333333333333333,
-3.66661143271685));
#58250=CARTESIAN_POINT('Ctrl Pts',(0.786422660831985,0.333333333333333,
-3.66661143271685));
#58251=CARTESIAN_POINT('Ctrl Pts',(0.786422660831985,0.666666666666667,
-3.66661143271685));
#58252=CARTESIAN_POINT('Ctrl Pts',(0.786422660831985,1.,-3.66661143271685));
#58253=CARTESIAN_POINT('',(0.73204283740062,1.,-4.13571194405636));
#58254=CARTESIAN_POINT('',(0.73204283740062,0.,-4.13571194405636));
#58255=CARTESIAN_POINT('Ctrl Pts',(0.786422660831986,1.,-3.66661143271685));
#58256=CARTESIAN_POINT('Ctrl Pts',(0.786459983895432,1.,-3.6666431041522));
#58257=CARTESIAN_POINT('Ctrl Pts',(0.786565919558984,1.,-3.66680946938293));
#58258=CARTESIAN_POINT('Ctrl Pts',(0.786774337198062,1.,-3.66743103898702));
#58259=CARTESIAN_POINT('Ctrl Pts',(0.787145041181546,1.,-3.66907505398677));
#58260=CARTESIAN_POINT('Ctrl Pts',(0.787758799995742,1.,-3.67252923663655));
#58261=CARTESIAN_POINT('Ctrl Pts',(0.788569566220285,1.,-3.67777119516252));
#58262=CARTESIAN_POINT('Ctrl Pts',(0.789483546064386,1.,-3.68428439783905));
#58263=CARTESIAN_POINT('Ctrl Pts',(0.790436284988787,1.,-3.69172044327364));
#58264=CARTESIAN_POINT('Ctrl Pts',(0.79135657569598,1.,-3.69968940808721));
#58265=CARTESIAN_POINT('Ctrl Pts',(0.792177688845817,1.,-3.70781724021806));
#58266=CARTESIAN_POINT('Ctrl Pts',(0.792848377370287,1.,-3.71580242396124));
#58267=CARTESIAN_POINT('Ctrl Pts',(0.793347023784204,1.,-3.72348797293734));
#58268=CARTESIAN_POINT('Ctrl Pts',(0.793682750269684,1.,-3.73086914695805));
#58269=CARTESIAN_POINT('Ctrl Pts',(0.793882700937016,1.,-3.73803280541687));
#58270=CARTESIAN_POINT('Ctrl Pts',(0.793982700459951,1.,-3.74511357728861));
#58271=CARTESIAN_POINT('Ctrl Pts',(0.794017347371377,1.,-3.75224692493864));
#58272=CARTESIAN_POINT('Ctrl Pts',(0.794008429134907,1.,-3.75951468666257));
#58273=CARTESIAN_POINT('Ctrl Pts',(0.793961083688991,1.,-3.76692626931111));
#58274=CARTESIAN_POINT('Ctrl Pts',(0.793870523787407,1.,-3.77444863801212));
#58275=CARTESIAN_POINT('Ctrl Pts',(0.7937262357813,1.,-3.78202460377598));
#58276=CARTESIAN_POINT('Ctrl Pts',(0.793516871680993,1.,-3.78959439439235));
#58277=CARTESIAN_POINT('Ctrl Pts',(0.793235612973273,1.,-3.79711921389897));
#58278=CARTESIAN_POINT('Ctrl Pts',(0.792882695234777,1.,-3.80459229925637));
#58279=CARTESIAN_POINT('Ctrl Pts',(0.792462483517634,1.,-3.81202588694756));
#58280=CARTESIAN_POINT('Ctrl Pts',(0.791981740718634,1.,-3.81944345442249));
#58281=CARTESIAN_POINT('Ctrl Pts',(0.791447528662369,1.,-3.82687033899792));
#58282=CARTESIAN_POINT('Ctrl Pts',(0.7908650127053,1.,-3.83432392054786));
#58283=CARTESIAN_POINT('Ctrl Pts',(0.790236124191242,1.,-3.84180762342454));
#58284=CARTESIAN_POINT('Ctrl Pts',(0.789560798155582,1.,-3.84931637808894));
#58285=CARTESIAN_POINT('Ctrl Pts',(0.788837734090671,1.,-3.85683995872529));
#58286=CARTESIAN_POINT('Ctrl Pts',(0.788065315093777,1.,-3.86436702561345));
#58287=CARTESIAN_POINT('Ctrl Pts',(0.787242527617999,1.,-3.87188916600912));
#58288=CARTESIAN_POINT('Ctrl Pts',(0.786369675812608,1.,-3.8794040281819));
#58289=CARTESIAN_POINT('Ctrl Pts',(0.78544789034073,1.,-3.88691313167398));
#58290=CARTESIAN_POINT('Ctrl Pts',(0.784478799358336,1.,-3.89442039235103));
#58291=CARTESIAN_POINT('Ctrl Pts',(0.783464141529081,1.,-3.9019303904397));
#58292=CARTESIAN_POINT('Ctrl Pts',(0.782405395622764,1.,-3.90944671004542));
#58293=CARTESIAN_POINT('Ctrl Pts',(0.781303428618366,1.,-3.91697036054676));
#58294=CARTESIAN_POINT('Ctrl Pts',(0.780158678615542,1.,-3.92450058323823));
#58295=CARTESIAN_POINT('Ctrl Pts',(0.77897130813482,1.,-3.93203552473174));
#58296=CARTESIAN_POINT('Ctrl Pts',(0.777741370568558,1.,-3.93957296768103));
#58297=CARTESIAN_POINT('Ctrl Pts',(0.776468966697921,1.,-3.94711101619447));
#58298=CARTESIAN_POINT('Ctrl Pts',(0.775154418039351,1.,-3.9546488545231));
#58299=CARTESIAN_POINT('Ctrl Pts',(0.773798212026565,1.,-3.96218649639807));
#58300=CARTESIAN_POINT('Ctrl Pts',(0.772400931772136,1.,-3.96972446532772));
#58301=CARTESIAN_POINT('Ctrl Pts',(0.77096319003047,1.,-3.97726349165488));
#58302=CARTESIAN_POINT('Ctrl Pts',(0.769485566245544,1.,-3.98480422348451));
#58303=CARTESIAN_POINT('Ctrl Pts',(0.767968531377914,1.,-3.9923468788101));
#58304=CARTESIAN_POINT('Ctrl Pts',(0.766412457136063,1.,-3.99989129179622));
#58305=CARTESIAN_POINT('Ctrl Pts',(0.764817648785197,1.,-4.00743706791509));
#58306=CARTESIAN_POINT('Ctrl Pts',(0.763184371182935,1.,-4.01498370680496));
#58307=CARTESIAN_POINT('Ctrl Pts',(0.761512875859804,1.,-4.02253072741268));
#58308=CARTESIAN_POINT('Ctrl Pts',(0.759803433243751,1.,-4.03007781954412));
#58309=CARTESIAN_POINT('Ctrl Pts',(0.758056338884944,1.,-4.03762485803119));
#58310=CARTESIAN_POINT('Ctrl Pts',(0.75627190236958,1.,-4.04517182653997));
#58311=CARTESIAN_POINT('Ctrl Pts',(0.754450441816078,1.,-4.05271876687915));
#58312=CARTESIAN_POINT('Ctrl Pts',(0.752592276483072,1.,-4.06026572221515));
#58313=CARTESIAN_POINT('Ctrl Pts',(0.750697720484036,1.,-4.06781267242378));
#58314=CARTESIAN_POINT('Ctrl Pts',(0.748767076680557,1.,-4.07535951056152));
#58315=CARTESIAN_POINT('Ctrl Pts',(0.746800631492315,1.,-4.08290608095642));
#58316=CARTESIAN_POINT('Ctrl Pts',(0.7447986497065,1.,-4.09045220253573));
#58317=CARTESIAN_POINT('Ctrl Pts',(0.742761369689841,1.,-4.09799769702611));
#58318=CARTESIAN_POINT('Ctrl Pts',(0.740688998553376,1.,-4.10554241757547));
#58319=CARTESIAN_POINT('Ctrl Pts',(0.738581708225843,1.,-4.11308626951927));
#58320=CARTESIAN_POINT('Ctrl Pts',(0.736439634331344,1.,-4.120629196238));
#58321=CARTESIAN_POINT('Ctrl Pts',(0.734698226764092,1.,-4.12666277570844));
#58322=CARTESIAN_POINT('Ctrl Pts',(0.733376589323546,1.,-4.13118752795207));
#58323=CARTESIAN_POINT('Ctrl Pts',(0.732488575135159,1.,-4.1342038373684));
#58324=CARTESIAN_POINT('Ctrl Pts',(0.73204283740062,1.,-4.13571194405636));
#58325=CARTESIAN_POINT('Origin',(0.73204283740062,0.,-4.13571194405636));
#58326=CARTESIAN_POINT('',(0.581791163835815,1.,-4.15950947128175));
#58327=CARTESIAN_POINT('Origin',(0.,0.,0.));
#58328=CARTESIAN_POINT('',(0.963899035117248,1.,-3.62400312501245));
#58329=CARTESIAN_POINT('Origin',(0.,1.,0.));
#58330=CARTESIAN_POINT('Ctrl Pts',(0.963899035117248,1.,-3.62400312501246));
#58331=CARTESIAN_POINT('Ctrl Pts',(0.963899035117248,0.666666666666667,
-3.62400312501246));
#58332=CARTESIAN_POINT('Ctrl Pts',(0.963899035117248,0.333333333333333,
-3.62400312501246));
#58333=CARTESIAN_POINT('Ctrl Pts',(0.963899035117248,-0.333333333333333,
-3.62400312501246));
#58334=CARTESIAN_POINT('Ctrl Pts',(0.963899035117249,-0.666666666666667,
-3.62400312501246));
#58335=CARTESIAN_POINT('Ctrl Pts',(0.963899035117249,-1.,-3.62400312501246));
#58336=CARTESIAN_POINT('Ctrl Pts',(1.22531898815164,-1.,-4.01728681790024));
#58337=CARTESIAN_POINT('Ctrl Pts',(1.22531898815164,1.,-4.01728681790024));
#58338=CARTESIAN_POINT('Ctrl Pts',(1.22423716681447,-1.,-4.0161454457032));
#58339=CARTESIAN_POINT('Ctrl Pts',(1.22423716681447,1.,-4.0161454457032));
#58340=CARTESIAN_POINT('Ctrl Pts',(1.22207656456199,-1.,-4.01386104434674));
#58341=CARTESIAN_POINT('Ctrl Pts',(1.22207656456199,1.,-4.01386104434674));
#58342=CARTESIAN_POINT('Ctrl Pts',(1.21884478244983,-1.,-4.01042947142681));
#58343=CARTESIAN_POINT('Ctrl Pts',(1.21884478244983,1.,-4.01042947142681));
#58344=CARTESIAN_POINT('Ctrl Pts',(1.21455398918813,-1.,-4.00584409524937));
#58345=CARTESIAN_POINT('Ctrl Pts',(1.21455398918813,1.,-4.00584409524937));
#58346=CARTESIAN_POINT('Ctrl Pts',(1.20922097030107,-1.,-4.00009577952534));
#58347=CARTESIAN_POINT('Ctrl Pts',(1.20922097030107,1.,-4.00009577952534));
#58348=CARTESIAN_POINT('Ctrl Pts',(1.2039185237544,-1.,-3.99433084800649));
#58349=CARTESIAN_POINT('Ctrl Pts',(1.2039185237544,1.,-3.99433084800649));
#58350=CARTESIAN_POINT('Ctrl Pts',(1.19864679609596,-1.,-3.98854928957287));
#58351=CARTESIAN_POINT('Ctrl Pts',(1.19864679609596,1.,-3.98854928957287));
#58352=CARTESIAN_POINT('Ctrl Pts',(1.19340598349307,-1.,-3.98275111052015));
#58353=CARTESIAN_POINT('Ctrl Pts',(1.19340598349307,1.,-3.98275111052015));
#58354=CARTESIAN_POINT('Ctrl Pts',(1.18819633715285,-1.,-3.97693634766926));
#58355=CARTESIAN_POINT('Ctrl Pts',(1.18819633715285,1.,-3.97693634766926));
#58356=CARTESIAN_POINT('Ctrl Pts',(1.18301815039596,-1.,-3.9711050516465));
#58357=CARTESIAN_POINT('Ctrl Pts',(1.18301815039596,1.,-3.9711050516465));
#58358=CARTESIAN_POINT('Ctrl Pts',(1.17787174135445,-1.,-3.96525726357682));
#58359=CARTESIAN_POINT('Ctrl Pts',(1.17787174135445,1.,-3.96525726357682));
#58360=CARTESIAN_POINT('Ctrl Pts',(1.17275743590327,-1.,-3.95939299213164));
#58361=CARTESIAN_POINT('Ctrl Pts',(1.17275743590327,1.,-3.95939299213164));
#58362=CARTESIAN_POINT('Ctrl Pts',(1.16767555244495,-1.,-3.95351219510062));
#58363=CARTESIAN_POINT('Ctrl Pts',(1.16767555244495,1.,-3.95351219510062));
#58364=CARTESIAN_POINT('Ctrl Pts',(1.16262637999261,-1.,-3.9476147478092));
#58365=CARTESIAN_POINT('Ctrl Pts',(1.16262637999261,1.,-3.9476147478092));
#58366=CARTESIAN_POINT('Ctrl Pts',(1.1576101834106,-1.,-3.94170046685542));
#58367=CARTESIAN_POINT('Ctrl Pts',(1.1576101834106,1.,-3.94170046685542));
#58368=CARTESIAN_POINT('Ctrl Pts',(1.1526272271639,-1.,-3.9357691705651));
#58369=CARTESIAN_POINT('Ctrl Pts',(1.1526272271639,1.,-3.9357691705651));
#58370=CARTESIAN_POINT('Ctrl Pts',(1.14767779451147,-1.,-3.92982073294334));
#58371=CARTESIAN_POINT('Ctrl Pts',(1.14767779451147,1.,-3.92982073294334));
#58372=CARTESIAN_POINT('Ctrl Pts',(1.14276220561575,-1.,-3.92385513133937));
#58373=CARTESIAN_POINT('Ctrl Pts',(1.14276220561575,1.,-3.92385513133937));
#58374=CARTESIAN_POINT('Ctrl Pts',(1.13788084225511,-1.,-3.91787251936688));
#58375=CARTESIAN_POINT('Ctrl Pts',(1.13788084225511,1.,-3.91787251936688));
#58376=CARTESIAN_POINT('Ctrl Pts',(1.13303414693849,-1.,-3.91187321145495));
#58377=CARTESIAN_POINT('Ctrl Pts',(1.13303414693849,1.,-3.91187321145495));
#58378=CARTESIAN_POINT('Ctrl Pts',(1.12822258281518,-1.,-3.90585753318622));
#58379=CARTESIAN_POINT('Ctrl Pts',(1.12822258281518,1.,-3.90585753318622));
#58380=CARTESIAN_POINT('Ctrl Pts',(1.12344660099029,-1.,-3.89982569749978));
#58381=CARTESIAN_POINT('Ctrl Pts',(1.12344660099029,1.,-3.89982569749978));
#58382=CARTESIAN_POINT('Ctrl Pts',(1.11870660794609,-1.,-3.89377768340362));
#58383=CARTESIAN_POINT('Ctrl Pts',(1.11870660794609,1.,-3.89377768340362));
#58384=CARTESIAN_POINT('Ctrl Pts',(1.11400292434447,-1.,-3.88771308285229));
#58385=CARTESIAN_POINT('Ctrl Pts',(1.11400292434447,1.,-3.88771308285229));
#58386=CARTESIAN_POINT('Ctrl Pts',(1.10933577224029,-1.,-3.88163105531791));
#58387=CARTESIAN_POINT('Ctrl Pts',(1.10933577224029,1.,-3.88163105531791));
#58388=CARTESIAN_POINT('Ctrl Pts',(1.10470536603303,-1.,-3.87553067187566));
#58389=CARTESIAN_POINT('Ctrl Pts',(1.10470536603303,1.,-3.87553067187566));
#58390=CARTESIAN_POINT('Ctrl Pts',(1.10011198761202,-1.,-3.86941120134872));
#58391=CARTESIAN_POINT('Ctrl Pts',(1.10011198761202,1.,-3.86941120134872));
#58392=CARTESIAN_POINT('Ctrl Pts',(1.09555606505012,-1.,-3.86327241021242));
#58393=CARTESIAN_POINT('Ctrl Pts',(1.09555606505012,1.,-3.86327241021242));
#58394=CARTESIAN_POINT('Ctrl Pts',(1.09103825516288,-1.,-3.85711487933911));
#58395=CARTESIAN_POINT('Ctrl Pts',(1.09103825516288,1.,-3.85711487933911));
#58396=CARTESIAN_POINT('Ctrl Pts',(1.08655950846377,-1.,-3.85094025222691));
#58397=CARTESIAN_POINT('Ctrl Pts',(1.08655950846377,1.,-3.85094025222691));
#58398=CARTESIAN_POINT('Ctrl Pts',(1.08212087917986,-1.,-3.84475048030615));
#58399=CARTESIAN_POINT('Ctrl Pts',(1.08212087917986,1.,-3.84475048030615));
#58400=CARTESIAN_POINT('Ctrl Pts',(1.07772335353856,-1.,-3.83854714117486));
#58401=CARTESIAN_POINT('Ctrl Pts',(1.07772335353856,1.,-3.83854714117486));
#58402=CARTESIAN_POINT('Ctrl Pts',(1.0733676663346,-1.,-3.83233071195145));
#58403=CARTESIAN_POINT('Ctrl Pts',(1.0733676663346,1.,-3.83233071195145));
#58404=CARTESIAN_POINT('Ctrl Pts',(1.0690541318036,-1.,-3.82609989967278));
#58405=CARTESIAN_POINT('Ctrl Pts',(1.0690541318036,1.,-3.82609989967278));
#58406=CARTESIAN_POINT('Ctrl Pts',(1.06478244038931,-1.,-3.81985083953012));
#58407=CARTESIAN_POINT('Ctrl Pts',(1.06478244038931,1.,-3.81985083953012));
#58408=CARTESIAN_POINT('Ctrl Pts',(1.06055206187298,-1.,-3.81357866117485));
#58409=CARTESIAN_POINT('Ctrl Pts',(1.06055206187298,1.,-3.81357866117485));
#58410=CARTESIAN_POINT('Ctrl Pts',(1.05636266918643,-1.,-3.80727913637784));
#58411=CARTESIAN_POINT('Ctrl Pts',(1.05636266918643,1.,-3.80727913637784));
#58412=CARTESIAN_POINT('Ctrl Pts',(1.05221457990015,-1.,-3.80095039790678));
#58413=CARTESIAN_POINT('Ctrl Pts',(1.05221457990015,1.,-3.80095039790678));
#58414=CARTESIAN_POINT('Ctrl Pts',(1.04810913267641,-1.,-3.79459440308793));
#58415=CARTESIAN_POINT('Ctrl Pts',(1.04810913267641,1.,-3.79459440308793));
#58416=CARTESIAN_POINT('Ctrl Pts',(1.04404924374426,-1.,-3.78821910787195));
#58417=CARTESIAN_POINT('Ctrl Pts',(1.04404924374426,1.,-3.78821910787195));
#58418=CARTESIAN_POINT('Ctrl Pts',(1.04003862055804,-1.,-3.78183535008192));
#58419=CARTESIAN_POINT('Ctrl Pts',(1.04003862055804,1.,-3.78183535008192));
#58420=CARTESIAN_POINT('Ctrl Pts',(1.03608074678013,-1.,-3.77545283140445));
#58421=CARTESIAN_POINT('Ctrl Pts',(1.03608074678013,1.,-3.77545283140445));
#58422=CARTESIAN_POINT('Ctrl Pts',(1.0321778660492,-1.,-3.76907609832522));
#58423=CARTESIAN_POINT('Ctrl Pts',(1.0321778660492,1.,-3.76907609832522));
#58424=CARTESIAN_POINT('Ctrl Pts',(1.02833014458181,-1.,-3.76270122291232));
#58425=CARTESIAN_POINT('Ctrl Pts',(1.02833014458181,1.,-3.76270122291232));
#58426=CARTESIAN_POINT('Ctrl Pts',(1.0245342944466,-1.,-3.75631037456194));
#58427=CARTESIAN_POINT('Ctrl Pts',(1.0245342944466,1.,-3.75631037456194));
#58428=CARTESIAN_POINT('Ctrl Pts',(1.02078510487428,-1.,-3.74987777155834));
#58429=CARTESIAN_POINT('Ctrl Pts',(1.02078510487428,1.,-3.74987777155834));
#58430=CARTESIAN_POINT('Ctrl Pts',(1.01707794311079,-1.,-3.74337942504959));
#58431=CARTESIAN_POINT('Ctrl Pts',(1.01707794311079,1.,-3.74337942504959));
#58432=CARTESIAN_POINT('Ctrl Pts',(1.01341114319903,-1.,-3.73680245055734));
#58433=CARTESIAN_POINT('Ctrl Pts',(1.01341114319903,1.,-3.73680245055734));
#58434=CARTESIAN_POINT('Ctrl Pts',(1.00978798539496,-1.,-3.73015276704426));
#58435=CARTESIAN_POINT('Ctrl Pts',(1.00978798539496,1.,-3.73015276704426));
#58436=CARTESIAN_POINT('Ctrl Pts',(1.0062200073571,-1.,-3.72346803750596));
#58437=CARTESIAN_POINT('Ctrl Pts',(1.0062200073571,1.,-3.72346803750596));
#58438=CARTESIAN_POINT('Ctrl Pts',(1.00272423396822,-1.,-3.71680667125119));
#58439=CARTESIAN_POINT('Ctrl Pts',(1.00272423396822,1.,-3.71680667125119));
#58440=CARTESIAN_POINT('Ctrl Pts',(0.99931726075653,-1.,-3.71022439713938));
#58441=CARTESIAN_POINT('Ctrl Pts',(0.99931726075653,1.,-3.71022439713938));
#58442=CARTESIAN_POINT('Ctrl Pts',(0.996009819772518,-1.,-3.70375282282138));
#58443=CARTESIAN_POINT('Ctrl Pts',(0.996009819772518,1.,-3.70375282282138));
#58444=CARTESIAN_POINT('Ctrl Pts',(0.99280221833201,-1.,-3.69738123415662));
#58445=CARTESIAN_POINT('Ctrl Pts',(0.99280221833201,1.,-3.69738123415662));
#58446=CARTESIAN_POINT('Ctrl Pts',(0.989676715398558,-1.,-3.69102682138847));
#58447=CARTESIAN_POINT('Ctrl Pts',(0.989676715398558,1.,-3.69102682138847));
#58448=CARTESIAN_POINT('Ctrl Pts',(0.986602639863837,-1.,-3.68455317926068));
#58449=CARTESIAN_POINT('Ctrl Pts',(0.986602639863837,1.,-3.68455317926068));
#58450=CARTESIAN_POINT('Ctrl Pts',(0.983550791470419,-1.,-3.67782408841715));
#58451=CARTESIAN_POINT('Ctrl Pts',(0.983550791470419,1.,-3.67782408841715));
#58452=CARTESIAN_POINT('Ctrl Pts',(0.980505922458267,-1.,-3.67074983340361));
#58453=CARTESIAN_POINT('Ctrl Pts',(0.980505922458267,1.,-3.67074983340361));
#58454=CARTESIAN_POINT('Ctrl Pts',(0.977478312751618,-1.,-3.66333049637475));
#58455=CARTESIAN_POINT('Ctrl Pts',(0.977478312751618,1.,-3.66333049637475));
#58456=CARTESIAN_POINT('Ctrl Pts',(0.974519971354848,-1.,-3.65571576735126));
#58457=CARTESIAN_POINT('Ctrl Pts',(0.974519971354848,1.,-3.65571576735126));
#58458=CARTESIAN_POINT('Ctrl Pts',(0.971722122061341,-1.,-3.64819756447455));
#58459=CARTESIAN_POINT('Ctrl Pts',(0.971722122061341,1.,-3.64819756447455));
#58460=CARTESIAN_POINT('Ctrl Pts',(0.969195124675865,-1.,-3.64113946505766));
#58461=CARTESIAN_POINT('Ctrl Pts',(0.969195124675865,1.,-3.64113946505766));
#58462=CARTESIAN_POINT('Ctrl Pts',(0.967052554541385,-1.,-3.63492122081143));
#58463=CARTESIAN_POINT('Ctrl Pts',(0.967052554541385,1.,-3.63492122081143));
#58464=CARTESIAN_POINT('Ctrl Pts',(0.965395153165293,-1.,-3.62988252139846));
#58465=CARTESIAN_POINT('Ctrl Pts',(0.965395153165293,1.,-3.62988252139846));
#58466=CARTESIAN_POINT('Ctrl Pts',(0.964291001273287,-1.,-3.62625391254797));
#58467=CARTESIAN_POINT('Ctrl Pts',(0.964291001273287,1.,-3.62625391254797));
#58468=CARTESIAN_POINT('Ctrl Pts',(0.963875774530619,-1.,-3.6245656860652));
#58469=CARTESIAN_POINT('Ctrl Pts',(0.963875774530619,1.,-3.6245656860652));
#58470=CARTESIAN_POINT('Ctrl Pts',(0.963832486395051,-1.,-3.62399933639915));
#58471=CARTESIAN_POINT('Ctrl Pts',(0.963832486395051,1.,-3.62399933639915));
#58472=CARTESIAN_POINT('Ctrl Pts',(0.963922720982193,-1.,-3.62393257642052));
#58473=CARTESIAN_POINT('Ctrl Pts',(0.963922720982193,1.,-3.62393257642052));
#58474=CARTESIAN_POINT('Ctrl Pts',(0.963997613369571,-1.,-3.62397690409552));
#58475=CARTESIAN_POINT('Ctrl Pts',(0.963997613369571,1.,-3.62397690409552));
#58476=CARTESIAN_POINT('',(1.22531898815164,1.,-4.01728681790024));
#58477=CARTESIAN_POINT('Ctrl Pts',(1.22531898815164,1.,-4.01728681790024));
#58478=CARTESIAN_POINT('Ctrl Pts',(1.22423716681447,1.,-4.0161454457032));
#58479=CARTESIAN_POINT('Ctrl Pts',(1.22207656456199,1.,-4.01386104434674));
#58480=CARTESIAN_POINT('Ctrl Pts',(1.21884478244983,1.,-4.01042947142681));
#58481=CARTESIAN_POINT('Ctrl Pts',(1.21455398918813,1.,-4.00584409524937));
#58482=CARTESIAN_POINT('Ctrl Pts',(1.20922097030107,1.,-4.00009577952534));
#58483=CARTESIAN_POINT('Ctrl Pts',(1.2039185237544,1.,-3.99433084800649));
#58484=CARTESIAN_POINT('Ctrl Pts',(1.19864679609596,1.,-3.98854928957287));
#58485=CARTESIAN_POINT('Ctrl Pts',(1.19340598349307,1.,-3.98275111052015));
#58486=CARTESIAN_POINT('Ctrl Pts',(1.18819633715285,1.,-3.97693634766926));
#58487=CARTESIAN_POINT('Ctrl Pts',(1.18301815039596,1.,-3.9711050516465));
#58488=CARTESIAN_POINT('Ctrl Pts',(1.17787174135445,1.,-3.96525726357682));
#58489=CARTESIAN_POINT('Ctrl Pts',(1.17275743590327,1.,-3.95939299213164));
#58490=CARTESIAN_POINT('Ctrl Pts',(1.16767555244495,1.,-3.95351219510062));
#58491=CARTESIAN_POINT('Ctrl Pts',(1.16262637999261,1.,-3.9476147478092));
#58492=CARTESIAN_POINT('Ctrl Pts',(1.1576101834106,1.,-3.94170046685542));
#58493=CARTESIAN_POINT('Ctrl Pts',(1.1526272271639,1.,-3.9357691705651));
#58494=CARTESIAN_POINT('Ctrl Pts',(1.14767779451147,1.,-3.92982073294334));
#58495=CARTESIAN_POINT('Ctrl Pts',(1.14276220561575,1.,-3.92385513133937));
#58496=CARTESIAN_POINT('Ctrl Pts',(1.13788084225511,1.,-3.91787251936688));
#58497=CARTESIAN_POINT('Ctrl Pts',(1.13303414693849,1.,-3.91187321145495));
#58498=CARTESIAN_POINT('Ctrl Pts',(1.12822258281518,1.,-3.90585753318622));
#58499=CARTESIAN_POINT('Ctrl Pts',(1.12344660099029,1.,-3.89982569749978));
#58500=CARTESIAN_POINT('Ctrl Pts',(1.11870660794609,1.,-3.89377768340362));
#58501=CARTESIAN_POINT('Ctrl Pts',(1.11400292434447,1.,-3.88771308285229));
#58502=CARTESIAN_POINT('Ctrl Pts',(1.10933577224029,1.,-3.88163105531791));
#58503=CARTESIAN_POINT('Ctrl Pts',(1.10470536603303,1.,-3.87553067187566));
#58504=CARTESIAN_POINT('Ctrl Pts',(1.10011198761202,1.,-3.86941120134872));
#58505=CARTESIAN_POINT('Ctrl Pts',(1.09555606505012,1.,-3.86327241021242));
#58506=CARTESIAN_POINT('Ctrl Pts',(1.09103825516288,1.,-3.85711487933911));
#58507=CARTESIAN_POINT('Ctrl Pts',(1.08655950846377,1.,-3.85094025222691));
#58508=CARTESIAN_POINT('Ctrl Pts',(1.08212087917986,1.,-3.84475048030615));
#58509=CARTESIAN_POINT('Ctrl Pts',(1.07772335353856,1.,-3.83854714117486));
#58510=CARTESIAN_POINT('Ctrl Pts',(1.0733676663346,1.,-3.83233071195145));
#58511=CARTESIAN_POINT('Ctrl Pts',(1.0690541318036,1.,-3.82609989967278));
#58512=CARTESIAN_POINT('Ctrl Pts',(1.06478244038931,1.,-3.81985083953012));
#58513=CARTESIAN_POINT('Ctrl Pts',(1.06055206187298,1.,-3.81357866117485));
#58514=CARTESIAN_POINT('Ctrl Pts',(1.05636266918643,1.,-3.80727913637784));
#58515=CARTESIAN_POINT('Ctrl Pts',(1.05221457990015,1.,-3.80095039790678));
#58516=CARTESIAN_POINT('Ctrl Pts',(1.04810913267641,1.,-3.79459440308793));
#58517=CARTESIAN_POINT('Ctrl Pts',(1.04404924374426,1.,-3.78821910787195));
#58518=CARTESIAN_POINT('Ctrl Pts',(1.04003862055804,1.,-3.78183535008192));
#58519=CARTESIAN_POINT('Ctrl Pts',(1.03608074678013,1.,-3.77545283140445));
#58520=CARTESIAN_POINT('Ctrl Pts',(1.0321778660492,1.,-3.76907609832522));
#58521=CARTESIAN_POINT('Ctrl Pts',(1.02833014458181,1.,-3.76270122291232));
#58522=CARTESIAN_POINT('Ctrl Pts',(1.0245342944466,1.,-3.75631037456194));
#58523=CARTESIAN_POINT('Ctrl Pts',(1.02078510487428,1.,-3.74987777155834));
#58524=CARTESIAN_POINT('Ctrl Pts',(1.01707794311079,1.,-3.74337942504959));
#58525=CARTESIAN_POINT('Ctrl Pts',(1.01341114319903,1.,-3.73680245055734));
#58526=CARTESIAN_POINT('Ctrl Pts',(1.00978798539496,1.,-3.73015276704426));
#58527=CARTESIAN_POINT('Ctrl Pts',(1.0062200073571,1.,-3.72346803750596));
#58528=CARTESIAN_POINT('Ctrl Pts',(1.00272423396822,1.,-3.71680667125119));
#58529=CARTESIAN_POINT('Ctrl Pts',(0.99931726075653,1.,-3.71022439713938));
#58530=CARTESIAN_POINT('Ctrl Pts',(0.996009819772518,1.,-3.70375282282138));
#58531=CARTESIAN_POINT('Ctrl Pts',(0.99280221833201,1.,-3.69738123415662));
#58532=CARTESIAN_POINT('Ctrl Pts',(0.989676715398558,1.,-3.69102682138847));
#58533=CARTESIAN_POINT('Ctrl Pts',(0.986602639863837,1.,-3.68455317926068));
#58534=CARTESIAN_POINT('Ctrl Pts',(0.983550791470419,1.,-3.67782408841715));
#58535=CARTESIAN_POINT('Ctrl Pts',(0.980505922458267,1.,-3.67074983340361));
#58536=CARTESIAN_POINT('Ctrl Pts',(0.977478312751618,1.,-3.66333049637475));
#58537=CARTESIAN_POINT('Ctrl Pts',(0.974519971354848,1.,-3.65571576735126));
#58538=CARTESIAN_POINT('Ctrl Pts',(0.971722122061341,1.,-3.64819756447455));
#58539=CARTESIAN_POINT('Ctrl Pts',(0.969195124675865,1.,-3.64113946505766));
#58540=CARTESIAN_POINT('Ctrl Pts',(0.967052554541385,1.,-3.63492122081143));
#58541=CARTESIAN_POINT('Ctrl Pts',(0.965395153165293,1.,-3.62988252139846));
#58542=CARTESIAN_POINT('Ctrl Pts',(0.964373850166457,1.,-3.62652618145335));
#58543=CARTESIAN_POINT('Ctrl Pts',(0.963957782642843,1.,-3.62489305727662));
#58544=CARTESIAN_POINT('Ctrl Pts',(0.963861297423241,1.,-3.62424461507588));
#58545=CARTESIAN_POINT('Ctrl Pts',(0.963880158555582,1.,-3.6240482887845));
#58546=CARTESIAN_POINT('Ctrl Pts',(0.963899035117249,1.,-3.62400312501246));
#58547=CARTESIAN_POINT('',(1.22531898815164,0.,-4.01728681790024));
#58548=CARTESIAN_POINT('Ctrl Pts',(1.35022972712301,-1.,-3.49848248301936));
#58549=CARTESIAN_POINT('Ctrl Pts',(1.35022972712301,1.,-3.49848248301936));
#58550=CARTESIAN_POINT('Ctrl Pts',(1.35026426118402,-1.,-3.4984026005375));
#58551=CARTESIAN_POINT('Ctrl Pts',(1.35026426118402,1.,-3.4984026005375));
#58552=CARTESIAN_POINT('Ctrl Pts',(1.35037650303019,-1.,-3.49840357193736));
#58553=CARTESIAN_POINT('Ctrl Pts',(1.35037650303019,1.,-3.49840357193736));
#58554=CARTESIAN_POINT('Ctrl Pts',(1.35067437417483,-1.,-3.49888720257132));
#58555=CARTESIAN_POINT('Ctrl Pts',(1.35067437417483,1.,-3.49888720257132));
#58556=CARTESIAN_POINT('Ctrl Pts',(1.3513307633124,-1.,-3.5004970706414));
#58557=CARTESIAN_POINT('Ctrl Pts',(1.3513307633124,1.,-3.5004970706414));
#58558=CARTESIAN_POINT('Ctrl Pts',(1.35257032843486,-1.,-3.50408168106261));
#58559=CARTESIAN_POINT('Ctrl Pts',(1.35257032843486,1.,-3.50408168106261));
#58560=CARTESIAN_POINT('Ctrl Pts',(1.35419113575956,-1.,-3.50913227059999));
#58561=CARTESIAN_POINT('Ctrl Pts',(1.35419113575956,1.,-3.50913227059999));
#58562=CARTESIAN_POINT('Ctrl Pts',(1.35611275237152,-1.,-3.51542230699556));
#58563=CARTESIAN_POINT('Ctrl Pts',(1.35611275237152,1.,-3.51542230699556));
#58564=CARTESIAN_POINT('Ctrl Pts',(1.35821701528836,-1.,-3.52261776116748));
#58565=CARTESIAN_POINT('Ctrl Pts',(1.35821701528836,1.,-3.52261776116748));
#58566=CARTESIAN_POINT('Ctrl Pts',(1.36037259643734,-1.,-3.530344649616));
#58567=CARTESIAN_POINT('Ctrl Pts',(1.36037259643734,1.,-3.530344649616));
#58568=CARTESIAN_POINT('Ctrl Pts',(1.36245507339307,-1.,-3.53824396424961));
#58569=CARTESIAN_POINT('Ctrl Pts',(1.36245507339307,1.,-3.53824396424961));
#58570=CARTESIAN_POINT('Ctrl Pts',(1.36436666257597,-1.,-3.54602591832973));
#58571=CARTESIAN_POINT('Ctrl Pts',(1.36436666257597,1.,-3.54602591832973));
#58572=CARTESIAN_POINT('Ctrl Pts',(1.3660614545677,-1.,-3.55353883995949));
#58573=CARTESIAN_POINT('Ctrl Pts',(1.3660614545677,1.,-3.55353883995949));
#58574=CARTESIAN_POINT('Ctrl Pts',(1.36754771771233,-1.,-3.56077662028649));
#58575=CARTESIAN_POINT('Ctrl Pts',(1.36754771771233,1.,-3.56077662028649));
#58576=CARTESIAN_POINT('Ctrl Pts',(1.36886584973389,-1.,-3.5678208030466));
#58577=CARTESIAN_POINT('Ctrl Pts',(1.36886584973389,1.,-3.5678208030466));
#58578=CARTESIAN_POINT('Ctrl Pts',(1.37007229485659,-1.,-3.57479875549486));
#58579=CARTESIAN_POINT('Ctrl Pts',(1.37007229485659,1.,-3.57479875549486));
#58580=CARTESIAN_POINT('Ctrl Pts',(1.37122241663062,-1.,-3.58183885982715));
#58581=CARTESIAN_POINT('Ctrl Pts',(1.37122241663062,1.,-3.58183885982715));
#58582=CARTESIAN_POINT('Ctrl Pts',(1.37235053660976,-1.,-3.58901853846365));
#58583=CARTESIAN_POINT('Ctrl Pts',(1.37235053660976,1.,-3.58901853846365));
#58584=CARTESIAN_POINT('Ctrl Pts',(1.37346320103157,-1.,-3.59634627869048));
#58585=CARTESIAN_POINT('Ctrl Pts',(1.37346320103157,1.,-3.59634627869048));
#58586=CARTESIAN_POINT('Ctrl Pts',(1.37455051379623,-1.,-3.60379020123988));
#58587=CARTESIAN_POINT('Ctrl Pts',(1.37455051379623,1.,-3.60379020123988));
#58588=CARTESIAN_POINT('Ctrl Pts',(1.37559314436634,-1.,-3.61129546591064));
#58589=CARTESIAN_POINT('Ctrl Pts',(1.37559314436634,1.,-3.61129546591064));
#58590=CARTESIAN_POINT('Ctrl Pts',(1.37657053403107,-1.,-3.61880481160421));
#58591=CARTESIAN_POINT('Ctrl Pts',(1.37657053403107,1.,-3.61880481160421));
#58592=CARTESIAN_POINT('Ctrl Pts',(1.37746987919881,-1.,-3.62628098665145));
#58593=CARTESIAN_POINT('Ctrl Pts',(1.37746987919881,1.,-3.62628098665145));
#58594=CARTESIAN_POINT('Ctrl Pts',(1.37829035457339,-1.,-3.63371727442486));
#58595=CARTESIAN_POINT('Ctrl Pts',(1.37829035457339,1.,-3.63371727442486));
#58596=CARTESIAN_POINT('Ctrl Pts',(1.37903818567359,-1.,-3.64112507791141));
#58597=CARTESIAN_POINT('Ctrl Pts',(1.37903818567359,1.,-3.64112507791141));
#58598=CARTESIAN_POINT('Ctrl Pts',(1.37972372481603,-1.,-3.64852652756456));
#58599=CARTESIAN_POINT('Ctrl Pts',(1.37972372481603,1.,-3.64852652756456));
#58600=CARTESIAN_POINT('Ctrl Pts',(1.38035791051212,-1.,-3.6559455440439));
#58601=CARTESIAN_POINT('Ctrl Pts',(1.38035791051212,1.,-3.6559455440439));
#58602=CARTESIAN_POINT('Ctrl Pts',(1.38094856333552,-1.,-3.66339848520857));
#58603=CARTESIAN_POINT('Ctrl Pts',(1.38094856333552,1.,-3.66339848520857));
#58604=CARTESIAN_POINT('Ctrl Pts',(1.38149812653868,-1.,-3.67088843112262));
#58605=CARTESIAN_POINT('Ctrl Pts',(1.38149812653868,1.,-3.67088843112262));
#58606=CARTESIAN_POINT('Ctrl Pts',(1.3820057429062,-1.,-3.67841038482414));
#58607=CARTESIAN_POINT('Ctrl Pts',(1.3820057429062,1.,-3.67841038482414));
#58608=CARTESIAN_POINT('Ctrl Pts',(1.38246852827182,-1.,-3.68595444983838));
#58609=CARTESIAN_POINT('Ctrl Pts',(1.38246852827182,1.,-3.68595444983838));
#58610=CARTESIAN_POINT('Ctrl Pts',(1.3828831117165,-1.,-3.69350967899526));
#58611=CARTESIAN_POINT('Ctrl Pts',(1.3828831117165,1.,-3.69350967899526));
#58612=CARTESIAN_POINT('Ctrl Pts',(1.38324717612865,-1.,-3.701067921679));
#58613=CARTESIAN_POINT('Ctrl Pts',(1.38324717612865,1.,-3.701067921679));
#58614=CARTESIAN_POINT('Ctrl Pts',(1.38356065402124,-1.,-3.70862680753347));
#58615=CARTESIAN_POINT('Ctrl Pts',(1.38356065402124,1.,-3.70862680753347));
#58616=CARTESIAN_POINT('Ctrl Pts',(1.38382489984586,-1.,-3.7161876605181));
#58617=CARTESIAN_POINT('Ctrl Pts',(1.38382489984586,1.,-3.7161876605181));
#58618=CARTESIAN_POINT('Ctrl Pts',(1.3840421342895,-1.,-3.72375409358803));
#58619=CARTESIAN_POINT('Ctrl Pts',(1.3840421342895,1.,-3.72375409358803));
#58620=CARTESIAN_POINT('Ctrl Pts',(1.38421479111531,-1.,-3.73133035859282));
#58621=CARTESIAN_POINT('Ctrl Pts',(1.38421479111531,1.,-3.73133035859282));
#58622=CARTESIAN_POINT('Ctrl Pts',(1.38434489156458,-1.,-3.73891976418104));
#58623=CARTESIAN_POINT('Ctrl Pts',(1.38434489156458,1.,-3.73891976418104));
#58624=CARTESIAN_POINT('Ctrl Pts',(1.38443344984394,-1.,-3.74652317167876));
#58625=CARTESIAN_POINT('Ctrl Pts',(1.38443344984394,1.,-3.74652317167876));
#58626=CARTESIAN_POINT('Ctrl Pts',(1.38448077997163,-1.,-3.7541397631875));
#58627=CARTESIAN_POINT('Ctrl Pts',(1.38448077997163,1.,-3.7541397631875));
#58628=CARTESIAN_POINT('Ctrl Pts',(1.3844867525335,-1.,-3.76176768271367));
#58629=CARTESIAN_POINT('Ctrl Pts',(1.3844867525335,1.,-3.76176768271367));
#58630=CARTESIAN_POINT('Ctrl Pts',(1.38445107339518,-1.,-3.76940473185779));
#58631=CARTESIAN_POINT('Ctrl Pts',(1.38445107339518,1.,-3.76940473185779));
#58632=CARTESIAN_POINT('Ctrl Pts',(1.38437354551428,-1.,-3.77704902230418));
#58633=CARTESIAN_POINT('Ctrl Pts',(1.38437354551428,1.,-3.77704902230418));
#58634=CARTESIAN_POINT('Ctrl Pts',(1.38425435883756,-1.,-3.78469969805082));
#58635=CARTESIAN_POINT('Ctrl Pts',(1.38425435883756,1.,-3.78469969805082));
#58636=CARTESIAN_POINT('Ctrl Pts',(1.38409399694566,-1.,-3.79235669640841));
#58637=CARTESIAN_POINT('Ctrl Pts',(1.38409399694566,1.,-3.79235669640841));
#58638=CARTESIAN_POINT('Ctrl Pts',(1.38389311766682,-1.,-3.80002044322111));
#58639=CARTESIAN_POINT('Ctrl Pts',(1.38389311766682,1.,-3.80002044322111));
#58640=CARTESIAN_POINT('Ctrl Pts',(1.3836524404622,-1.,-3.80769156398411));
#58641=CARTESIAN_POINT('Ctrl Pts',(1.3836524404622,1.,-3.80769156398411));
#58642=CARTESIAN_POINT('Ctrl Pts',(1.38337263902782,-1.,-3.81537060817811));
#58643=CARTESIAN_POINT('Ctrl Pts',(1.38337263902782,1.,-3.81537060817811));
#58644=CARTESIAN_POINT('Ctrl Pts',(1.38305421262763,-1.,-3.82305771743829));
#58645=CARTESIAN_POINT('Ctrl Pts',(1.38305421262763,1.,-3.82305771743829));
#58646=CARTESIAN_POINT('Ctrl Pts',(1.38269750245138,-1.,-3.8307526698229));
#58647=CARTESIAN_POINT('Ctrl Pts',(1.38269750245138,1.,-3.8307526698229));
#58648=CARTESIAN_POINT('Ctrl Pts',(1.38230274828821,-1.,-3.83845502790746));
#58649=CARTESIAN_POINT('Ctrl Pts',(1.38230274828821,1.,-3.83845502790746));
#58650=CARTESIAN_POINT('Ctrl Pts',(1.38187013346109,-1.,-3.84616425605764));
#58651=CARTESIAN_POINT('Ctrl Pts',(1.38187013346109,1.,-3.84616425605764));
#58652=CARTESIAN_POINT('Ctrl Pts',(1.38139983115049,-1.,-3.85387983979481));
#58653=CARTESIAN_POINT('Ctrl Pts',(1.38139983115049,1.,-3.85387983979481));
#58654=CARTESIAN_POINT('Ctrl Pts',(1.38089205992989,-1.,-3.86160143043959));
#58655=CARTESIAN_POINT('Ctrl Pts',(1.38089205992989,1.,-3.86160143043959));
#58656=CARTESIAN_POINT('Ctrl Pts',(1.38034709213014,-1.,-3.86932885813068));
#58657=CARTESIAN_POINT('Ctrl Pts',(1.38034709213014,1.,-3.86932885813068));
#58658=CARTESIAN_POINT('Ctrl Pts',(1.37976523097073,-1.,-3.87706205830532));
#58659=CARTESIAN_POINT('Ctrl Pts',(1.37976523097073,1.,-3.87706205830532));
#58660=CARTESIAN_POINT('Ctrl Pts',(1.37914679719383,-1.,-3.88480102249278));
#58661=CARTESIAN_POINT('Ctrl Pts',(1.37914679719383,1.,-3.88480102249278));
#58662=CARTESIAN_POINT('Ctrl Pts',(1.3784921128802,-1.,-3.89254574338496));
#58663=CARTESIAN_POINT('Ctrl Pts',(1.3784921128802,1.,-3.89254574338496));
#58664=CARTESIAN_POINT('Ctrl Pts',(1.37780148512792,-1.,-3.90029615196727));
#58665=CARTESIAN_POINT('Ctrl Pts',(1.37780148512792,1.,-3.90029615196727));
#58666=CARTESIAN_POINT('Ctrl Pts',(1.3770751963402,-1.,-3.90805209523486));
#58667=CARTESIAN_POINT('Ctrl Pts',(1.3770751963402,1.,-3.90805209523486));
#58668=CARTESIAN_POINT('Ctrl Pts',(1.37631350505797,-1.,-3.91581337462644));
#58669=CARTESIAN_POINT('Ctrl Pts',(1.37631350505797,1.,-3.91581337462644));
#58670=CARTESIAN_POINT('Ctrl Pts',(1.37551664448242,-1.,-3.92357976987672));
#58671=CARTESIAN_POINT('Ctrl Pts',(1.37551664448242,1.,-3.92357976987672));
#58672=CARTESIAN_POINT('Ctrl Pts',(1.37468482215751,-1.,-3.93135106761844));
#58673=CARTESIAN_POINT('Ctrl Pts',(1.37468482215751,1.,-3.93135106761844));
#58674=CARTESIAN_POINT('Ctrl Pts',(1.37381821967165,-1.,-3.93912709040818));
#58675=CARTESIAN_POINT('Ctrl Pts',(1.37381821967165,1.,-3.93912709040818));
#58676=CARTESIAN_POINT('Ctrl Pts',(1.37291699202807,-1.,-3.94690771785133));
#58677=CARTESIAN_POINT('Ctrl Pts',(1.37291699202807,1.,-3.94690771785133));
#58678=CARTESIAN_POINT('Ctrl Pts',(1.37198126432386,-1.,-3.95469287280914));
#58679=CARTESIAN_POINT('Ctrl Pts',(1.37198126432386,1.,-3.95469287280914));
#58680=CARTESIAN_POINT('Ctrl Pts',(1.3712051561502,-1.,-3.96092458506535));
#58681=CARTESIAN_POINT('Ctrl Pts',(1.3712051561502,1.,-3.96092458506535));
#58682=CARTESIAN_POINT('Ctrl Pts',(1.37060761745635,-1.,-3.96560037974645));
#58683=CARTESIAN_POINT('Ctrl Pts',(1.37060761745635,1.,-3.96560037974645));
#58684=CARTESIAN_POINT('Ctrl Pts',(1.37020239094614,-1.,-3.9687184694131));
#58685=CARTESIAN_POINT('Ctrl Pts',(1.37020239094614,1.,-3.9687184694131));
#58686=CARTESIAN_POINT('Ctrl Pts',(1.36999806084572,-1.,-3.97027773754922));
#58687=CARTESIAN_POINT('Ctrl Pts',(1.36999806084572,1.,-3.97027773754922));
#58688=CARTESIAN_POINT('',(1.35032489087101,1.,-3.4984457533445));
#58689=CARTESIAN_POINT('Ctrl Pts',(1.35032489087101,-1.,-3.4984457533445));
#58690=CARTESIAN_POINT('Ctrl Pts',(1.35032489087101,-0.666666666666667,
-3.4984457533445));
#58691=CARTESIAN_POINT('Ctrl Pts',(1.35032489087101,-0.333333333333333,
-3.4984457533445));
#58692=CARTESIAN_POINT('Ctrl Pts',(1.35032489087101,0.333333333333333,-3.4984457533445));
#58693=CARTESIAN_POINT('Ctrl Pts',(1.35032489087101,0.666666666666667,-3.4984457533445));
#58694=CARTESIAN_POINT('Ctrl Pts',(1.35032489087101,1.,-3.4984457533445));
#58695=CARTESIAN_POINT('',(1.36999806084572,1.,-3.97027773754922));
#58696=CARTESIAN_POINT('',(1.36999806084572,0.,-3.97027773754922));
#58697=CARTESIAN_POINT('Ctrl Pts',(1.35032489087101,1.,-3.49844575334451));
#58698=CARTESIAN_POINT('Ctrl Pts',(1.35036670892966,1.,-3.49847119623846));
#58699=CARTESIAN_POINT('Ctrl Pts',(1.35049736560527,1.,-3.49861894124827));
#58700=CARTESIAN_POINT('Ctrl Pts',(1.35080045218587,1.,-3.49920025459723));
#58701=CARTESIAN_POINT('Ctrl Pts',(1.35142377279517,1.,-3.50076603816491));
#58702=CARTESIAN_POINT('Ctrl Pts',(1.35257032843486,1.,-3.50408168106261));
#58703=CARTESIAN_POINT('Ctrl Pts',(1.35419113575956,1.,-3.50913227059999));
#58704=CARTESIAN_POINT('Ctrl Pts',(1.35611275237152,1.,-3.51542230699556));
#58705=CARTESIAN_POINT('Ctrl Pts',(1.35821701528836,1.,-3.52261776116748));
#58706=CARTESIAN_POINT('Ctrl Pts',(1.36037259643734,1.,-3.530344649616));
#58707=CARTESIAN_POINT('Ctrl Pts',(1.36245507339307,1.,-3.53824396424961));
#58708=CARTESIAN_POINT('Ctrl Pts',(1.36436666257597,1.,-3.54602591832973));
#58709=CARTESIAN_POINT('Ctrl Pts',(1.3660614545677,1.,-3.55353883995949));
#58710=CARTESIAN_POINT('Ctrl Pts',(1.36754771771233,1.,-3.56077662028649));
#58711=CARTESIAN_POINT('Ctrl Pts',(1.36886584973389,1.,-3.5678208030466));
#58712=CARTESIAN_POINT('Ctrl Pts',(1.37007229485659,1.,-3.57479875549486));
#58713=CARTESIAN_POINT('Ctrl Pts',(1.37122241663062,1.,-3.58183885982715));
#58714=CARTESIAN_POINT('Ctrl Pts',(1.37235053660976,1.,-3.58901853846365));
#58715=CARTESIAN_POINT('Ctrl Pts',(1.37346320103157,1.,-3.59634627869048));
#58716=CARTESIAN_POINT('Ctrl Pts',(1.37455051379623,1.,-3.60379020123988));
#58717=CARTESIAN_POINT('Ctrl Pts',(1.37559314436634,1.,-3.61129546591064));
#58718=CARTESIAN_POINT('Ctrl Pts',(1.37657053403107,1.,-3.61880481160421));
#58719=CARTESIAN_POINT('Ctrl Pts',(1.37746987919881,1.,-3.62628098665145));
#58720=CARTESIAN_POINT('Ctrl Pts',(1.37829035457339,1.,-3.63371727442486));
#58721=CARTESIAN_POINT('Ctrl Pts',(1.37903818567359,1.,-3.64112507791141));
#58722=CARTESIAN_POINT('Ctrl Pts',(1.37972372481603,1.,-3.64852652756456));
#58723=CARTESIAN_POINT('Ctrl Pts',(1.38035791051212,1.,-3.6559455440439));
#58724=CARTESIAN_POINT('Ctrl Pts',(1.38094856333552,1.,-3.66339848520857));
#58725=CARTESIAN_POINT('Ctrl Pts',(1.38149812653868,1.,-3.67088843112262));
#58726=CARTESIAN_POINT('Ctrl Pts',(1.3820057429062,1.,-3.67841038482414));
#58727=CARTESIAN_POINT('Ctrl Pts',(1.38246852827182,1.,-3.68595444983838));
#58728=CARTESIAN_POINT('Ctrl Pts',(1.3828831117165,1.,-3.69350967899526));
#58729=CARTESIAN_POINT('Ctrl Pts',(1.38324717612865,1.,-3.701067921679));
#58730=CARTESIAN_POINT('Ctrl Pts',(1.38356065402124,1.,-3.70862680753347));
#58731=CARTESIAN_POINT('Ctrl Pts',(1.38382489984586,1.,-3.7161876605181));
#58732=CARTESIAN_POINT('Ctrl Pts',(1.3840421342895,1.,-3.72375409358803));
#58733=CARTESIAN_POINT('Ctrl Pts',(1.38421479111531,1.,-3.73133035859282));
#58734=CARTESIAN_POINT('Ctrl Pts',(1.38434489156458,1.,-3.73891976418104));
#58735=CARTESIAN_POINT('Ctrl Pts',(1.38443344984394,1.,-3.74652317167876));
#58736=CARTESIAN_POINT('Ctrl Pts',(1.38448077997163,1.,-3.7541397631875));
#58737=CARTESIAN_POINT('Ctrl Pts',(1.3844867525335,1.,-3.76176768271367));
#58738=CARTESIAN_POINT('Ctrl Pts',(1.38445107339518,1.,-3.76940473185779));
#58739=CARTESIAN_POINT('Ctrl Pts',(1.38437354551428,1.,-3.77704902230418));
#58740=CARTESIAN_POINT('Ctrl Pts',(1.38425435883756,1.,-3.78469969805082));
#58741=CARTESIAN_POINT('Ctrl Pts',(1.38409399694566,1.,-3.79235669640841));
#58742=CARTESIAN_POINT('Ctrl Pts',(1.38389311766682,1.,-3.80002044322111));
#58743=CARTESIAN_POINT('Ctrl Pts',(1.3836524404622,1.,-3.80769156398411));
#58744=CARTESIAN_POINT('Ctrl Pts',(1.38337263902782,1.,-3.81537060817811));
#58745=CARTESIAN_POINT('Ctrl Pts',(1.38305421262763,1.,-3.82305771743829));
#58746=CARTESIAN_POINT('Ctrl Pts',(1.38269750245138,1.,-3.8307526698229));
#58747=CARTESIAN_POINT('Ctrl Pts',(1.38230274828821,1.,-3.83845502790746));
#58748=CARTESIAN_POINT('Ctrl Pts',(1.38187013346109,1.,-3.84616425605764));
#58749=CARTESIAN_POINT('Ctrl Pts',(1.38139983115049,1.,-3.85387983979481));
#58750=CARTESIAN_POINT('Ctrl Pts',(1.38089205992989,1.,-3.86160143043959));
#58751=CARTESIAN_POINT('Ctrl Pts',(1.38034709213014,1.,-3.86932885813068));
#58752=CARTESIAN_POINT('Ctrl Pts',(1.37976523097073,1.,-3.87706205830532));
#58753=CARTESIAN_POINT('Ctrl Pts',(1.37914679719383,1.,-3.88480102249278));
#58754=CARTESIAN_POINT('Ctrl Pts',(1.3784921128802,1.,-3.89254574338496));
#58755=CARTESIAN_POINT('Ctrl Pts',(1.37780148512792,1.,-3.90029615196727));
#58756=CARTESIAN_POINT('Ctrl Pts',(1.3770751963402,1.,-3.90805209523486));
#58757=CARTESIAN_POINT('Ctrl Pts',(1.37631350505797,1.,-3.91581337462644));
#58758=CARTESIAN_POINT('Ctrl Pts',(1.37551664448242,1.,-3.92357976987672));
#58759=CARTESIAN_POINT('Ctrl Pts',(1.37468482215751,1.,-3.93135106761844));
#58760=CARTESIAN_POINT('Ctrl Pts',(1.37381821967165,1.,-3.93912709040818));
#58761=CARTESIAN_POINT('Ctrl Pts',(1.37291699202807,1.,-3.94690771785133));
#58762=CARTESIAN_POINT('Ctrl Pts',(1.37198126432386,1.,-3.95469287280914));
#58763=CARTESIAN_POINT('Ctrl Pts',(1.3712051561502,1.,-3.96092458506535));
#58764=CARTESIAN_POINT('Ctrl Pts',(1.37060761745635,1.,-3.96560037974645));
#58765=CARTESIAN_POINT('Ctrl Pts',(1.37020239094614,1.,-3.9687184694131));
#58766=CARTESIAN_POINT('Ctrl Pts',(1.36999806084572,1.,-3.97027773754922));
#58767=CARTESIAN_POINT('Origin',(1.36999806084572,0.,-3.97027773754922));
#58768=CARTESIAN_POINT('',(1.22531898815164,1.,-4.01728681790024));
#58769=CARTESIAN_POINT('Origin',(0.,0.,0.));
#58770=CARTESIAN_POINT('',(1.51895082866166,1.,-3.42859860294378));
#58771=CARTESIAN_POINT('Origin',(0.,1.,0.));
#58772=CARTESIAN_POINT('Ctrl Pts',(1.51895082866166,1.,-3.42859860294378));
#58773=CARTESIAN_POINT('Ctrl Pts',(1.51895082866166,0.666666666666667,-3.42859860294378));
#58774=CARTESIAN_POINT('Ctrl Pts',(1.51895082866166,0.333333333333333,-3.42859860294378));
#58775=CARTESIAN_POINT('Ctrl Pts',(1.51895082866166,-0.333333333333333,
-3.42859860294378));
#58776=CARTESIAN_POINT('Ctrl Pts',(1.51895082866166,-0.666666666666667,
-3.42859860294378));
#58777=CARTESIAN_POINT('Ctrl Pts',(1.51895082866166,-1.,-3.42859860294378));
#58778=CARTESIAN_POINT('Ctrl Pts',(1.83867539237861,-1.,-3.77614523045147));
#58779=CARTESIAN_POINT('Ctrl Pts',(1.83867539237861,1.,-3.77614523045147));
#58780=CARTESIAN_POINT('Ctrl Pts',(1.83742834010821,-1.,-3.77518714458232));
#58781=CARTESIAN_POINT('Ctrl Pts',(1.83742834010821,1.,-3.77518714458232));
#58782=CARTESIAN_POINT('Ctrl Pts',(1.83493697935064,-1.,-3.77326886065484));
#58783=CARTESIAN_POINT('Ctrl Pts',(1.83493697935064,1.,-3.77326886065484));
#58784=CARTESIAN_POINT('Ctrl Pts',(1.83120816956515,-1.,-3.77038509819777));
#58785=CARTESIAN_POINT('Ctrl Pts',(1.83120816956515,1.,-3.77038509819777));
#58786=CARTESIAN_POINT('Ctrl Pts',(1.82625289221933,-1.,-3.76652740355856));
#58787=CARTESIAN_POINT('Ctrl Pts',(1.82625289221933,1.,-3.76652740355856));
#58788=CARTESIAN_POINT('Ctrl Pts',(1.82008629694924,-1.,-3.76168412709652));
#58789=CARTESIAN_POINT('Ctrl Pts',(1.82008629694924,1.,-3.76168412709652));
#58790=CARTESIAN_POINT('Ctrl Pts',(1.81394729834032,-1.,-3.75681965683995));
#58791=CARTESIAN_POINT('Ctrl Pts',(1.81394729834032,1.,-3.75681965683995));
#58792=CARTESIAN_POINT('Ctrl Pts',(1.80783603939662,-1.,-3.75193395888069));
#58793=CARTESIAN_POINT('Ctrl Pts',(1.80783603939662,1.,-3.75193395888069));
#58794=CARTESIAN_POINT('Ctrl Pts',(1.80175271485519,-1.,-3.74702700874954));
#58795=CARTESIAN_POINT('Ctrl Pts',(1.80175271485519,1.,-3.74702700874954));
#58796=CARTESIAN_POINT('Ctrl Pts',(1.79569757859041,-1.,-3.74209880351667));
#58797=CARTESIAN_POINT('Ctrl Pts',(1.79569757859041,1.,-3.74209880351667));
#58798=CARTESIAN_POINT('Ctrl Pts',(1.78967092823139,-1.,-3.73714934729962));
#58799=CARTESIAN_POINT('Ctrl Pts',(1.78967092823139,1.,-3.73714934729962));
#58800=CARTESIAN_POINT('Ctrl Pts',(1.78367308442682,-1.,-3.73217863095022));
#58801=CARTESIAN_POINT('Ctrl Pts',(1.78367308442682,1.,-3.73217863095022));
#58802=CARTESIAN_POINT('Ctrl Pts',(1.77770437039606,-1.,-3.72718661205504));
#58803=CARTESIAN_POINT('Ctrl Pts',(1.77770437039606,1.,-3.72718661205504));
#58804=CARTESIAN_POINT('Ctrl Pts',(1.77176509401846,-1.,-3.72217319911429));
#58805=CARTESIAN_POINT('Ctrl Pts',(1.77176509401846,1.,-3.72217319911429));
#58806=CARTESIAN_POINT('Ctrl Pts',(1.76585552124549,-1.,-3.71713822377676));
#58807=CARTESIAN_POINT('Ctrl Pts',(1.76585552124549,1.,-3.71713822377676));
#58808=CARTESIAN_POINT('Ctrl Pts',(1.75997588499021,-1.,-3.71208146346455));
#58809=CARTESIAN_POINT('Ctrl Pts',(1.75997588499021,1.,-3.71208146346455));
#58810=CARTESIAN_POINT('Ctrl Pts',(1.75412641804148,-1.,-3.70700269736876));
#58811=CARTESIAN_POINT('Ctrl Pts',(1.75412641804148,1.,-3.70700269736876));
#58812=CARTESIAN_POINT('Ctrl Pts',(1.74830738046092,-1.,-3.70190175673422));
#58813=CARTESIAN_POINT('Ctrl Pts',(1.74830738046092,1.,-3.70190175673422));
#58814=CARTESIAN_POINT('Ctrl Pts',(1.74251908492589,-1.,-3.6967785691046));
#58815=CARTESIAN_POINT('Ctrl Pts',(1.74251908492589,1.,-3.6967785691046));
#58816=CARTESIAN_POINT('Ctrl Pts',(1.73676193254493,-1.,-3.69163322647906));
#58817=CARTESIAN_POINT('Ctrl Pts',(1.73676193254493,1.,-3.69163322647906));
#58818=CARTESIAN_POINT('Ctrl Pts',(1.73103640956647,-1.,-3.68646597019188));
#58819=CARTESIAN_POINT('Ctrl Pts',(1.73103640956647,1.,-3.68646597019188));
#58820=CARTESIAN_POINT('Ctrl Pts',(1.72534302437003,-1.,-3.68127704936472));
#58821=CARTESIAN_POINT('Ctrl Pts',(1.72534302437003,1.,-3.68127704936472));
#58822=CARTESIAN_POINT('Ctrl Pts',(1.71968225581787,-1.,-3.67606660374665));
#58823=CARTESIAN_POINT('Ctrl Pts',(1.71968225581787,1.,-3.67606660374665));
#58824=CARTESIAN_POINT('Ctrl Pts',(1.71405450210392,-1.,-3.67083454901629));
#58825=CARTESIAN_POINT('Ctrl Pts',(1.71405450210392,1.,-3.67083454901629));
#58826=CARTESIAN_POINT('Ctrl Pts',(1.70846001610983,-1.,-3.6655804319893));
#58827=CARTESIAN_POINT('Ctrl Pts',(1.70846001610983,1.,-3.6655804319893));
#58828=CARTESIAN_POINT('Ctrl Pts',(1.70289888566904,-1.,-3.6603033877491));
#58829=CARTESIAN_POINT('Ctrl Pts',(1.70289888566904,1.,-3.6603033877491));
#58830=CARTESIAN_POINT('Ctrl Pts',(1.69737117722558,-1.,-3.65500246526798));
#58831=CARTESIAN_POINT('Ctrl Pts',(1.69737117722558,1.,-3.65500246526798));
#58832=CARTESIAN_POINT('Ctrl Pts',(1.691877054817,-1.,-3.64967689827393));
#58833=CARTESIAN_POINT('Ctrl Pts',(1.691877054817,1.,-3.64967689827393));
#58834=CARTESIAN_POINT('Ctrl Pts',(1.68641690471455,-1.,-3.64432638915199));
#58835=CARTESIAN_POINT('Ctrl Pts',(1.68641690471455,1.,-3.64432638915199));
#58836=CARTESIAN_POINT('Ctrl Pts',(1.68099146651577,-1.,-3.63895140887443));
#58837=CARTESIAN_POINT('Ctrl Pts',(1.68099146651577,1.,-3.63895140887443));
#58838=CARTESIAN_POINT('Ctrl Pts',(1.67560193613145,-1.,-3.63355343201211));
#58839=CARTESIAN_POINT('Ctrl Pts',(1.67560193613145,1.,-3.63355343201211));
#58840=CARTESIAN_POINT('Ctrl Pts',(1.67024966008037,-1.,-3.62813422105257));
#58841=CARTESIAN_POINT('Ctrl Pts',(1.67024966008037,1.,-3.62813422105257));
#58842=CARTESIAN_POINT('Ctrl Pts',(1.66493585923853,-1.,-3.62269517989104));
#58843=CARTESIAN_POINT('Ctrl Pts',(1.66493585923853,1.,-3.62269517989104));
#58844=CARTESIAN_POINT('Ctrl Pts',(1.65966133399186,-1.,-3.61723666482457));
#58845=CARTESIAN_POINT('Ctrl Pts',(1.65966133399186,1.,-3.61723666482457));
#58846=CARTESIAN_POINT('Ctrl Pts',(1.65442619244327,-1.,-3.61175734965129));
#58847=CARTESIAN_POINT('Ctrl Pts',(1.65442619244327,1.,-3.61175734965129));
#58848=CARTESIAN_POINT('Ctrl Pts',(1.64922952425833,-1.,-3.60625346556992));
#58849=CARTESIAN_POINT('Ctrl Pts',(1.64922952425833,1.,-3.60625346556992));
#58850=CARTESIAN_POINT('Ctrl Pts',(1.6440700438558,-1.,-3.6007202851384));
#58851=CARTESIAN_POINT('Ctrl Pts',(1.6440700438558,1.,-3.6007202851384));
#58852=CARTESIAN_POINT('Ctrl Pts',(1.63894676675349,-1.,-3.59515368334887));
#58853=CARTESIAN_POINT('Ctrl Pts',(1.63894676675349,1.,-3.59515368334887));
#58854=CARTESIAN_POINT('Ctrl Pts',(1.63385971451259,-1.,-3.58955176627876));
#58855=CARTESIAN_POINT('Ctrl Pts',(1.63385971451259,1.,-3.58955176627876));
#58856=CARTESIAN_POINT('Ctrl Pts',(1.62881051550748,-1.,-3.5839162577435));
#58857=CARTESIAN_POINT('Ctrl Pts',(1.62881051550748,1.,-3.5839162577435));
#58858=CARTESIAN_POINT('Ctrl Pts',(1.62380329464851,-1.,-3.57825455954405));
#58859=CARTESIAN_POINT('Ctrl Pts',(1.62380329464851,1.,-3.57825455954405));
#58860=CARTESIAN_POINT('Ctrl Pts',(1.61884340915412,-1.,-3.57257679609826));
#58861=CARTESIAN_POINT('Ctrl Pts',(1.61884340915412,1.,-3.57257679609826));
#58862=CARTESIAN_POINT('Ctrl Pts',(1.61393581747522,-1.,-3.56689200468404));
#58863=CARTESIAN_POINT('Ctrl Pts',(1.61393581747522,1.,-3.56689200468404));
#58864=CARTESIAN_POINT('Ctrl Pts',(1.60908344685459,-1.,-3.56120432482986));
#58865=CARTESIAN_POINT('Ctrl Pts',(1.60908344685459,1.,-3.56120432482986));
#58866=CARTESIAN_POINT('Ctrl Pts',(1.60428584699848,-1.,-3.55550985096117));
#58867=CARTESIAN_POINT('Ctrl Pts',(1.60428584699848,1.,-3.55550985096117));
#58868=CARTESIAN_POINT('Ctrl Pts',(1.59953698113444,-1.,-3.54979148634426));
#58869=CARTESIAN_POINT('Ctrl Pts',(1.59953698113444,1.,-3.54979148634426));
#58870=CARTESIAN_POINT('Ctrl Pts',(1.5948276694975,-1.,-3.544024581823));
#58871=CARTESIAN_POINT('Ctrl Pts',(1.5948276694975,1.,-3.544024581823));
#58872=CARTESIAN_POINT('Ctrl Pts',(1.59014958368725,-1.,-3.53818616861045));
#58873=CARTESIAN_POINT('Ctrl Pts',(1.59014958368725,1.,-3.53818616861045));
#58874=CARTESIAN_POINT('Ctrl Pts',(1.58549906268083,-1.,-3.53226378147068));
#58875=CARTESIAN_POINT('Ctrl Pts',(1.58549906268083,1.,-3.53226378147068));
#58876=CARTESIAN_POINT('Ctrl Pts',(1.58088027227856,-1.,-3.52626275334899));
#58877=CARTESIAN_POINT('Ctrl Pts',(1.58088027227856,1.,-3.52626275334899));
#58878=CARTESIAN_POINT('Ctrl Pts',(1.5763104998818,-1.,-3.52021847865961));
#58879=CARTESIAN_POINT('Ctrl Pts',(1.5763104998818,1.,-3.52021847865961));
#58880=CARTESIAN_POINT('Ctrl Pts',(1.57181569799774,-1.,-3.51418598431733));
#58881=CARTESIAN_POINT('Ctrl Pts',(1.57181569799774,1.,-3.51418598431733));
#58882=CARTESIAN_POINT('Ctrl Pts',(1.56742097575041,-1.,-3.50821771695427));
#58883=CARTESIAN_POINT('Ctrl Pts',(1.56742097575041,1.,-3.50821771695427));
#58884=CARTESIAN_POINT('Ctrl Pts',(1.56314187758689,-1.,-3.50234321621607));
#58885=CARTESIAN_POINT('Ctrl Pts',(1.56314187758689,1.,-3.50234321621607));
#58886=CARTESIAN_POINT('Ctrl Pts',(1.55897703097859,-1.,-3.49655185179623));
#58887=CARTESIAN_POINT('Ctrl Pts',(1.55897703097859,1.,-3.49655185179623));
#58888=CARTESIAN_POINT('Ctrl Pts',(1.5548959590107,-1.,-3.49076460877317));
#58889=CARTESIAN_POINT('Ctrl Pts',(1.5548959590107,1.,-3.49076460877317));
#58890=CARTESIAN_POINT('Ctrl Pts',(1.55084702970382,-1.,-3.48485155928414));
#58891=CARTESIAN_POINT('Ctrl Pts',(1.55084702970382,1.,-3.48485155928414));
#58892=CARTESIAN_POINT('Ctrl Pts',(1.54678009290206,-1.,-3.47868272898599));
#58893=CARTESIAN_POINT('Ctrl Pts',(1.54678009290206,1.,-3.47868272898599));
#58894=CARTESIAN_POINT('Ctrl Pts',(1.54266605398152,-1.,-3.47217189224576));
#58895=CARTESIAN_POINT('Ctrl Pts',(1.54266605398152,1.,-3.47217189224576));
#58896=CARTESIAN_POINT('Ctrl Pts',(1.53851507915533,-1.,-3.46531752207222));
#58897=CARTESIAN_POINT('Ctrl Pts',(1.53851507915533,1.,-3.46531752207222));
#58898=CARTESIAN_POINT('Ctrl Pts',(1.53440195378902,-1.,-3.45825932955273));
#58899=CARTESIAN_POINT('Ctrl Pts',(1.53440195378902,1.,-3.45825932955273));
#58900=CARTESIAN_POINT('Ctrl Pts',(1.530462444618,-1.,-3.45127136828667));
#58901=CARTESIAN_POINT('Ctrl Pts',(1.530462444618,1.,-3.45127136828667));
#58902=CARTESIAN_POINT('Ctrl Pts',(1.52686242875717,-1.,-3.44469547527));
#58903=CARTESIAN_POINT('Ctrl Pts',(1.52686242875717,1.,-3.44469547527));
#58904=CARTESIAN_POINT('Ctrl Pts',(1.52377348950429,-1.,-3.43888895974182));
#58905=CARTESIAN_POINT('Ctrl Pts',(1.52377348950429,1.,-3.43888895974182));
#58906=CARTESIAN_POINT('Ctrl Pts',(1.52134826724227,-1.,-3.43417156977749));
#58907=CARTESIAN_POINT('Ctrl Pts',(1.52134826724227,1.,-3.43417156977749));
#58908=CARTESIAN_POINT('Ctrl Pts',(1.51969006980792,-1.,-3.43076036253384));
#58909=CARTESIAN_POINT('Ctrl Pts',(1.51969006980792,1.,-3.43076036253384));
#58910=CARTESIAN_POINT('Ctrl Pts',(1.51901585838879,-1.,-3.42915787669388));
#58911=CARTESIAN_POINT('Ctrl Pts',(1.51901585838879,1.,-3.42915787669388));
#58912=CARTESIAN_POINT('Ctrl Pts',(1.51888450659497,-1.,-3.42860527148835));
#58913=CARTESIAN_POINT('Ctrl Pts',(1.51888450659497,1.,-3.42860527148835));
#58914=CARTESIAN_POINT('Ctrl Pts',(1.51896318668306,-1.,-3.42852521763648));
#58915=CARTESIAN_POINT('Ctrl Pts',(1.51896318668306,1.,-3.42852521763648));
#58916=CARTESIAN_POINT('Ctrl Pts',(1.519044091397,-1.,-3.42855728381368));
#58917=CARTESIAN_POINT('Ctrl Pts',(1.519044091397,1.,-3.42855728381368));
#58918=CARTESIAN_POINT('',(1.83867539237861,1.,-3.77614523045147));
#58919=CARTESIAN_POINT('Ctrl Pts',(1.83867539237861,1.,-3.77614523045147));
#58920=CARTESIAN_POINT('Ctrl Pts',(1.83742834010821,1.,-3.77518714458232));
#58921=CARTESIAN_POINT('Ctrl Pts',(1.83493697935064,1.,-3.77326886065484));
#58922=CARTESIAN_POINT('Ctrl Pts',(1.83120816956515,1.,-3.77038509819777));
#58923=CARTESIAN_POINT('Ctrl Pts',(1.82625289221933,1.,-3.76652740355856));
#58924=CARTESIAN_POINT('Ctrl Pts',(1.82008629694924,1.,-3.76168412709652));
#58925=CARTESIAN_POINT('Ctrl Pts',(1.81394729834032,1.,-3.75681965683995));
#58926=CARTESIAN_POINT('Ctrl Pts',(1.80783603939662,1.,-3.75193395888069));
#58927=CARTESIAN_POINT('Ctrl Pts',(1.80175271485519,1.,-3.74702700874954));
#58928=CARTESIAN_POINT('Ctrl Pts',(1.79569757859041,1.,-3.74209880351667));
#58929=CARTESIAN_POINT('Ctrl Pts',(1.78967092823139,1.,-3.73714934729962));
#58930=CARTESIAN_POINT('Ctrl Pts',(1.78367308442682,1.,-3.73217863095022));
#58931=CARTESIAN_POINT('Ctrl Pts',(1.77770437039606,1.,-3.72718661205504));
#58932=CARTESIAN_POINT('Ctrl Pts',(1.77176509401846,1.,-3.72217319911429));
#58933=CARTESIAN_POINT('Ctrl Pts',(1.76585552124549,1.,-3.71713822377676));
#58934=CARTESIAN_POINT('Ctrl Pts',(1.75997588499021,1.,-3.71208146346455));
#58935=CARTESIAN_POINT('Ctrl Pts',(1.75412641804148,1.,-3.70700269736876));
#58936=CARTESIAN_POINT('Ctrl Pts',(1.74830738046092,1.,-3.70190175673422));
#58937=CARTESIAN_POINT('Ctrl Pts',(1.74251908492589,1.,-3.6967785691046));
#58938=CARTESIAN_POINT('Ctrl Pts',(1.73676193254493,1.,-3.69163322647906));
#58939=CARTESIAN_POINT('Ctrl Pts',(1.73103640956647,1.,-3.68646597019188));
#58940=CARTESIAN_POINT('Ctrl Pts',(1.72534302437003,1.,-3.68127704936472));
#58941=CARTESIAN_POINT('Ctrl Pts',(1.71968225581787,1.,-3.67606660374665));
#58942=CARTESIAN_POINT('Ctrl Pts',(1.71405450210392,1.,-3.67083454901629));
#58943=CARTESIAN_POINT('Ctrl Pts',(1.70846001610983,1.,-3.6655804319893));
#58944=CARTESIAN_POINT('Ctrl Pts',(1.70289888566904,1.,-3.6603033877491));
#58945=CARTESIAN_POINT('Ctrl Pts',(1.69737117722558,1.,-3.65500246526798));
#58946=CARTESIAN_POINT('Ctrl Pts',(1.691877054817,1.,-3.64967689827393));
#58947=CARTESIAN_POINT('Ctrl Pts',(1.68641690471455,1.,-3.64432638915199));
#58948=CARTESIAN_POINT('Ctrl Pts',(1.68099146651577,1.,-3.63895140887443));
#58949=CARTESIAN_POINT('Ctrl Pts',(1.67560193613145,1.,-3.63355343201211));
#58950=CARTESIAN_POINT('Ctrl Pts',(1.67024966008037,1.,-3.62813422105257));
#58951=CARTESIAN_POINT('Ctrl Pts',(1.66493585923853,1.,-3.62269517989104));
#58952=CARTESIAN_POINT('Ctrl Pts',(1.65966133399186,1.,-3.61723666482457));
#58953=CARTESIAN_POINT('Ctrl Pts',(1.65442619244327,1.,-3.61175734965129));
#58954=CARTESIAN_POINT('Ctrl Pts',(1.64922952425833,1.,-3.60625346556992));
#58955=CARTESIAN_POINT('Ctrl Pts',(1.6440700438558,1.,-3.6007202851384));
#58956=CARTESIAN_POINT('Ctrl Pts',(1.63894676675349,1.,-3.59515368334887));
#58957=CARTESIAN_POINT('Ctrl Pts',(1.63385971451259,1.,-3.58955176627876));
#58958=CARTESIAN_POINT('Ctrl Pts',(1.62881051550748,1.,-3.5839162577435));
#58959=CARTESIAN_POINT('Ctrl Pts',(1.62380329464851,1.,-3.57825455954405));
#58960=CARTESIAN_POINT('Ctrl Pts',(1.61884340915412,1.,-3.57257679609826));
#58961=CARTESIAN_POINT('Ctrl Pts',(1.61393581747522,1.,-3.56689200468404));
#58962=CARTESIAN_POINT('Ctrl Pts',(1.60908344685459,1.,-3.56120432482986));
#58963=CARTESIAN_POINT('Ctrl Pts',(1.60428584699848,1.,-3.55550985096117));
#58964=CARTESIAN_POINT('Ctrl Pts',(1.59953698113444,1.,-3.54979148634426));
#58965=CARTESIAN_POINT('Ctrl Pts',(1.5948276694975,1.,-3.544024581823));
#58966=CARTESIAN_POINT('Ctrl Pts',(1.59014958368725,1.,-3.53818616861045));
#58967=CARTESIAN_POINT('Ctrl Pts',(1.58549906268083,1.,-3.53226378147068));
#58968=CARTESIAN_POINT('Ctrl Pts',(1.58088027227856,1.,-3.52626275334899));
#58969=CARTESIAN_POINT('Ctrl Pts',(1.5763104998818,1.,-3.52021847865961));
#58970=CARTESIAN_POINT('Ctrl Pts',(1.57181569799774,1.,-3.51418598431733));
#58971=CARTESIAN_POINT('Ctrl Pts',(1.56742097575041,1.,-3.50821771695427));
#58972=CARTESIAN_POINT('Ctrl Pts',(1.56314187758689,1.,-3.50234321621607));
#58973=CARTESIAN_POINT('Ctrl Pts',(1.55897703097859,1.,-3.49655185179623));
#58974=CARTESIAN_POINT('Ctrl Pts',(1.5548959590107,1.,-3.49076460877317));
#58975=CARTESIAN_POINT('Ctrl Pts',(1.55084702970382,1.,-3.48485155928414));
#58976=CARTESIAN_POINT('Ctrl Pts',(1.54678009290206,1.,-3.47868272898599));
#58977=CARTESIAN_POINT('Ctrl Pts',(1.54266605398152,1.,-3.47217189224576));
#58978=CARTESIAN_POINT('Ctrl Pts',(1.53851507915533,1.,-3.46531752207222));
#58979=CARTESIAN_POINT('Ctrl Pts',(1.53440195378902,1.,-3.45825932955273));
#58980=CARTESIAN_POINT('Ctrl Pts',(1.530462444618,1.,-3.45127136828667));
#58981=CARTESIAN_POINT('Ctrl Pts',(1.52686242875717,1.,-3.44469547527));
#58982=CARTESIAN_POINT('Ctrl Pts',(1.52377348950429,1.,-3.43888895974182));
#58983=CARTESIAN_POINT('Ctrl Pts',(1.52134826724227,1.,-3.43417156977749));
#58984=CARTESIAN_POINT('Ctrl Pts',(1.5198144909343,1.,-3.43101631893491));
#58985=CARTESIAN_POINT('Ctrl Pts',(1.51914806898539,1.,-3.42946838852728));
#58986=CARTESIAN_POINT('Ctrl Pts',(1.51895133295017,1.,-3.42884302333978));
#58987=CARTESIAN_POINT('Ctrl Pts',(1.51893924967231,1.,-3.42864616361967));
#58988=CARTESIAN_POINT('Ctrl Pts',(1.51895082866166,1.,-3.42859860294378));
#58989=CARTESIAN_POINT('',(1.83867539237861,0.,-3.77614523045147));
#58990=CARTESIAN_POINT('Ctrl Pts',(1.8808893942881,-1.,-3.24418789321065));
#58991=CARTESIAN_POINT('Ctrl Pts',(1.8808893942881,1.,-3.24418789321065));
#58992=CARTESIAN_POINT('Ctrl Pts',(1.8809110068042,-1.,-3.24410359189733));
#58993=CARTESIAN_POINT('Ctrl Pts',(1.8809110068042,1.,-3.24410359189733));
#58994=CARTESIAN_POINT('Ctrl Pts',(1.8810220187274,-1.,-3.24408699284449));
#58995=CARTESIAN_POINT('Ctrl Pts',(1.8810220187274,1.,-3.24408699284449));
#58996=CARTESIAN_POINT('Ctrl Pts',(1.88139187908347,-1.,-3.24451807186964));
#58997=CARTESIAN_POINT('Ctrl Pts',(1.88139187908347,1.,-3.24451807186964));
#58998=CARTESIAN_POINT('Ctrl Pts',(1.88229202583187,-1.,-3.24600543790876));
#58999=CARTESIAN_POINT('Ctrl Pts',(1.88229202583187,1.,-3.24600543790876));
#59000=CARTESIAN_POINT('Ctrl Pts',(1.88407708646435,-1.,-3.24935200512055));
#59001=CARTESIAN_POINT('Ctrl Pts',(1.88407708646435,1.,-3.24935200512055));
#59002=CARTESIAN_POINT('Ctrl Pts',(1.88646802523372,-1.,-3.25408686339298));
#59003=CARTESIAN_POINT('Ctrl Pts',(1.88646802523372,1.,-3.25408686339298));
#59004=CARTESIAN_POINT('Ctrl Pts',(1.88934996203508,-1.,-3.2599988519361));
#59005=CARTESIAN_POINT('Ctrl Pts',(1.88934996203508,1.,-3.2599988519361));
#59006=CARTESIAN_POINT('Ctrl Pts',(1.89255393500769,-1.,-3.2667765388833));
#59007=CARTESIAN_POINT('Ctrl Pts',(1.89255393500769,1.,-3.2667765388833));
#59008=CARTESIAN_POINT('Ctrl Pts',(1.89589172903662,-1.,-3.27407108932908));
#59009=CARTESIAN_POINT('Ctrl Pts',(1.89589172903662,1.,-3.27407108932908));
#59010=CARTESIAN_POINT('Ctrl Pts',(1.89918429230424,-1.,-3.28154737912287));
#59011=CARTESIAN_POINT('Ctrl Pts',(1.89918429230424,1.,-3.28154737912287));
#59012=CARTESIAN_POINT('Ctrl Pts',(1.9022897124757,-1.,-3.28893448600364));
#59013=CARTESIAN_POINT('Ctrl Pts',(1.9022897124757,1.,-3.28893448600364));
#59014=CARTESIAN_POINT('Ctrl Pts',(1.9051389186417,-1.,-3.29608978722258));
#59015=CARTESIAN_POINT('Ctrl Pts',(1.9051389186417,1.,-3.29608978722258));
#59016=CARTESIAN_POINT('Ctrl Pts',(1.90773912171424,-1.,-3.30300595568341));
#59017=CARTESIAN_POINT('Ctrl Pts',(1.90773912171424,1.,-3.30300595568341));
#59018=CARTESIAN_POINT('Ctrl Pts',(1.91014297830502,-1.,-3.30975721158694));
#59019=CARTESIAN_POINT('Ctrl Pts',(1.91014297830502,1.,-3.30975721158694));
#59020=CARTESIAN_POINT('Ctrl Pts',(1.91242616234459,-1.,-3.31646052426395));
#59021=CARTESIAN_POINT('Ctrl Pts',(1.91242616234459,1.,-3.31646052426395));
#59022=CARTESIAN_POINT('Ctrl Pts',(1.91466343916612,-1.,-3.32323403454507));
#59023=CARTESIAN_POINT('Ctrl Pts',(1.91466343916612,1.,-3.32323403454507));
#59024=CARTESIAN_POINT('Ctrl Pts',(1.91690081930297,-1.,-3.33014884257812));
#59025=CARTESIAN_POINT('Ctrl Pts',(1.91690081930297,1.,-3.33014884257812));
#59026=CARTESIAN_POINT('Ctrl Pts',(1.91914609610173,-1.,-3.33721230709948));
#59027=CARTESIAN_POINT('Ctrl Pts',(1.91914609610173,1.,-3.33721230709948));
#59028=CARTESIAN_POINT('Ctrl Pts',(1.92138450828378,-1.,-3.34439448941915));
#59029=CARTESIAN_POINT('Ctrl Pts',(1.92138450828378,1.,-3.34439448941915));
#59030=CARTESIAN_POINT('Ctrl Pts',(1.92358838440518,-1.,-3.35164424847207));
#59031=CARTESIAN_POINT('Ctrl Pts',(1.92358838440518,1.,-3.35164424847207));
#59032=CARTESIAN_POINT('Ctrl Pts',(1.92572846125763,-1.,-3.35890824422976));
#59033=CARTESIAN_POINT('Ctrl Pts',(1.92572846125763,1.,-3.35890824422976));
#59034=CARTESIAN_POINT('Ctrl Pts',(1.92778626543803,-1.,-3.36615168657597));
#59035=CARTESIAN_POINT('Ctrl Pts',(1.92778626543803,1.,-3.36615168657597));
#59036=CARTESIAN_POINT('Ctrl Pts',(1.92975993109897,-1.,-3.37336807068078));
#59037=CARTESIAN_POINT('Ctrl Pts',(1.92975993109897,1.,-3.37336807068078));
#59038=CARTESIAN_POINT('Ctrl Pts',(1.93165739093292,-1.,-3.38056768525577));
#59039=CARTESIAN_POINT('Ctrl Pts',(1.93165739093292,1.,-3.38056768525577));
#59040=CARTESIAN_POINT('Ctrl Pts',(1.93349233176794,-1.,-3.38777076883267));
#59041=CARTESIAN_POINT('Ctrl Pts',(1.93349233176794,1.,-3.38777076883267));
#59042=CARTESIAN_POINT('Ctrl Pts',(1.93527929945982,-1.,-3.39499923640789));
#59043=CARTESIAN_POINT('Ctrl Pts',(1.93527929945982,1.,-3.39499923640789));
#59044=CARTESIAN_POINT('Ctrl Pts',(1.93702857723089,-1.,-3.40226802104093));
#59045=CARTESIAN_POINT('Ctrl Pts',(1.93702857723089,1.,-3.40226802104093));
#59046=CARTESIAN_POINT('Ctrl Pts',(1.93874306008132,-1.,-3.40957978266623));
#59047=CARTESIAN_POINT('Ctrl Pts',(1.93874306008132,1.,-3.40957978266623));
#59048=CARTESIAN_POINT('Ctrl Pts',(1.94042111965237,-1.,-3.41692971994082));
#59049=CARTESIAN_POINT('Ctrl Pts',(1.94042111965237,1.,-3.41692971994082));
#59050=CARTESIAN_POINT('Ctrl Pts',(1.94205835913692,-1.,-3.42430850941497));
#59051=CARTESIAN_POINT('Ctrl Pts',(1.94205835913692,1.,-3.42430850941497));
#59052=CARTESIAN_POINT('Ctrl Pts',(1.94364973660285,-1.,-3.43170586602436));
#59053=CARTESIAN_POINT('Ctrl Pts',(1.94364973660285,1.,-3.43170586602436));
#59054=CARTESIAN_POINT('Ctrl Pts',(1.94519168842883,-1.,-3.43911410197693));
#59055=CARTESIAN_POINT('Ctrl Pts',(1.94519168842883,1.,-3.43911410197693));
#59056=CARTESIAN_POINT('Ctrl Pts',(1.94668377715332,-1.,-3.44653088665685));
#59057=CARTESIAN_POINT('Ctrl Pts',(1.94668377715332,1.,-3.44653088665685));
#59058=CARTESIAN_POINT('Ctrl Pts',(1.94812754766524,-1.,-3.45395731584051));
#59059=CARTESIAN_POINT('Ctrl Pts',(1.94812754766524,1.,-3.45395731584051));
#59060=CARTESIAN_POINT('Ctrl Pts',(1.94952575850196,-1.,-3.46139661060959));
#59061=CARTESIAN_POINT('Ctrl Pts',(1.94952575850196,1.,-3.46139661060959));
#59062=CARTESIAN_POINT('Ctrl Pts',(1.95088147859876,-1.,-3.4688525897419));
#59063=CARTESIAN_POINT('Ctrl Pts',(1.95088147859876,1.,-3.4688525897419));
#59064=CARTESIAN_POINT('Ctrl Pts',(1.95219722189878,-1.,-3.47632820495926));
#59065=CARTESIAN_POINT('Ctrl Pts',(1.95219722189878,1.,-3.47632820495926));
#59066=CARTESIAN_POINT('Ctrl Pts',(1.95347412486316,-1.,-3.48382414832649));
#59067=CARTESIAN_POINT('Ctrl Pts',(1.95347412486316,1.,-3.48382414832649));
#59068=CARTESIAN_POINT('Ctrl Pts',(1.95471236969653,-1.,-3.49133956289154));
#59069=CARTESIAN_POINT('Ctrl Pts',(1.95471236969653,1.,-3.49133956289154));
#59070=CARTESIAN_POINT('Ctrl Pts',(1.9559115382367,-1.,-3.49887263575602));
#59071=CARTESIAN_POINT('Ctrl Pts',(1.9559115382367,1.,-3.49887263575602));
#59072=CARTESIAN_POINT('Ctrl Pts',(1.95707099606513,-1.,-3.50642124159913));
#59073=CARTESIAN_POINT('Ctrl Pts',(1.95707099606513,1.,-3.50642124159913));
#59074=CARTESIAN_POINT('Ctrl Pts',(1.95819025316768,-1.,-3.51398354617773));
#59075=CARTESIAN_POINT('Ctrl Pts',(1.95819025316768,1.,-3.51398354617773));
#59076=CARTESIAN_POINT('Ctrl Pts',(1.95926936324436,-1.,-3.52155867431438));
#59077=CARTESIAN_POINT('Ctrl Pts',(1.95926936324436,1.,-3.52155867431438));
#59078=CARTESIAN_POINT('Ctrl Pts',(1.96030879411534,-1.,-3.52914648844289));
#59079=CARTESIAN_POINT('Ctrl Pts',(1.96030879411534,1.,-3.52914648844289));
#59080=CARTESIAN_POINT('Ctrl Pts',(1.96130926212661,-1.,-3.53674730625759));
#59081=CARTESIAN_POINT('Ctrl Pts',(1.96130926212661,1.,-3.53674730625759));
#59082=CARTESIAN_POINT('Ctrl Pts',(1.96227157573058,-1.,-3.54436163300425));
#59083=CARTESIAN_POINT('Ctrl Pts',(1.96227157573058,1.,-3.54436163300425));
#59084=CARTESIAN_POINT('Ctrl Pts',(1.96319648628667,-1.,-3.55198990600929));
#59085=CARTESIAN_POINT('Ctrl Pts',(1.96319648628667,1.,-3.55198990600929));
#59086=CARTESIAN_POINT('Ctrl Pts',(1.96408450906868,-1.,-3.55963218706201));
#59087=CARTESIAN_POINT('Ctrl Pts',(1.96408450906868,1.,-3.55963218706201));
#59088=CARTESIAN_POINT('Ctrl Pts',(1.96493594634643,-1.,-3.56728820357933));
#59089=CARTESIAN_POINT('Ctrl Pts',(1.96493594634643,1.,-3.56728820357933));
#59090=CARTESIAN_POINT('Ctrl Pts',(1.96575096652857,-1.,-3.57495748601088));
#59091=CARTESIAN_POINT('Ctrl Pts',(1.96575096652857,1.,-3.57495748601088));
#59092=CARTESIAN_POINT('Ctrl Pts',(1.9665296668894,-1.,-3.58263947663884));
#59093=CARTESIAN_POINT('Ctrl Pts',(1.9665296668894,1.,-3.58263947663884));
#59094=CARTESIAN_POINT('Ctrl Pts',(1.96727213799507,-1.,-3.5903336402273));
#59095=CARTESIAN_POINT('Ctrl Pts',(1.96727213799507,1.,-3.5903336402273));
#59096=CARTESIAN_POINT('Ctrl Pts',(1.96797854118257,-1.,-3.59803959819725));
#59097=CARTESIAN_POINT('Ctrl Pts',(1.96797854118257,1.,-3.59803959819725));
#59098=CARTESIAN_POINT('Ctrl Pts',(1.96864911885775,-1.,-3.60575714017676));
#59099=CARTESIAN_POINT('Ctrl Pts',(1.96864911885775,1.,-3.60575714017676));
#59100=CARTESIAN_POINT('Ctrl Pts',(1.96928416040712,-1.,-3.61348615496393));
#59101=CARTESIAN_POINT('Ctrl Pts',(1.96928416040712,1.,-3.61348615496393));
#59102=CARTESIAN_POINT('Ctrl Pts',(1.96988398129888,-1.,-3.62122658401722));
#59103=CARTESIAN_POINT('Ctrl Pts',(1.96988398129888,1.,-3.62122658401722));
#59104=CARTESIAN_POINT('Ctrl Pts',(1.97044889850518,-1.,-3.62897836973397));
#59105=CARTESIAN_POINT('Ctrl Pts',(1.97044889850518,1.,-3.62897836973397));
#59106=CARTESIAN_POINT('Ctrl Pts',(1.97097920454698,-1.,-3.63674139590853));
#59107=CARTESIAN_POINT('Ctrl Pts',(1.97097920454698,1.,-3.63674139590853));
#59108=CARTESIAN_POINT('Ctrl Pts',(1.97147515441539,-1.,-3.64451546724222));
#59109=CARTESIAN_POINT('Ctrl Pts',(1.97147515441539,1.,-3.64451546724222));
#59110=CARTESIAN_POINT('Ctrl Pts',(1.97193697240645,-1.,-3.65230034717364));
#59111=CARTESIAN_POINT('Ctrl Pts',(1.97193697240645,1.,-3.65230034717364));
#59112=CARTESIAN_POINT('Ctrl Pts',(1.97236485439317,-1.,-3.66009578166865));
#59113=CARTESIAN_POINT('Ctrl Pts',(1.97236485439317,1.,-3.66009578166865));
#59114=CARTESIAN_POINT('Ctrl Pts',(1.9727589719863,-1.,-3.66790152751984));
#59115=CARTESIAN_POINT('Ctrl Pts',(1.9727589719863,1.,-3.66790152751984));
#59116=CARTESIAN_POINT('Ctrl Pts',(1.97311947678035,-1.,-3.67571738106175));
#59117=CARTESIAN_POINT('Ctrl Pts',(1.97311947678035,1.,-3.67571738106175));
#59118=CARTESIAN_POINT('Ctrl Pts',(1.9734465030363,-1.,-3.68354319913416));
#59119=CARTESIAN_POINT('Ctrl Pts',(1.9734465030363,1.,-3.68354319913416));
#59120=CARTESIAN_POINT('Ctrl Pts',(1.97374016224397,-1.,-3.69137888597855));
#59121=CARTESIAN_POINT('Ctrl Pts',(1.97374016224397,1.,-3.69137888597855));
#59122=CARTESIAN_POINT('Ctrl Pts',(1.97394846382288,-1.,-3.69765528558292));
#59123=CARTESIAN_POINT('Ctrl Pts',(1.97394846382288,1.,-3.69765528558292));
#59124=CARTESIAN_POINT('Ctrl Pts',(1.97408973726149,-1.,-3.70236698911837));
#59125=CARTESIAN_POINT('Ctrl Pts',(1.97408973726149,1.,-3.70236698911837));
#59126=CARTESIAN_POINT('Ctrl Pts',(1.974177276451,-1.,-3.7055100813194));
#59127=CARTESIAN_POINT('Ctrl Pts',(1.974177276451,1.,-3.7055100813194));
#59128=CARTESIAN_POINT('Ctrl Pts',(1.97421938526992,-1.,-3.70708211654725));
#59129=CARTESIAN_POINT('Ctrl Pts',(1.97421938526992,1.,-3.70708211654725));
#59130=CARTESIAN_POINT('',(1.88097764062542,1.,-3.24413672884902));
#59131=CARTESIAN_POINT('Ctrl Pts',(1.88097764062541,-1.,-3.24413672884902));
#59132=CARTESIAN_POINT('Ctrl Pts',(1.88097764062541,-0.666666666666667,
-3.24413672884902));
#59133=CARTESIAN_POINT('Ctrl Pts',(1.88097764062541,-0.333333333333333,
-3.24413672884902));
#59134=CARTESIAN_POINT('Ctrl Pts',(1.88097764062541,0.333333333333333,-3.24413672884902));
#59135=CARTESIAN_POINT('Ctrl Pts',(1.88097764062541,0.666666666666667,-3.24413672884902));
#59136=CARTESIAN_POINT('Ctrl Pts',(1.88097764062541,1.,-3.24413672884902));
#59137=CARTESIAN_POINT('',(1.97421938526992,1.,-3.70708211654725));
#59138=CARTESIAN_POINT('',(1.97421938526992,0.,-3.70708211654725));
#59139=CARTESIAN_POINT('Ctrl Pts',(1.88097764062542,1.,-3.24413672884902));
#59140=CARTESIAN_POINT('Ctrl Pts',(1.88102292397987,1.,-3.24415531671311));
#59141=CARTESIAN_POINT('Ctrl Pts',(1.88117508446657,1.,-3.24428080352952));
#59142=CARTESIAN_POINT('Ctrl Pts',(1.88156537699118,1.,-3.24480754675942));
#59143=CARTESIAN_POINT('Ctrl Pts',(1.88242596600422,1.,-3.24625654410705));
#59144=CARTESIAN_POINT('Ctrl Pts',(1.88407708646435,1.,-3.24935200512055));
#59145=CARTESIAN_POINT('Ctrl Pts',(1.88646802523372,1.,-3.25408686339298));
#59146=CARTESIAN_POINT('Ctrl Pts',(1.88934996203508,1.,-3.2599988519361));
#59147=CARTESIAN_POINT('Ctrl Pts',(1.89255393500769,1.,-3.2667765388833));
#59148=CARTESIAN_POINT('Ctrl Pts',(1.89589172903662,1.,-3.27407108932908));
#59149=CARTESIAN_POINT('Ctrl Pts',(1.89918429230424,1.,-3.28154737912287));
#59150=CARTESIAN_POINT('Ctrl Pts',(1.9022897124757,1.,-3.28893448600364));
#59151=CARTESIAN_POINT('Ctrl Pts',(1.9051389186417,1.,-3.29608978722258));
#59152=CARTESIAN_POINT('Ctrl Pts',(1.90773912171424,1.,-3.30300595568341));
#59153=CARTESIAN_POINT('Ctrl Pts',(1.91014297830502,1.,-3.30975721158694));
#59154=CARTESIAN_POINT('Ctrl Pts',(1.91242616234459,1.,-3.31646052426395));
#59155=CARTESIAN_POINT('Ctrl Pts',(1.91466343916612,1.,-3.32323403454507));
#59156=CARTESIAN_POINT('Ctrl Pts',(1.91690081930297,1.,-3.33014884257812));
#59157=CARTESIAN_POINT('Ctrl Pts',(1.91914609610173,1.,-3.33721230709948));
#59158=CARTESIAN_POINT('Ctrl Pts',(1.92138450828378,1.,-3.34439448941915));
#59159=CARTESIAN_POINT('Ctrl Pts',(1.92358838440518,1.,-3.35164424847207));
#59160=CARTESIAN_POINT('Ctrl Pts',(1.92572846125763,1.,-3.35890824422976));
#59161=CARTESIAN_POINT('Ctrl Pts',(1.92778626543803,1.,-3.36615168657597));
#59162=CARTESIAN_POINT('Ctrl Pts',(1.92975993109897,1.,-3.37336807068078));
#59163=CARTESIAN_POINT('Ctrl Pts',(1.93165739093292,1.,-3.38056768525577));
#59164=CARTESIAN_POINT('Ctrl Pts',(1.93349233176794,1.,-3.38777076883267));
#59165=CARTESIAN_POINT('Ctrl Pts',(1.93527929945982,1.,-3.39499923640789));
#59166=CARTESIAN_POINT('Ctrl Pts',(1.93702857723089,1.,-3.40226802104093));
#59167=CARTESIAN_POINT('Ctrl Pts',(1.93874306008132,1.,-3.40957978266623));
#59168=CARTESIAN_POINT('Ctrl Pts',(1.94042111965237,1.,-3.41692971994082));
#59169=CARTESIAN_POINT('Ctrl Pts',(1.94205835913692,1.,-3.42430850941497));
#59170=CARTESIAN_POINT('Ctrl Pts',(1.94364973660285,1.,-3.43170586602436));
#59171=CARTESIAN_POINT('Ctrl Pts',(1.94519168842883,1.,-3.43911410197693));
#59172=CARTESIAN_POINT('Ctrl Pts',(1.94668377715332,1.,-3.44653088665685));
#59173=CARTESIAN_POINT('Ctrl Pts',(1.94812754766524,1.,-3.45395731584051));
#59174=CARTESIAN_POINT('Ctrl Pts',(1.94952575850196,1.,-3.46139661060959));
#59175=CARTESIAN_POINT('Ctrl Pts',(1.95088147859876,1.,-3.4688525897419));
#59176=CARTESIAN_POINT('Ctrl Pts',(1.95219722189878,1.,-3.47632820495926));
#59177=CARTESIAN_POINT('Ctrl Pts',(1.95347412486316,1.,-3.48382414832649));
#59178=CARTESIAN_POINT('Ctrl Pts',(1.95471236969653,1.,-3.49133956289154));
#59179=CARTESIAN_POINT('Ctrl Pts',(1.9559115382367,1.,-3.49887263575602));
#59180=CARTESIAN_POINT('Ctrl Pts',(1.95707099606513,1.,-3.50642124159913));
#59181=CARTESIAN_POINT('Ctrl Pts',(1.95819025316768,1.,-3.51398354617773));
#59182=CARTESIAN_POINT('Ctrl Pts',(1.95926936324436,1.,-3.52155867431438));
#59183=CARTESIAN_POINT('Ctrl Pts',(1.96030879411534,1.,-3.52914648844289));
#59184=CARTESIAN_POINT('Ctrl Pts',(1.96130926212661,1.,-3.53674730625759));
#59185=CARTESIAN_POINT('Ctrl Pts',(1.96227157573058,1.,-3.54436163300425));
#59186=CARTESIAN_POINT('Ctrl Pts',(1.96319648628667,1.,-3.55198990600929));
#59187=CARTESIAN_POINT('Ctrl Pts',(1.96408450906868,1.,-3.55963218706201));
#59188=CARTESIAN_POINT('Ctrl Pts',(1.96493594634643,1.,-3.56728820357933));
#59189=CARTESIAN_POINT('Ctrl Pts',(1.96575096652857,1.,-3.57495748601088));
#59190=CARTESIAN_POINT('Ctrl Pts',(1.9665296668894,1.,-3.58263947663884));
#59191=CARTESIAN_POINT('Ctrl Pts',(1.96727213799507,1.,-3.5903336402273));
#59192=CARTESIAN_POINT('Ctrl Pts',(1.96797854118257,1.,-3.59803959819725));
#59193=CARTESIAN_POINT('Ctrl Pts',(1.96864911885775,1.,-3.60575714017676));
#59194=CARTESIAN_POINT('Ctrl Pts',(1.96928416040712,1.,-3.61348615496393));
#59195=CARTESIAN_POINT('Ctrl Pts',(1.96988398129888,1.,-3.62122658401722));
#59196=CARTESIAN_POINT('Ctrl Pts',(1.97044889850518,1.,-3.62897836973397));
#59197=CARTESIAN_POINT('Ctrl Pts',(1.97097920454698,1.,-3.63674139590853));
#59198=CARTESIAN_POINT('Ctrl Pts',(1.97147515441539,1.,-3.64451546724222));
#59199=CARTESIAN_POINT('Ctrl Pts',(1.97193697240645,1.,-3.65230034717364));
#59200=CARTESIAN_POINT('Ctrl Pts',(1.97236485439317,1.,-3.66009578166865));
#59201=CARTESIAN_POINT('Ctrl Pts',(1.9727589719863,1.,-3.66790152751984));
#59202=CARTESIAN_POINT('Ctrl Pts',(1.97311947678035,1.,-3.67571738106175));
#59203=CARTESIAN_POINT('Ctrl Pts',(1.9734465030363,1.,-3.68354319913416));
#59204=CARTESIAN_POINT('Ctrl Pts',(1.97374016224397,1.,-3.69137888597855));
#59205=CARTESIAN_POINT('Ctrl Pts',(1.97394846382288,1.,-3.69765528558292));
#59206=CARTESIAN_POINT('Ctrl Pts',(1.97408973726149,1.,-3.70236698911837));
#59207=CARTESIAN_POINT('Ctrl Pts',(1.974177276451,1.,-3.7055100813194));
#59208=CARTESIAN_POINT('Ctrl Pts',(1.97421938526992,1.,-3.70708211654725));
#59209=CARTESIAN_POINT('Origin',(1.97421938526992,0.,-3.70708211654725));
#59210=CARTESIAN_POINT('',(1.83867539237861,1.,-3.77614523045147));
#59211=CARTESIAN_POINT('Origin',(0.,0.,0.));
#59212=CARTESIAN_POINT('',(2.03660101169564,1.,-3.14877060440425));
#59213=CARTESIAN_POINT('Origin',(0.,1.,0.));
#59214=CARTESIAN_POINT('Ctrl Pts',(2.03660101169564,1.,-3.14877060440425));
#59215=CARTESIAN_POINT('Ctrl Pts',(2.03660101169564,0.666666666666667,-3.14877060440425));
#59216=CARTESIAN_POINT('Ctrl Pts',(2.03660101169564,0.333333333333333,-3.14877060440425));
#59217=CARTESIAN_POINT('Ctrl Pts',(2.03660101169564,-0.333333333333333,
-3.14877060440425));
#59218=CARTESIAN_POINT('Ctrl Pts',(2.03660101169564,-0.666666666666667,
-3.14877060440425));
#59219=CARTESIAN_POINT('Ctrl Pts',(2.03660101169564,-1.,-3.14877060440425));
#59220=CARTESIAN_POINT('Ctrl Pts',(2.40675750623143,-1.,-3.44202241512147));
#59221=CARTESIAN_POINT('Ctrl Pts',(2.40675750623143,1.,-3.44202241512147));
#59222=CARTESIAN_POINT('Ctrl Pts',(2.40537592959345,-1.,-3.44127120683402));
#59223=CARTESIAN_POINT('Ctrl Pts',(2.40537592959345,1.,-3.44127120683402));
#59224=CARTESIAN_POINT('Ctrl Pts',(2.40261515590099,-1.,-3.43976627485223));
#59225=CARTESIAN_POINT('Ctrl Pts',(2.40261515590099,1.,-3.43976627485223));
#59226=CARTESIAN_POINT('Ctrl Pts',(2.39848113411428,-1.,-3.43750133066037));
#59227=CARTESIAN_POINT('Ctrl Pts',(2.39848113411428,1.,-3.43750133066037));
#59228=CARTESIAN_POINT('Ctrl Pts',(2.39298338805823,-1.,-3.43446630680436));
#59229=CARTESIAN_POINT('Ctrl Pts',(2.39298338805823,1.,-3.43446630680436));
#59230=CARTESIAN_POINT('Ctrl Pts',(2.38613505844641,-1.,-3.43064732714472));
#59231=CARTESIAN_POINT('Ctrl Pts',(2.38613505844641,1.,-3.43064732714472));
#59232=CARTESIAN_POINT('Ctrl Pts',(2.37931067029517,-1.,-3.42680309755241));
#59233=CARTESIAN_POINT('Ctrl Pts',(2.37931067029517,1.,-3.42680309755241));
#59234=CARTESIAN_POINT('Ctrl Pts',(2.37251035954351,-1.,-3.42293356216595));
#59235=CARTESIAN_POINT('Ctrl Pts',(2.37251035954351,1.,-3.42293356216595));
#59236=CARTESIAN_POINT('Ctrl Pts',(2.36573431470313,-1.,-3.41903866635384));
#59237=CARTESIAN_POINT('Ctrl Pts',(2.36573431470313,1.,-3.41903866635384));
#59238=CARTESIAN_POINT('Ctrl Pts',(2.35898278606449,-1.,-3.4151183675076));
#59239=CARTESIAN_POINT('Ctrl Pts',(2.35898278606449,1.,-3.4151183675076));
#59240=CARTESIAN_POINT('Ctrl Pts',(2.35225606823649,-1.,-3.41117262313464));
#59241=CARTESIAN_POINT('Ctrl Pts',(2.35225606823649,1.,-3.41117262313464));
#59242=CARTESIAN_POINT('Ctrl Pts',(2.34555447648901,-1.,-3.40720137403888));
#59243=CARTESIAN_POINT('Ctrl Pts',(2.34555447648901,1.,-3.40720137403888));
#59244=CARTESIAN_POINT('Ctrl Pts',(2.33887832342715,-1.,-3.40320452776646));
#59245=CARTESIAN_POINT('Ctrl Pts',(2.33887832342715,1.,-3.40320452776646));
#59246=CARTESIAN_POINT('Ctrl Pts',(2.33222789882601,-1.,-3.39918194578115));
#59247=CARTESIAN_POINT('Ctrl Pts',(2.33222789882601,1.,-3.39918194578115));
#59248=CARTESIAN_POINT('Ctrl Pts',(2.32560343902683,-1.,-3.39513342020045));
#59249=CARTESIAN_POINT('Ctrl Pts',(2.32560343902683,1.,-3.39513342020045));
#59250=CARTESIAN_POINT('Ctrl Pts',(2.31900513925627,-1.,-3.39105869475112));
#59251=CARTESIAN_POINT('Ctrl Pts',(2.31900513925627,1.,-3.39105869475112));
#59252=CARTESIAN_POINT('Ctrl Pts',(2.31243319489505,-1.,-3.38695751492659));
#59253=CARTESIAN_POINT('Ctrl Pts',(2.31243319489505,1.,-3.38695751492659));
#59254=CARTESIAN_POINT('Ctrl Pts',(2.30588783640389,-1.,-3.38282967336676));
#59255=CARTESIAN_POINT('Ctrl Pts',(2.30588783640389,1.,-3.38282967336676));
#59256=CARTESIAN_POINT('Ctrl Pts',(2.29936936127588,-1.,-3.37867504959382));
#59257=CARTESIAN_POINT('Ctrl Pts',(2.29936936127588,1.,-3.37867504959382));
#59258=CARTESIAN_POINT('Ctrl Pts',(2.2928781800731,-1.,-3.37449367172707));
#59259=CARTESIAN_POINT('Ctrl Pts',(2.2928781800731,1.,-3.37449367172707));
#59260=CARTESIAN_POINT('Ctrl Pts',(2.28641481081045,-1.,-3.37028570206357));
#59261=CARTESIAN_POINT('Ctrl Pts',(2.28641481081045,1.,-3.37028570206357));
#59262=CARTESIAN_POINT('Ctrl Pts',(2.27997979457968,-1.,-3.36605130712978));
#59263=CARTESIAN_POINT('Ctrl Pts',(2.27997979457968,1.,-3.36605130712978));
#59264=CARTESIAN_POINT('Ctrl Pts',(2.27357362620902,-1.,-3.36179055004369));
#59265=CARTESIAN_POINT('Ctrl Pts',(2.27357362620902,1.,-3.36179055004369));
#59266=CARTESIAN_POINT('Ctrl Pts',(2.26719668579921,-1.,-3.35750328523077));
#59267=CARTESIAN_POINT('Ctrl Pts',(2.26719668579921,1.,-3.35750328523077));
#59268=CARTESIAN_POINT('Ctrl Pts',(2.26084915222484,-1.,-3.35318902552676));
#59269=CARTESIAN_POINT('Ctrl Pts',(2.26084915222484,1.,-3.35318902552676));
#59270=CARTESIAN_POINT('Ctrl Pts',(2.25453097693524,-1.,-3.34884690292342));
#59271=CARTESIAN_POINT('Ctrl Pts',(2.25453097693524,1.,-3.34884690292342));
#59272=CARTESIAN_POINT('Ctrl Pts',(2.24824207678287,-1.,-3.34447596770768));
#59273=CARTESIAN_POINT('Ctrl Pts',(2.24824207678287,1.,-3.34447596770768));
#59274=CARTESIAN_POINT('Ctrl Pts',(2.24198249391437,-1.,-3.34007543738044));
#59275=CARTESIAN_POINT('Ctrl Pts',(2.24198249391437,1.,-3.34007543738044));
#59276=CARTESIAN_POINT('Ctrl Pts',(2.23575256328809,-1.,-3.33564495756478));
#59277=CARTESIAN_POINT('Ctrl Pts',(2.23575256328809,1.,-3.33564495756478));
#59278=CARTESIAN_POINT('Ctrl Pts',(2.22955308907221,-1.,-3.33118487773593));
#59279=CARTESIAN_POINT('Ctrl Pts',(2.22955308907221,1.,-3.33118487773593));
#59280=CARTESIAN_POINT('Ctrl Pts',(2.22338548312758,-1.,-3.32669646722871));
#59281=CARTESIAN_POINT('Ctrl Pts',(2.22338548312758,1.,-3.32669646722871));
#59282=CARTESIAN_POINT('Ctrl Pts',(2.21725135110889,-1.,-3.32218125618955));
#59283=CARTESIAN_POINT('Ctrl Pts',(2.21725135110889,1.,-3.32218125618955));
#59284=CARTESIAN_POINT('Ctrl Pts',(2.21115211847872,-1.,-3.31764044024231));
#59285=CARTESIAN_POINT('Ctrl Pts',(2.21115211847872,1.,-3.31764044024231));
#59286=CARTESIAN_POINT('Ctrl Pts',(2.20508863150608,-1.,-3.3130742460895));
#59287=CARTESIAN_POINT('Ctrl Pts',(2.20508863150608,1.,-3.3130742460895));
#59288=CARTESIAN_POINT('Ctrl Pts',(2.19906078949924,-1.,-3.30848134694597));
#59289=CARTESIAN_POINT('Ctrl Pts',(2.19906078949924,1.,-3.30848134694597));
#59290=CARTESIAN_POINT('Ctrl Pts',(2.19306710376112,-1.,-3.30385816281831));
#59291=CARTESIAN_POINT('Ctrl Pts',(2.19306710376112,1.,-3.30385816281831));
#59292=CARTESIAN_POINT('Ctrl Pts',(2.18710556500325,-1.,-3.29920022557635));
#59293=CARTESIAN_POINT('Ctrl Pts',(2.18710556500325,1.,-3.29920022557635));
#59294=CARTESIAN_POINT('Ctrl Pts',(2.18117455557062,-1.,-3.29450361500484));
#59295=CARTESIAN_POINT('Ctrl Pts',(2.18117455557062,1.,-3.29450361500484));
#59296=CARTESIAN_POINT('Ctrl Pts',(2.17527380048422,-1.,-3.28976645712566));
#59297=CARTESIAN_POINT('Ctrl Pts',(2.17527380048422,1.,-3.28976645712566));
#59298=CARTESIAN_POINT('Ctrl Pts',(2.16940517773459,-1.,-3.2849901997973));
#59299=CARTESIAN_POINT('Ctrl Pts',(2.16940517773459,1.,-3.2849901997973));
#59300=CARTESIAN_POINT('Ctrl Pts',(2.16357391934434,-1.,-3.28018150841414));
#59301=CARTESIAN_POINT('Ctrl Pts',(2.16357391934434,1.,-3.28018150841414));
#59302=CARTESIAN_POINT('Ctrl Pts',(2.15778690038359,-1.,-3.27534954469206));
#59303=CARTESIAN_POINT('Ctrl Pts',(2.15778690038359,1.,-3.27534954469206));
#59304=CARTESIAN_POINT('Ctrl Pts',(2.15205043199818,-1.,-3.27050245897244));
#59305=CARTESIAN_POINT('Ctrl Pts',(2.15205043199818,1.,-3.27050245897244));
#59306=CARTESIAN_POINT('Ctrl Pts',(2.14636805295663,-1.,-3.26564388189764));
#59307=CARTESIAN_POINT('Ctrl Pts',(2.14636805295663,1.,-3.26564388189764));
#59308=CARTESIAN_POINT('Ctrl Pts',(2.14073870754257,-1.,-3.26077002641868));
#59309=CARTESIAN_POINT('Ctrl Pts',(2.14073870754257,1.,-3.26077002641868));
#59310=CARTESIAN_POINT('Ctrl Pts',(2.13515375878786,-1.,-3.25586495065027));
#59311=CARTESIAN_POINT('Ctrl Pts',(2.13515375878786,1.,-3.25586495065027));
#59312=CARTESIAN_POINT('Ctrl Pts',(2.1296002839681,-1.,-3.25090574493994));
#59313=CARTESIAN_POINT('Ctrl Pts',(2.1296002839681,1.,-3.25090574493994));
#59314=CARTESIAN_POINT('Ctrl Pts',(2.12406646410943,-1.,-3.24587102613347));
#59315=CARTESIAN_POINT('Ctrl Pts',(2.12406646410943,1.,-3.24587102613347));
#59316=CARTESIAN_POINT('Ctrl Pts',(2.11854673326972,-1.,-3.24074905517282));
#59317=CARTESIAN_POINT('Ctrl Pts',(2.11854673326972,1.,-3.24074905517282));
#59318=CARTESIAN_POINT('Ctrl Pts',(2.11304604021784,-1.,-3.23554444767115));
#59319=CARTESIAN_POINT('Ctrl Pts',(2.11304604021784,1.,-3.23554444767115));
#59320=CARTESIAN_POINT('Ctrl Pts',(2.1075869964248,-1.,-3.23028945793334));
#59321=CARTESIAN_POINT('Ctrl Pts',(2.1075869964248,1.,-3.23028945793334));
#59322=CARTESIAN_POINT('Ctrl Pts',(2.10220384298533,-1.,-3.22503437553496));
#59323=CARTESIAN_POINT('Ctrl Pts',(2.10220384298533,1.,-3.22503437553496));
#59324=CARTESIAN_POINT('Ctrl Pts',(2.09692958434933,-1.,-3.21982707347067));
#59325=CARTESIAN_POINT('Ctrl Pts',(2.09692958434933,1.,-3.21982707347067));
#59326=CARTESIAN_POINT('Ctrl Pts',(2.0917841946046,-1.,-3.2146942960168));
#59327=CARTESIAN_POINT('Ctrl Pts',(2.0917841946046,1.,-3.2146942960168));
#59328=CARTESIAN_POINT('Ctrl Pts',(2.08676465517435,-1.,-3.20962575845433));
#59329=CARTESIAN_POINT('Ctrl Pts',(2.08676465517435,1.,-3.20962575845433));
#59330=CARTESIAN_POINT('Ctrl Pts',(2.08182850370816,-1.,-3.20454818630635));
#59331=CARTESIAN_POINT('Ctrl Pts',(2.08182850370816,1.,-3.20454818630635));
#59332=CARTESIAN_POINT('Ctrl Pts',(2.0769044187063,-1.,-3.19934132835879));
#59333=CARTESIAN_POINT('Ctrl Pts',(2.0769044187063,1.,-3.19934132835879));
#59334=CARTESIAN_POINT('Ctrl Pts',(2.07192253497765,-1.,-3.19388465568113));
#59335=CARTESIAN_POINT('Ctrl Pts',(2.07192253497765,1.,-3.19388465568113));
#59336=CARTESIAN_POINT('Ctrl Pts',(2.06684062744065,-1.,-3.18809755562297));
#59337=CARTESIAN_POINT('Ctrl Pts',(2.06684062744065,1.,-3.18809755562297));
#59338=CARTESIAN_POINT('Ctrl Pts',(2.06166849827143,-1.,-3.18197692964677));
#59339=CARTESIAN_POINT('Ctrl Pts',(2.06166849827143,1.,-3.18197692964677));
#59340=CARTESIAN_POINT('Ctrl Pts',(2.05650186773279,-1.,-3.17564906975592));
#59341=CARTESIAN_POINT('Ctrl Pts',(2.05650186773279,1.,-3.17564906975592));
#59342=CARTESIAN_POINT('Ctrl Pts',(2.05151770247452,-1.,-3.16936341689859));
#59343=CARTESIAN_POINT('Ctrl Pts',(2.05151770247452,1.,-3.16936341689859));
#59344=CARTESIAN_POINT('Ctrl Pts',(2.0469333124766,-1.,-3.16343165059235));
#59345=CARTESIAN_POINT('Ctrl Pts',(2.0469333124766,1.,-3.16343165059235));
#59346=CARTESIAN_POINT('Ctrl Pts',(2.04297406404132,-1.,-3.15817983946525));
#59347=CARTESIAN_POINT('Ctrl Pts',(2.04297406404132,1.,-3.15817983946525));
#59348=CARTESIAN_POINT('Ctrl Pts',(2.03984073791432,-1.,-3.1538999167466));
#59349=CARTESIAN_POINT('Ctrl Pts',(2.03984073791432,1.,-3.1538999167466));
#59350=CARTESIAN_POINT('Ctrl Pts',(2.03766932526171,-1.,-3.15079010635326));
#59351=CARTESIAN_POINT('Ctrl Pts',(2.03766932526171,1.,-3.15079010635326));
#59352=CARTESIAN_POINT('Ctrl Pts',(2.03675273048882,-1.,-3.14931281967585));
#59353=CARTESIAN_POINT('Ctrl Pts',(2.03675273048882,1.,-3.14931281967585));
#59354=CARTESIAN_POINT('Ctrl Pts',(2.03653654935384,-1.,-3.14878756590499));
#59355=CARTESIAN_POINT('Ctrl Pts',(2.03653654935384,1.,-3.14878756590499));
#59356=CARTESIAN_POINT('Ctrl Pts',(2.036601737578,-1.,-3.14869618937139));
#59357=CARTESIAN_POINT('Ctrl Pts',(2.036601737578,1.,-3.14869618937139));
#59358=CARTESIAN_POINT('Ctrl Pts',(2.03668666247593,-1.,-3.1487152044751));
#59359=CARTESIAN_POINT('Ctrl Pts',(2.03668666247593,1.,-3.1487152044751));
#59360=CARTESIAN_POINT('',(2.40675750623143,1.,-3.44202241512147));
#59361=CARTESIAN_POINT('Ctrl Pts',(2.40675750623143,1.,-3.44202241512147));
#59362=CARTESIAN_POINT('Ctrl Pts',(2.40537592959345,1.,-3.44127120683402));
#59363=CARTESIAN_POINT('Ctrl Pts',(2.40261515590099,1.,-3.43976627485223));
#59364=CARTESIAN_POINT('Ctrl Pts',(2.39848113411428,1.,-3.43750133066037));
#59365=CARTESIAN_POINT('Ctrl Pts',(2.39298338805823,1.,-3.43446630680436));
#59366=CARTESIAN_POINT('Ctrl Pts',(2.38613505844641,1.,-3.43064732714472));
#59367=CARTESIAN_POINT('Ctrl Pts',(2.37931067029517,1.,-3.42680309755241));
#59368=CARTESIAN_POINT('Ctrl Pts',(2.37251035954351,1.,-3.42293356216595));
#59369=CARTESIAN_POINT('Ctrl Pts',(2.36573431470313,1.,-3.41903866635384));
#59370=CARTESIAN_POINT('Ctrl Pts',(2.35898278606449,1.,-3.4151183675076));
#59371=CARTESIAN_POINT('Ctrl Pts',(2.35225606823649,1.,-3.41117262313464));
#59372=CARTESIAN_POINT('Ctrl Pts',(2.34555447648901,1.,-3.40720137403888));
#59373=CARTESIAN_POINT('Ctrl Pts',(2.33887832342715,1.,-3.40320452776646));
#59374=CARTESIAN_POINT('Ctrl Pts',(2.33222789882601,1.,-3.39918194578115));
#59375=CARTESIAN_POINT('Ctrl Pts',(2.32560343902683,1.,-3.39513342020045));
#59376=CARTESIAN_POINT('Ctrl Pts',(2.31900513925627,1.,-3.39105869475112));
#59377=CARTESIAN_POINT('Ctrl Pts',(2.31243319489505,1.,-3.38695751492659));
#59378=CARTESIAN_POINT('Ctrl Pts',(2.30588783640389,1.,-3.38282967336676));
#59379=CARTESIAN_POINT('Ctrl Pts',(2.29936936127588,1.,-3.37867504959382));
#59380=CARTESIAN_POINT('Ctrl Pts',(2.2928781800731,1.,-3.37449367172707));
#59381=CARTESIAN_POINT('Ctrl Pts',(2.28641481081045,1.,-3.37028570206357));
#59382=CARTESIAN_POINT('Ctrl Pts',(2.27997979457968,1.,-3.36605130712978));
#59383=CARTESIAN_POINT('Ctrl Pts',(2.27357362620902,1.,-3.36179055004369));
#59384=CARTESIAN_POINT('Ctrl Pts',(2.26719668579921,1.,-3.35750328523077));
#59385=CARTESIAN_POINT('Ctrl Pts',(2.26084915222484,1.,-3.35318902552676));
#59386=CARTESIAN_POINT('Ctrl Pts',(2.25453097693524,1.,-3.34884690292342));
#59387=CARTESIAN_POINT('Ctrl Pts',(2.24824207678287,1.,-3.34447596770768));
#59388=CARTESIAN_POINT('Ctrl Pts',(2.24198249391437,1.,-3.34007543738044));
#59389=CARTESIAN_POINT('Ctrl Pts',(2.23575256328809,1.,-3.33564495756478));
#59390=CARTESIAN_POINT('Ctrl Pts',(2.22955308907221,1.,-3.33118487773593));
#59391=CARTESIAN_POINT('Ctrl Pts',(2.22338548312758,1.,-3.32669646722871));
#59392=CARTESIAN_POINT('Ctrl Pts',(2.21725135110889,1.,-3.32218125618955));
#59393=CARTESIAN_POINT('Ctrl Pts',(2.21115211847872,1.,-3.31764044024231));
#59394=CARTESIAN_POINT('Ctrl Pts',(2.20508863150608,1.,-3.3130742460895));
#59395=CARTESIAN_POINT('Ctrl Pts',(2.19906078949924,1.,-3.30848134694597));
#59396=CARTESIAN_POINT('Ctrl Pts',(2.19306710376112,1.,-3.30385816281831));
#59397=CARTESIAN_POINT('Ctrl Pts',(2.18710556500325,1.,-3.29920022557635));
#59398=CARTESIAN_POINT('Ctrl Pts',(2.18117455557062,1.,-3.29450361500484));
#59399=CARTESIAN_POINT('Ctrl Pts',(2.17527380048422,1.,-3.28976645712566));
#59400=CARTESIAN_POINT('Ctrl Pts',(2.16940517773459,1.,-3.2849901997973));
#59401=CARTESIAN_POINT('Ctrl Pts',(2.16357391934434,1.,-3.28018150841414));
#59402=CARTESIAN_POINT('Ctrl Pts',(2.15778690038359,1.,-3.27534954469206));
#59403=CARTESIAN_POINT('Ctrl Pts',(2.15205043199818,1.,-3.27050245897244));
#59404=CARTESIAN_POINT('Ctrl Pts',(2.14636805295663,1.,-3.26564388189764));
#59405=CARTESIAN_POINT('Ctrl Pts',(2.14073870754257,1.,-3.26077002641868));
#59406=CARTESIAN_POINT('Ctrl Pts',(2.13515375878786,1.,-3.25586495065027));
#59407=CARTESIAN_POINT('Ctrl Pts',(2.1296002839681,1.,-3.25090574493994));
#59408=CARTESIAN_POINT('Ctrl Pts',(2.12406646410943,1.,-3.24587102613347));
#59409=CARTESIAN_POINT('Ctrl Pts',(2.11854673326972,1.,-3.24074905517282));
#59410=CARTESIAN_POINT('Ctrl Pts',(2.11304604021784,1.,-3.23554444767115));
#59411=CARTESIAN_POINT('Ctrl Pts',(2.1075869964248,1.,-3.23028945793334));
#59412=CARTESIAN_POINT('Ctrl Pts',(2.10220384298533,1.,-3.22503437553496));
#59413=CARTESIAN_POINT('Ctrl Pts',(2.09692958434933,1.,-3.21982707347067));
#59414=CARTESIAN_POINT('Ctrl Pts',(2.0917841946046,1.,-3.2146942960168));
#59415=CARTESIAN_POINT('Ctrl Pts',(2.08676465517435,1.,-3.20962575845433));
#59416=CARTESIAN_POINT('Ctrl Pts',(2.08182850370816,1.,-3.20454818630635));
#59417=CARTESIAN_POINT('Ctrl Pts',(2.0769044187063,1.,-3.19934132835879));
#59418=CARTESIAN_POINT('Ctrl Pts',(2.07192253497765,1.,-3.19388465568113));
#59419=CARTESIAN_POINT('Ctrl Pts',(2.06684062744065,1.,-3.18809755562297));
#59420=CARTESIAN_POINT('Ctrl Pts',(2.06166849827143,1.,-3.18197692964677));
#59421=CARTESIAN_POINT('Ctrl Pts',(2.05650186773279,1.,-3.17564906975592));
#59422=CARTESIAN_POINT('Ctrl Pts',(2.05151770247452,1.,-3.16936341689859));
#59423=CARTESIAN_POINT('Ctrl Pts',(2.0469333124766,1.,-3.16343165059235));
#59424=CARTESIAN_POINT('Ctrl Pts',(2.04297406404132,1.,-3.15817983946525));
#59425=CARTESIAN_POINT('Ctrl Pts',(2.03984073791432,1.,-3.1538999167466));
#59426=CARTESIAN_POINT('Ctrl Pts',(2.03783225496023,1.,-3.15102344775396));
#59427=CARTESIAN_POINT('Ctrl Pts',(2.03693188810614,1.,-3.14959882629936));
#59428=CARTESIAN_POINT('Ctrl Pts',(2.03663974554941,1.,-3.14901193669147));
#59429=CARTESIAN_POINT('Ctrl Pts',(2.03659701539175,1.,-3.1488193908823));
#59430=CARTESIAN_POINT('Ctrl Pts',(2.03660101169564,1.,-3.14877060440425));
#59431=CARTESIAN_POINT('',(2.40675750623143,0.,-3.44202241512147));
#59432=CARTESIAN_POINT('Ctrl Pts',(2.36523532225181,-1.,-2.91001063062876));
#59433=CARTESIAN_POINT('Ctrl Pts',(2.36523532225181,1.,-2.91001063062876));
#59434=CARTESIAN_POINT('Ctrl Pts',(2.36524348105112,-1.,-2.90992398626211));
#59435=CARTESIAN_POINT('Ctrl Pts',(2.36524348105112,1.,-2.90992398626211));
#59436=CARTESIAN_POINT('Ctrl Pts',(2.36535052956938,-1.,-2.90989022548032));
#59437=CARTESIAN_POINT('Ctrl Pts',(2.36535052956938,1.,-2.90989022548032));
#59438=CARTESIAN_POINT('Ctrl Pts',(2.36578327194741,-1.,-2.91025813830041));
#59439=CARTESIAN_POINT('Ctrl Pts',(2.36578327194741,1.,-2.91025813830041));
#59440=CARTESIAN_POINT('Ctrl Pts',(2.36690501170627,-1.,-2.9115863784204));
#59441=CARTESIAN_POINT('Ctrl Pts',(2.36690501170627,1.,-2.9115863784204));
#59442=CARTESIAN_POINT('Ctrl Pts',(2.36919161373173,-1.,-2.9146124988314));
#59443=CARTESIAN_POINT('Ctrl Pts',(2.36919161373173,1.,-2.9146124988314));
#59444=CARTESIAN_POINT('Ctrl Pts',(2.37229381109821,-1.,-2.91891503791411));
#59445=CARTESIAN_POINT('Ctrl Pts',(2.37229381109821,1.,-2.91891503791411));
#59446=CARTESIAN_POINT('Ctrl Pts',(2.3760651052403,-1.,-2.92430340582608));
#59447=CARTESIAN_POINT('Ctrl Pts',(2.3760651052403,1.,-2.92430340582608));
#59448=CARTESIAN_POINT('Ctrl Pts',(2.38028989582073,-1.,-2.93049643640206));
#59449=CARTESIAN_POINT('Ctrl Pts',(2.38028989582073,1.,-2.93049643640206));
#59450=CARTESIAN_POINT('Ctrl Pts',(2.38472771516311,-1.,-2.93717903280391));
#59451=CARTESIAN_POINT('Ctrl Pts',(2.38472771516311,1.,-2.93717903280391));
#59452=CARTESIAN_POINT('Ctrl Pts',(2.38914929090759,-1.,-2.94404820669076));
#59453=CARTESIAN_POINT('Ctrl Pts',(2.38914929090759,1.,-2.94404820669076));
#59454=CARTESIAN_POINT('Ctrl Pts',(2.39337207631667,-1.,-2.95085857128439));
#59455=CARTESIAN_POINT('Ctrl Pts',(2.39337207631667,1.,-2.95085857128439));
#59456=CARTESIAN_POINT('Ctrl Pts',(2.39730553974516,-1.,-2.95748006482942));
#59457=CARTESIAN_POINT('Ctrl Pts',(2.39730553974516,1.,-2.95748006482942));
#59458=CARTESIAN_POINT('Ctrl Pts',(2.4009556571164,-1.,-2.96390432240312));
#59459=CARTESIAN_POINT('Ctrl Pts',(2.4009556571164,1.,-2.96390432240312));
#59460=CARTESIAN_POINT('Ctrl Pts',(2.40438604734919,-1.,-2.9701964131236));
#59461=CARTESIAN_POINT('Ctrl Pts',(2.40438604734919,1.,-2.9701964131236));
#59462=CARTESIAN_POINT('Ctrl Pts',(2.40768975073713,-1.,-2.97646002822422));
#59463=CARTESIAN_POINT('Ctrl Pts',(2.40768975073713,1.,-2.97646002822422));
#59464=CARTESIAN_POINT('Ctrl Pts',(2.41095909342571,-1.,-2.98280015815107));
#59465=CARTESIAN_POINT('Ctrl Pts',(2.41095909342571,1.,-2.98280015815107));
#59466=CARTESIAN_POINT('Ctrl Pts',(2.41425064199586,-1.,-2.98927983005796));
#59467=CARTESIAN_POINT('Ctrl Pts',(2.41425064199586,1.,-2.98927983005796));
#59468=CARTESIAN_POINT('Ctrl Pts',(2.41757324500514,-1.,-2.99590509293503));
#59469=CARTESIAN_POINT('Ctrl Pts',(2.41757324500514,1.,-2.99590509293503));
#59470=CARTESIAN_POINT('Ctrl Pts',(2.42090763946779,-1.,-3.00264868585996));
#59471=CARTESIAN_POINT('Ctrl Pts',(2.42090763946779,1.,-3.00264868585996));
#59472=CARTESIAN_POINT('Ctrl Pts',(2.42421849439613,-1.,-3.00946442616659));
#59473=CARTESIAN_POINT('Ctrl Pts',(2.42421849439613,1.,-3.00946442616659));
#59474=CARTESIAN_POINT('Ctrl Pts',(2.42746856264168,-1.,-3.01630420830504));
#59475=CARTESIAN_POINT('Ctrl Pts',(2.42746856264168,1.,-3.01630420830504));
#59476=CARTESIAN_POINT('Ctrl Pts',(2.43063415586637,-1.,-3.02313656036004));
#59477=CARTESIAN_POINT('Ctrl Pts',(2.43063415586637,1.,-3.02313656036004));
#59478=CARTESIAN_POINT('Ctrl Pts',(2.43371241361488,-1.,-3.02995534946978));
#59479=CARTESIAN_POINT('Ctrl Pts',(2.43371241361488,1.,-3.02995534946978));
#59480=CARTESIAN_POINT('Ctrl Pts',(2.43671278042414,-1.,-3.03676949672822));
#59481=CARTESIAN_POINT('Ctrl Pts',(2.43671278042414,1.,-3.03676949672822));
#59482=CARTESIAN_POINT('Ctrl Pts',(2.43965194061857,-1.,-3.04359685040555));
#59483=CARTESIAN_POINT('Ctrl Pts',(2.43965194061857,1.,-3.04359685040555));
#59484=CARTESIAN_POINT('Ctrl Pts',(2.44254768923105,-1.,-3.05045678021504));
#59485=CARTESIAN_POINT('Ctrl Pts',(2.44254768923105,1.,-3.05045678021504));
#59486=CARTESIAN_POINT('Ctrl Pts',(2.44541251892556,-1.,-3.05736242671506));
#59487=CARTESIAN_POINT('Ctrl Pts',(2.44541251892556,1.,-3.05736242671506));
#59488=CARTESIAN_POINT('Ctrl Pts',(2.44824970516543,-1.,-3.06431596421405));
#59489=CARTESIAN_POINT('Ctrl Pts',(2.44824970516543,1.,-3.06431596421405));
#59490=CARTESIAN_POINT('Ctrl Pts',(2.45105688854422,-1.,-3.07131290521297));
#59491=CARTESIAN_POINT('Ctrl Pts',(2.45105688854422,1.,-3.07131290521297));
#59492=CARTESIAN_POINT('Ctrl Pts',(2.4538282678779,-1.,-3.07834472886139));
#59493=CARTESIAN_POINT('Ctrl Pts',(2.4538282678779,1.,-3.07834472886139));
#59494=CARTESIAN_POINT('Ctrl Pts',(2.45655725437039,-1.,-3.08540206545315));
#59495=CARTESIAN_POINT('Ctrl Pts',(2.45655725437039,1.,-3.08540206545315));
#59496=CARTESIAN_POINT('Ctrl Pts',(2.4592391256388,-1.,-3.09247787931887));
#59497=CARTESIAN_POINT('Ctrl Pts',(2.4592391256388,1.,-3.09247787931887));
#59498=CARTESIAN_POINT('Ctrl Pts',(2.46187308501884,-1.,-3.09956993697052));
#59499=CARTESIAN_POINT('Ctrl Pts',(2.46187308501884,1.,-3.09956993697052));
#59500=CARTESIAN_POINT('Ctrl Pts',(2.46446082979646,-1.,-3.1066790790198));
#59501=CARTESIAN_POINT('Ctrl Pts',(2.46446082979646,1.,-3.1066790790198));
#59502=CARTESIAN_POINT('Ctrl Pts',(2.46700558843506,-1.,-3.11380805536122));
#59503=CARTESIAN_POINT('Ctrl Pts',(2.46700558843506,1.,-3.11380805536122));
#59504=CARTESIAN_POINT('Ctrl Pts',(2.46951098947469,-1.,-3.12096015766983));
#59505=CARTESIAN_POINT('Ctrl Pts',(2.46951098947469,1.,-3.12096015766983));
#59506=CARTESIAN_POINT('Ctrl Pts',(2.47197997765871,-1.,-3.12813790805952));
#59507=CARTESIAN_POINT('Ctrl Pts',(2.47197997765871,1.,-3.12813790805952));
#59508=CARTESIAN_POINT('Ctrl Pts',(2.47441378371932,-1.,-3.13534181229295));
#59509=CARTESIAN_POINT('Ctrl Pts',(2.47441378371932,1.,-3.13534181229295));
#59510=CARTESIAN_POINT('Ctrl Pts',(2.47681245356109,-1.,-3.1425709954655));
#59511=CARTESIAN_POINT('Ctrl Pts',(2.47681245356109,1.,-3.1425709954655));
#59512=CARTESIAN_POINT('Ctrl Pts',(2.47917529057029,-1.,-3.14982373241352));
#59513=CARTESIAN_POINT('Ctrl Pts',(2.47917529057029,1.,-3.14982373241352));
#59514=CARTESIAN_POINT('Ctrl Pts',(2.48150133566571,-1.,-3.15709802322739));
#59515=CARTESIAN_POINT('Ctrl Pts',(2.48150133566571,1.,-3.15709802322739));
#59516=CARTESIAN_POINT('Ctrl Pts',(2.48378981792725,-1.,-3.16439213290161));
#59517=CARTESIAN_POINT('Ctrl Pts',(2.48378981792725,1.,-3.16439213290161));
#59518=CARTESIAN_POINT('Ctrl Pts',(2.48604065348587,-1.,-3.17170518863313));
#59519=CARTESIAN_POINT('Ctrl Pts',(2.48604065348587,1.,-3.17170518863313));
#59520=CARTESIAN_POINT('Ctrl Pts',(2.48825428288201,-1.,-3.17903698136622));
#59521=CARTESIAN_POINT('Ctrl Pts',(2.48825428288201,1.,-3.17903698136622));
#59522=CARTESIAN_POINT('Ctrl Pts',(2.49043146334059,-1.,-3.18638771282266));
#59523=CARTESIAN_POINT('Ctrl Pts',(2.49043146334059,1.,-3.18638771282266));
#59524=CARTESIAN_POINT('Ctrl Pts',(2.49257307239848,-1.,-3.19375775555798));
#59525=CARTESIAN_POINT('Ctrl Pts',(2.49257307239848,1.,-3.19375775555798));
#59526=CARTESIAN_POINT('Ctrl Pts',(2.49467992057755,-1.,-3.20114742397588));
#59527=CARTESIAN_POINT('Ctrl Pts',(2.49467992057755,1.,-3.20114742397588));
#59528=CARTESIAN_POINT('Ctrl Pts',(2.4967525264737,-1.,-3.20855669849836));
#59529=CARTESIAN_POINT('Ctrl Pts',(2.4967525264737,1.,-3.20855669849836));
#59530=CARTESIAN_POINT('Ctrl Pts',(2.4987911459939,-1.,-3.21598526261286));
#59531=CARTESIAN_POINT('Ctrl Pts',(2.4987911459939,1.,-3.21598526261286));
#59532=CARTESIAN_POINT('Ctrl Pts',(2.50079587201957,-1.,-3.22343262620503));
#59533=CARTESIAN_POINT('Ctrl Pts',(2.50079587201957,1.,-3.22343262620503));
#59534=CARTESIAN_POINT('Ctrl Pts',(2.50276671338111,-1.,-3.23089822320646));
#59535=CARTESIAN_POINT('Ctrl Pts',(2.50276671338111,1.,-3.23089822320646));
#59536=CARTESIAN_POINT('Ctrl Pts',(2.5047036758003,-1.,-3.23838151080319));
#59537=CARTESIAN_POINT('Ctrl Pts',(2.5047036758003,1.,-3.23838151080319));
#59538=CARTESIAN_POINT('Ctrl Pts',(2.506606859405,-1.,-3.24588208983849));
#59539=CARTESIAN_POINT('Ctrl Pts',(2.506606859405,1.,-3.24588208983849));
#59540=CARTESIAN_POINT('Ctrl Pts',(2.50847647070723,-1.,-3.25339971460982));
#59541=CARTESIAN_POINT('Ctrl Pts',(2.50847647070723,1.,-3.25339971460982));
#59542=CARTESIAN_POINT('Ctrl Pts',(2.51031277813486,-1.,-3.26093423001434));
#59543=CARTESIAN_POINT('Ctrl Pts',(2.51031277813486,1.,-3.26093423001434));
#59544=CARTESIAN_POINT('Ctrl Pts',(2.51211608411423,-1.,-3.26848552888116));
#59545=CARTESIAN_POINT('Ctrl Pts',(2.51211608411423,1.,-3.26848552888116));
#59546=CARTESIAN_POINT('Ctrl Pts',(2.513886692704,-1.,-3.27605350473142));
#59547=CARTESIAN_POINT('Ctrl Pts',(2.513886692704,1.,-3.27605350473142));
#59548=CARTESIAN_POINT('Ctrl Pts',(2.51562487464514,-1.,-3.28363799702982));
#59549=CARTESIAN_POINT('Ctrl Pts',(2.51562487464514,1.,-3.28363799702982));
#59550=CARTESIAN_POINT('Ctrl Pts',(2.51733085123797,-1.,-3.2912387729927));
#59551=CARTESIAN_POINT('Ctrl Pts',(2.51733085123797,1.,-3.2912387729927));
#59552=CARTESIAN_POINT('Ctrl Pts',(2.51900480701068,-1.,-3.29885556388353));
#59553=CARTESIAN_POINT('Ctrl Pts',(2.51900480701068,1.,-3.29885556388353));
#59554=CARTESIAN_POINT('Ctrl Pts',(2.52064689568511,-1.,-3.30648808815443));
#59555=CARTESIAN_POINT('Ctrl Pts',(2.52064689568511,1.,-3.30648808815443));
#59556=CARTESIAN_POINT('Ctrl Pts',(2.52225724871313,-1.,-3.31413607874645));
#59557=CARTESIAN_POINT('Ctrl Pts',(2.52225724871313,1.,-3.31413607874645));
#59558=CARTESIAN_POINT('Ctrl Pts',(2.5238359839626,-1.,-3.32179931078699));
#59559=CARTESIAN_POINT('Ctrl Pts',(2.5238359839626,1.,-3.32179931078699));
#59560=CARTESIAN_POINT('Ctrl Pts',(2.52538321164634,-1.,-3.32947762187533));
#59561=CARTESIAN_POINT('Ctrl Pts',(2.52538321164634,1.,-3.32947762187533));
#59562=CARTESIAN_POINT('Ctrl Pts',(2.52689902690158,-1.,-3.33717089999103));
#59563=CARTESIAN_POINT('Ctrl Pts',(2.52689902690158,1.,-3.33717089999103));
#59564=CARTESIAN_POINT('Ctrl Pts',(2.52808660915689,-1.,-3.34333744115511));
#59565=CARTESIAN_POINT('Ctrl Pts',(2.52808660915689,1.,-3.34333744115511));
#59566=CARTESIAN_POINT('Ctrl Pts',(2.52896321610703,-1.,-3.34796903576663));
#59567=CARTESIAN_POINT('Ctrl Pts',(2.52896321610703,1.,-3.34796903576663));
#59568=CARTESIAN_POINT('Ctrl Pts',(2.5295413654909,-1.,-3.35105973714072));
#59569=CARTESIAN_POINT('Ctrl Pts',(2.5295413654909,1.,-3.35105973714072));
#59570=CARTESIAN_POINT('Ctrl Pts',(2.52982887637028,-1.,-3.35260583073571));
#59571=CARTESIAN_POINT('Ctrl Pts',(2.52982887637028,1.,-3.35260583073571));
#59572=CARTESIAN_POINT('',(2.36531447826073,1.,-2.90994629141676));
#59573=CARTESIAN_POINT('Ctrl Pts',(2.36531447826073,-1.,-2.90994629141676));
#59574=CARTESIAN_POINT('Ctrl Pts',(2.36531447826073,-0.666666666666667,
-2.90994629141676));
#59575=CARTESIAN_POINT('Ctrl Pts',(2.36531447826073,-0.333333333333333,
-2.90994629141676));
#59576=CARTESIAN_POINT('Ctrl Pts',(2.36531447826073,0.333333333333333,-2.90994629141676));
#59577=CARTESIAN_POINT('Ctrl Pts',(2.36531447826074,0.666666666666667,-2.90994629141676));
#59578=CARTESIAN_POINT('Ctrl Pts',(2.36531447826074,1.,-2.90994629141676));
#59579=CARTESIAN_POINT('',(2.52982887637028,1.,-3.35260583073571));
#59580=CARTESIAN_POINT('',(2.52982887637028,0.,-3.35260583073571));
#59581=CARTESIAN_POINT('Ctrl Pts',(2.36531447826073,1.,-2.90994629141676));
#59582=CARTESIAN_POINT('Ctrl Pts',(2.36536211188453,1.,-2.90995756655606));
#59583=CARTESIAN_POINT('Ctrl Pts',(2.36553202948613,1.,-2.91005770527719));
#59584=CARTESIAN_POINT('Ctrl Pts',(2.36599991765749,1.,-2.91051690822156));
#59585=CARTESIAN_POINT('Ctrl Pts',(2.36707658451664,1.,-2.91181344022548));
#59586=CARTESIAN_POINT('Ctrl Pts',(2.36919161373173,1.,-2.9146124988314));
#59587=CARTESIAN_POINT('Ctrl Pts',(2.37229381109821,1.,-2.91891503791411));
#59588=CARTESIAN_POINT('Ctrl Pts',(2.3760651052403,1.,-2.92430340582608));
#59589=CARTESIAN_POINT('Ctrl Pts',(2.38028989582073,1.,-2.93049643640206));
#59590=CARTESIAN_POINT('Ctrl Pts',(2.38472771516311,1.,-2.93717903280391));
#59591=CARTESIAN_POINT('Ctrl Pts',(2.38914929090759,1.,-2.94404820669076));
#59592=CARTESIAN_POINT('Ctrl Pts',(2.39337207631667,1.,-2.95085857128439));
#59593=CARTESIAN_POINT('Ctrl Pts',(2.39730553974516,1.,-2.95748006482942));
#59594=CARTESIAN_POINT('Ctrl Pts',(2.4009556571164,1.,-2.96390432240312));
#59595=CARTESIAN_POINT('Ctrl Pts',(2.40438604734919,1.,-2.9701964131236));
#59596=CARTESIAN_POINT('Ctrl Pts',(2.40768975073713,1.,-2.97646002822422));
#59597=CARTESIAN_POINT('Ctrl Pts',(2.41095909342571,1.,-2.98280015815107));
#59598=CARTESIAN_POINT('Ctrl Pts',(2.41425064199586,1.,-2.98927983005796));
#59599=CARTESIAN_POINT('Ctrl Pts',(2.41757324500514,1.,-2.99590509293503));
#59600=CARTESIAN_POINT('Ctrl Pts',(2.42090763946779,1.,-3.00264868585996));
#59601=CARTESIAN_POINT('Ctrl Pts',(2.42421849439613,1.,-3.00946442616659));
#59602=CARTESIAN_POINT('Ctrl Pts',(2.42746856264168,1.,-3.01630420830504));
#59603=CARTESIAN_POINT('Ctrl Pts',(2.43063415586637,1.,-3.02313656036004));
#59604=CARTESIAN_POINT('Ctrl Pts',(2.43371241361488,1.,-3.02995534946978));
#59605=CARTESIAN_POINT('Ctrl Pts',(2.43671278042414,1.,-3.03676949672822));
#59606=CARTESIAN_POINT('Ctrl Pts',(2.43965194061857,1.,-3.04359685040555));
#59607=CARTESIAN_POINT('Ctrl Pts',(2.44254768923105,1.,-3.05045678021504));
#59608=CARTESIAN_POINT('Ctrl Pts',(2.44541251892556,1.,-3.05736242671506));
#59609=CARTESIAN_POINT('Ctrl Pts',(2.44824970516543,1.,-3.06431596421405));
#59610=CARTESIAN_POINT('Ctrl Pts',(2.45105688854422,1.,-3.07131290521297));
#59611=CARTESIAN_POINT('Ctrl Pts',(2.4538282678779,1.,-3.07834472886139));
#59612=CARTESIAN_POINT('Ctrl Pts',(2.45655725437039,1.,-3.08540206545315));
#59613=CARTESIAN_POINT('Ctrl Pts',(2.4592391256388,1.,-3.09247787931887));
#59614=CARTESIAN_POINT('Ctrl Pts',(2.46187308501884,1.,-3.09956993697052));
#59615=CARTESIAN_POINT('Ctrl Pts',(2.46446082979646,1.,-3.1066790790198));
#59616=CARTESIAN_POINT('Ctrl Pts',(2.46700558843506,1.,-3.11380805536122));
#59617=CARTESIAN_POINT('Ctrl Pts',(2.46951098947469,1.,-3.12096015766983));
#59618=CARTESIAN_POINT('Ctrl Pts',(2.47197997765871,1.,-3.12813790805952));
#59619=CARTESIAN_POINT('Ctrl Pts',(2.47441378371932,1.,-3.13534181229295));
#59620=CARTESIAN_POINT('Ctrl Pts',(2.47681245356109,1.,-3.1425709954655));
#59621=CARTESIAN_POINT('Ctrl Pts',(2.47917529057029,1.,-3.14982373241352));
#59622=CARTESIAN_POINT('Ctrl Pts',(2.48150133566571,1.,-3.15709802322739));
#59623=CARTESIAN_POINT('Ctrl Pts',(2.48378981792725,1.,-3.16439213290161));
#59624=CARTESIAN_POINT('Ctrl Pts',(2.48604065348587,1.,-3.17170518863313));
#59625=CARTESIAN_POINT('Ctrl Pts',(2.48825428288201,1.,-3.17903698136622));
#59626=CARTESIAN_POINT('Ctrl Pts',(2.49043146334059,1.,-3.18638771282266));
#59627=CARTESIAN_POINT('Ctrl Pts',(2.49257307239848,1.,-3.19375775555798));
#59628=CARTESIAN_POINT('Ctrl Pts',(2.49467992057755,1.,-3.20114742397588));
#59629=CARTESIAN_POINT('Ctrl Pts',(2.4967525264737,1.,-3.20855669849836));
#59630=CARTESIAN_POINT('Ctrl Pts',(2.4987911459939,1.,-3.21598526261286));
#59631=CARTESIAN_POINT('Ctrl Pts',(2.50079587201957,1.,-3.22343262620503));
#59632=CARTESIAN_POINT('Ctrl Pts',(2.50276671338111,1.,-3.23089822320646));
#59633=CARTESIAN_POINT('Ctrl Pts',(2.5047036758003,1.,-3.23838151080319));
#59634=CARTESIAN_POINT('Ctrl Pts',(2.506606859405,1.,-3.24588208983849));
#59635=CARTESIAN_POINT('Ctrl Pts',(2.50847647070723,1.,-3.25339971460982));
#59636=CARTESIAN_POINT('Ctrl Pts',(2.51031277813486,1.,-3.26093423001434));
#59637=CARTESIAN_POINT('Ctrl Pts',(2.51211608411423,1.,-3.26848552888116));
#59638=CARTESIAN_POINT('Ctrl Pts',(2.513886692704,1.,-3.27605350473142));
#59639=CARTESIAN_POINT('Ctrl Pts',(2.51562487464514,1.,-3.28363799702982));
#59640=CARTESIAN_POINT('Ctrl Pts',(2.51733085123797,1.,-3.2912387729927));
#59641=CARTESIAN_POINT('Ctrl Pts',(2.51900480701068,1.,-3.29885556388353));
#59642=CARTESIAN_POINT('Ctrl Pts',(2.52064689568511,1.,-3.30648808815443));
#59643=CARTESIAN_POINT('Ctrl Pts',(2.52225724871313,1.,-3.31413607874645));
#59644=CARTESIAN_POINT('Ctrl Pts',(2.5238359839626,1.,-3.32179931078699));
#59645=CARTESIAN_POINT('Ctrl Pts',(2.52538321164634,1.,-3.32947762187533));
#59646=CARTESIAN_POINT('Ctrl Pts',(2.52689902690158,1.,-3.33717089999103));
#59647=CARTESIAN_POINT('Ctrl Pts',(2.52808660915689,1.,-3.34333744115511));
#59648=CARTESIAN_POINT('Ctrl Pts',(2.52896321610703,1.,-3.34796903576663));
#59649=CARTESIAN_POINT('Ctrl Pts',(2.5295413654909,1.,-3.35105973714072));
#59650=CARTESIAN_POINT('Ctrl Pts',(2.52982887637028,1.,-3.35260583073571));
#59651=CARTESIAN_POINT('Origin',(2.52982887637028,0.,-3.35260583073571));
#59652=CARTESIAN_POINT('',(2.40675750623143,1.,-3.44202241512147));
#59653=CARTESIAN_POINT('Origin',(0.,0.,0.));
#59654=CARTESIAN_POINT('',(2.50410331873042,1.,-2.79140942341378));
#59655=CARTESIAN_POINT('Origin',(0.,1.,0.));
#59656=CARTESIAN_POINT('Ctrl Pts',(2.50410331873042,1.,-2.79140942341378));
#59657=CARTESIAN_POINT('Ctrl Pts',(2.50410331873042,0.666666666666667,-2.79140942341378));
#59658=CARTESIAN_POINT('Ctrl Pts',(2.50410331873042,0.333333333333333,-2.79140942341378));
#59659=CARTESIAN_POINT('Ctrl Pts',(2.50410331873042,-0.333333333333333,
-2.79140942341378));
#59660=CARTESIAN_POINT('Ctrl Pts',(2.50410331873042,-0.666666666666667,
-2.79140942341378));
#59661=CARTESIAN_POINT('Ctrl Pts',(2.50410331873042,-1.,-2.79140942341378));
#59662=CARTESIAN_POINT('Ctrl Pts',(2.91557726271063,-1.,-3.02314558451372));
#59663=CARTESIAN_POINT('Ctrl Pts',(2.91557726271063,1.,-3.02314558451372));
#59664=CARTESIAN_POINT('Ctrl Pts',(2.91409518070707,-1.,-3.02261975104912));
#59665=CARTESIAN_POINT('Ctrl Pts',(2.91409518070707,1.,-3.02261975104912));
#59666=CARTESIAN_POINT('Ctrl Pts',(2.91113297349052,-1.,-3.02156522743299));
#59667=CARTESIAN_POINT('Ctrl Pts',(2.91113297349052,1.,-3.02156522743299));
#59668=CARTESIAN_POINT('Ctrl Pts',(2.90669553303902,-1.,-3.01997487194926));
#59669=CARTESIAN_POINT('Ctrl Pts',(2.90669553303902,1.,-3.01997487194926));
#59670=CARTESIAN_POINT('Ctrl Pts',(2.90079069102661,-1.,-3.01783725123646));
#59671=CARTESIAN_POINT('Ctrl Pts',(2.90079069102661,1.,-3.01783725123646));
#59672=CARTESIAN_POINT('Ctrl Pts',(2.8934292556764,-1.,-3.01513660433291));
#59673=CARTESIAN_POINT('Ctrl Pts',(2.8934292556764,1.,-3.01513660433291));
#59674=CARTESIAN_POINT('Ctrl Pts',(2.88608751706796,-1.,-3.01240727309568));
#59675=CARTESIAN_POINT('Ctrl Pts',(2.88608751706796,1.,-3.01240727309568));
#59676=CARTESIAN_POINT('Ctrl Pts',(2.87876560072799,-1.,-3.0096491810855));
#59677=CARTESIAN_POINT('Ctrl Pts',(2.87876560072799,1.,-3.0096491810855));
#59678=CARTESIAN_POINT('Ctrl Pts',(2.87146368430104,-1.,-3.00686224485374));
#59679=CARTESIAN_POINT('Ctrl Pts',(2.87146368430104,1.,-3.00686224485374));
#59680=CARTESIAN_POINT('Ctrl Pts',(2.86418200833065,-1.,-3.00404638316245));
#59681=CARTESIAN_POINT('Ctrl Pts',(2.86418200833065,1.,-3.00404638316245));
#59682=CARTESIAN_POINT('Ctrl Pts',(2.85692085715129,-1.,-3.0012015079552));
#59683=CARTESIAN_POINT('Ctrl Pts',(2.85692085715129,1.,-3.0012015079552));
#59684=CARTESIAN_POINT('Ctrl Pts',(2.84968053289104,-1.,-2.99832751144566));
#59685=CARTESIAN_POINT('Ctrl Pts',(2.84968053289104,1.,-2.99832751144566));
#59686=CARTESIAN_POINT('Ctrl Pts',(2.84246132984334,-1.,-2.995424253416));
#59687=CARTESIAN_POINT('Ctrl Pts',(2.84246132984334,1.,-2.995424253416));
#59688=CARTESIAN_POINT('Ctrl Pts',(2.83526351254383,-1.,-2.99249155170479));
#59689=CARTESIAN_POINT('Ctrl Pts',(2.83526351254383,1.,-2.99249155170479));
#59690=CARTESIAN_POINT('Ctrl Pts',(2.82808728190402,-1.,-2.98952916401699));
#59691=CARTESIAN_POINT('Ctrl Pts',(2.82808728190402,1.,-2.98952916401699));
#59692=CARTESIAN_POINT('Ctrl Pts',(2.82093279065704,-1.,-2.98653680669434));
#59693=CARTESIAN_POINT('Ctrl Pts',(2.82093279065704,1.,-2.98653680669434));
#59694=CARTESIAN_POINT('Ctrl Pts',(2.81380019196454,-1.,-2.9835141977994));
#59695=CARTESIAN_POINT('Ctrl Pts',(2.81380019196454,1.,-2.9835141977994));
#59696=CARTESIAN_POINT('Ctrl Pts',(2.80668968101162,-1.,-2.98046109647299));
#59697=CARTESIAN_POINT('Ctrl Pts',(2.80668968101162,1.,-2.98046109647299));
#59698=CARTESIAN_POINT('Ctrl Pts',(2.79960153278186,-1.,-2.97737733718242));
#59699=CARTESIAN_POINT('Ctrl Pts',(2.79960153278186,1.,-2.97737733718242));
#59700=CARTESIAN_POINT('Ctrl Pts',(2.79253615718147,-1.,-2.97426288347475));
#59701=CARTESIAN_POINT('Ctrl Pts',(2.79253615718147,1.,-2.97426288347475));
#59702=CARTESIAN_POINT('Ctrl Pts',(2.78549409123657,-1.,-2.97111781461349));
#59703=CARTESIAN_POINT('Ctrl Pts',(2.78549409123657,1.,-2.97111781461349));
#59704=CARTESIAN_POINT('Ctrl Pts',(2.77847589542767,-1.,-2.9679422104295));
#59705=CARTESIAN_POINT('Ctrl Pts',(2.77847589542767,1.,-2.9679422104295));
#59706=CARTESIAN_POINT('Ctrl Pts',(2.77148206836464,-1.,-2.96473605585548));
#59707=CARTESIAN_POINT('Ctrl Pts',(2.77148206836464,1.,-2.96473605585548));
#59708=CARTESIAN_POINT('Ctrl Pts',(2.76451296269571,-1.,-2.96149914764832));
#59709=CARTESIAN_POINT('Ctrl Pts',(2.76451296269571,1.,-2.96149914764832));
#59710=CARTESIAN_POINT('Ctrl Pts',(2.75756867888393,-1.,-2.9582309766594));
#59711=CARTESIAN_POINT('Ctrl Pts',(2.75756867888393,1.,-2.9582309766594));
#59712=CARTESIAN_POINT('Ctrl Pts',(2.75064903318996,-1.,-2.95493069316211));
#59713=CARTESIAN_POINT('Ctrl Pts',(2.75064903318996,1.,-2.95493069316211));
#59714=CARTESIAN_POINT('Ctrl Pts',(2.7437537949221,-1.,-2.95159737214305));
#59715=CARTESIAN_POINT('Ctrl Pts',(2.7437537949221,1.,-2.95159737214305));
#59716=CARTESIAN_POINT('Ctrl Pts',(2.73688288329825,-1.,-2.94823023414381));
#59717=CARTESIAN_POINT('Ctrl Pts',(2.73688288329825,1.,-2.94823023414381));
#59718=CARTESIAN_POINT('Ctrl Pts',(2.73003657371613,-1.,-2.94482887675139));
#59719=CARTESIAN_POINT('Ctrl Pts',(2.73003657371613,1.,-2.94482887675139));
#59720=CARTESIAN_POINT('Ctrl Pts',(2.72321571511322,-1.,-2.94139351933882));
#59721=CARTESIAN_POINT('Ctrl Pts',(2.72321571511322,1.,-2.94139351933882));
#59722=CARTESIAN_POINT('Ctrl Pts',(2.71642190053575,-1.,-2.93792519474955));
#59723=CARTESIAN_POINT('Ctrl Pts',(2.71642190053575,1.,-2.93792519474955));
#59724=CARTESIAN_POINT('Ctrl Pts',(2.70965695523776,-1.,-2.93442516311168));
#59725=CARTESIAN_POINT('Ctrl Pts',(2.70965695523776,1.,-2.93442516311168));
#59726=CARTESIAN_POINT('Ctrl Pts',(2.70292247416881,-1.,-2.93089438233746));
#59727=CARTESIAN_POINT('Ctrl Pts',(2.70292247416881,1.,-2.93089438233746));
#59728=CARTESIAN_POINT('Ctrl Pts',(2.69621932864302,-1.,-2.92733294395268));
#59729=CARTESIAN_POINT('Ctrl Pts',(2.69621932864302,1.,-2.92733294395268));
#59730=CARTESIAN_POINT('Ctrl Pts',(2.68954721165342,-1.,-2.92373955325876));
#59731=CARTESIAN_POINT('Ctrl Pts',(2.68954721165342,1.,-2.92373955325876));
#59732=CARTESIAN_POINT('Ctrl Pts',(2.68290409279689,-1.,-2.92011090722152));
#59733=CARTESIAN_POINT('Ctrl Pts',(2.68290409279689,1.,-2.92011090722152));
#59734=CARTESIAN_POINT('Ctrl Pts',(2.67628728855309,-1.,-2.91644290704281));
#59735=CARTESIAN_POINT('Ctrl Pts',(2.67628728855309,1.,-2.91644290704281));
#59736=CARTESIAN_POINT('Ctrl Pts',(2.66969458792627,-1.,-2.91273193382876));
#59737=CARTESIAN_POINT('Ctrl Pts',(2.66969458792627,1.,-2.91273193382876));
#59738=CARTESIAN_POINT('Ctrl Pts',(2.66312542616808,-1.,-2.90897617968921));
#59739=CARTESIAN_POINT('Ctrl Pts',(2.66312542616808,1.,-2.90897617968921));
#59740=CARTESIAN_POINT('Ctrl Pts',(2.65658188464287,-1.,-2.90517678087467));
#59741=CARTESIAN_POINT('Ctrl Pts',(2.65658188464287,1.,-2.90517678087467));
#59742=CARTESIAN_POINT('Ctrl Pts',(2.65007017365576,-1.,-2.90133950224879));
#59743=CARTESIAN_POINT('Ctrl Pts',(2.65007017365576,1.,-2.90133950224879));
#59744=CARTESIAN_POINT('Ctrl Pts',(2.64359851684146,-1.,-2.89747231723361));
#59745=CARTESIAN_POINT('Ctrl Pts',(2.64359851684146,1.,-2.89747231723361));
#59746=CARTESIAN_POINT('Ctrl Pts',(2.63717442263944,-1.,-2.89358228854557));
#59747=CARTESIAN_POINT('Ctrl Pts',(2.63717442263944,1.,-2.89358228854557));
#59748=CARTESIAN_POINT('Ctrl Pts',(2.63080195420771,-1.,-2.88967244854243));
#59749=CARTESIAN_POINT('Ctrl Pts',(2.63080195420771,1.,-2.88967244854243));
#59750=CARTESIAN_POINT('Ctrl Pts',(2.62447947640253,-1.,-2.88573922195049));
#59751=CARTESIAN_POINT('Ctrl Pts',(2.62447947640253,1.,-2.88573922195049));
#59752=CARTESIAN_POINT('Ctrl Pts',(2.61819596473087,-1.,-2.88176821427502));
#59753=CARTESIAN_POINT('Ctrl Pts',(2.61819596473087,1.,-2.88176821427502));
#59754=CARTESIAN_POINT('Ctrl Pts',(2.61193507170928,-1.,-2.87773881947885));
#59755=CARTESIAN_POINT('Ctrl Pts',(2.61193507170928,1.,-2.87773881947885));
#59756=CARTESIAN_POINT('Ctrl Pts',(2.6056817788128,-1.,-2.87363176656475));
#59757=CARTESIAN_POINT('Ctrl Pts',(2.6056817788128,1.,-2.87363176656475));
#59758=CARTESIAN_POINT('Ctrl Pts',(2.59942875223202,-1.,-2.86943633170712));
#59759=CARTESIAN_POINT('Ctrl Pts',(2.59942875223202,1.,-2.86943633170712));
#59760=CARTESIAN_POINT('Ctrl Pts',(2.59318160184921,-1.,-2.86515629953528));
#59761=CARTESIAN_POINT('Ctrl Pts',(2.59318160184921,1.,-2.86515629953528));
#59762=CARTESIAN_POINT('Ctrl Pts',(2.5869677064356,-1.,-2.86081999003668));
#59763=CARTESIAN_POINT('Ctrl Pts',(2.5869677064356,1.,-2.86081999003668));
#59764=CARTESIAN_POINT('Ctrl Pts',(2.58082875254407,-1.,-2.85647171715147));
#59765=CARTESIAN_POINT('Ctrl Pts',(2.58082875254407,1.,-2.85647171715147));
#59766=CARTESIAN_POINT('Ctrl Pts',(2.57480482727128,-1.,-2.85215360144483));
#59767=CARTESIAN_POINT('Ctrl Pts',(2.57480482727128,1.,-2.85215360144483));
#59768=CARTESIAN_POINT('Ctrl Pts',(2.56891984251743,-1.,-2.84788893329091));
#59769=CARTESIAN_POINT('Ctrl Pts',(2.56891984251743,1.,-2.84788893329091));
#59770=CARTESIAN_POINT('Ctrl Pts',(2.56316920798489,-1.,-2.84366802680211));
#59771=CARTESIAN_POINT('Ctrl Pts',(2.56316920798489,1.,-2.84366802680211));
#59772=CARTESIAN_POINT('Ctrl Pts',(2.55749952145165,-1.,-2.83942515220699));
#59773=CARTESIAN_POINT('Ctrl Pts',(2.55749952145165,1.,-2.83942515220699));
#59774=CARTESIAN_POINT('Ctrl Pts',(2.55182152806964,-1.,-2.83505269592412));
#59775=CARTESIAN_POINT('Ctrl Pts',(2.55182152806964,1.,-2.83505269592412));
#59776=CARTESIAN_POINT('Ctrl Pts',(2.54604736792542,-1.,-2.83044254225794));
#59777=CARTESIAN_POINT('Ctrl Pts',(2.54604736792542,1.,-2.83044254225794));
#59778=CARTESIAN_POINT('Ctrl Pts',(2.54012272520141,-1.,-2.82552167649157));
#59779=CARTESIAN_POINT('Ctrl Pts',(2.54012272520141,1.,-2.82552167649157));
#59780=CARTESIAN_POINT('Ctrl Pts',(2.53405679667463,-1.,-2.82028550483744));
#59781=CARTESIAN_POINT('Ctrl Pts',(2.53405679667463,1.,-2.82028550483744));
#59782=CARTESIAN_POINT('Ctrl Pts',(2.52796388055457,-1.,-2.8148437904867));
#59783=CARTESIAN_POINT('Ctrl Pts',(2.52796388055457,1.,-2.8148437904867));
#59784=CARTESIAN_POINT('Ctrl Pts',(2.52205778589922,-1.,-2.80941521967234));
#59785=CARTESIAN_POINT('Ctrl Pts',(2.52205778589922,1.,-2.80941521967234));
#59786=CARTESIAN_POINT('Ctrl Pts',(2.51660190466067,-1.,-2.80427363984939));
#59787=CARTESIAN_POINT('Ctrl Pts',(2.51660190466067,1.,-2.80427363984939));
#59788=CARTESIAN_POINT('Ctrl Pts',(2.51186983687947,-1.,-2.79970585014308));
#59789=CARTESIAN_POINT('Ctrl Pts',(2.51186983687947,1.,-2.79970585014308));
#59790=CARTESIAN_POINT('Ctrl Pts',(2.50810555977564,-1.,-2.7959687805717));
#59791=CARTESIAN_POINT('Ctrl Pts',(2.50810555977564,1.,-2.7959687805717));
#59792=CARTESIAN_POINT('Ctrl Pts',(2.50547439929077,-1.,-2.79323694088143));
#59793=CARTESIAN_POINT('Ctrl Pts',(2.50547439929077,1.,-2.79323694088143));
#59794=CARTESIAN_POINT('Ctrl Pts',(2.50433799076945,-1.,-2.79192122906739));
#59795=CARTESIAN_POINT('Ctrl Pts',(2.50433799076945,1.,-2.79192122906739));
#59796=CARTESIAN_POINT('Ctrl Pts',(2.50404230339032,-1.,-2.79143626022225));
#59797=CARTESIAN_POINT('Ctrl Pts',(2.50404230339032,1.,-2.79143626022225));
#59798=CARTESIAN_POINT('Ctrl Pts',(2.50409239460011,-1.,-2.79133581100044));
#59799=CARTESIAN_POINT('Ctrl Pts',(2.50409239460011,1.,-2.79133581100044));
#59800=CARTESIAN_POINT('Ctrl Pts',(2.50417924854921,-1.,-2.79134130681569));
#59801=CARTESIAN_POINT('Ctrl Pts',(2.50417924854921,1.,-2.79134130681569));
#59802=CARTESIAN_POINT('',(2.91557726271063,1.,-3.02314558451372));
#59803=CARTESIAN_POINT('Ctrl Pts',(2.91557726271063,1.,-3.02314558451372));
#59804=CARTESIAN_POINT('Ctrl Pts',(2.91409518070707,1.,-3.02261975104912));
#59805=CARTESIAN_POINT('Ctrl Pts',(2.91113297349052,1.,-3.02156522743299));
#59806=CARTESIAN_POINT('Ctrl Pts',(2.90669553303902,1.,-3.01997487194926));
#59807=CARTESIAN_POINT('Ctrl Pts',(2.90079069102661,1.,-3.01783725123646));
#59808=CARTESIAN_POINT('Ctrl Pts',(2.8934292556764,1.,-3.01513660433291));
#59809=CARTESIAN_POINT('Ctrl Pts',(2.88608751706796,1.,-3.01240727309568));
#59810=CARTESIAN_POINT('Ctrl Pts',(2.87876560072799,1.,-3.0096491810855));
#59811=CARTESIAN_POINT('Ctrl Pts',(2.87146368430104,1.,-3.00686224485374));
#59812=CARTESIAN_POINT('Ctrl Pts',(2.86418200833065,1.,-3.00404638316245));
#59813=CARTESIAN_POINT('Ctrl Pts',(2.85692085715129,1.,-3.0012015079552));
#59814=CARTESIAN_POINT('Ctrl Pts',(2.84968053289104,1.,-2.99832751144566));
#59815=CARTESIAN_POINT('Ctrl Pts',(2.84246132984334,1.,-2.995424253416));
#59816=CARTESIAN_POINT('Ctrl Pts',(2.83526351254383,1.,-2.99249155170479));
#59817=CARTESIAN_POINT('Ctrl Pts',(2.82808728190402,1.,-2.98952916401699));
#59818=CARTESIAN_POINT('Ctrl Pts',(2.82093279065704,1.,-2.98653680669434));
#59819=CARTESIAN_POINT('Ctrl Pts',(2.81380019196454,1.,-2.9835141977994));
#59820=CARTESIAN_POINT('Ctrl Pts',(2.80668968101162,1.,-2.98046109647299));
#59821=CARTESIAN_POINT('Ctrl Pts',(2.79960153278186,1.,-2.97737733718242));
#59822=CARTESIAN_POINT('Ctrl Pts',(2.79253615718147,1.,-2.97426288347475));
#59823=CARTESIAN_POINT('Ctrl Pts',(2.78549409123657,1.,-2.97111781461349));
#59824=CARTESIAN_POINT('Ctrl Pts',(2.77847589542767,1.,-2.9679422104295));
#59825=CARTESIAN_POINT('Ctrl Pts',(2.77148206836464,1.,-2.96473605585548));
#59826=CARTESIAN_POINT('Ctrl Pts',(2.76451296269571,1.,-2.96149914764832));
#59827=CARTESIAN_POINT('Ctrl Pts',(2.75756867888393,1.,-2.9582309766594));
#59828=CARTESIAN_POINT('Ctrl Pts',(2.75064903318996,1.,-2.95493069316211));
#59829=CARTESIAN_POINT('Ctrl Pts',(2.7437537949221,1.,-2.95159737214305));
#59830=CARTESIAN_POINT('Ctrl Pts',(2.73688288329825,1.,-2.94823023414381));
#59831=CARTESIAN_POINT('Ctrl Pts',(2.73003657371613,1.,-2.94482887675139));
#59832=CARTESIAN_POINT('Ctrl Pts',(2.72321571511322,1.,-2.94139351933882));
#59833=CARTESIAN_POINT('Ctrl Pts',(2.71642190053575,1.,-2.93792519474955));
#59834=CARTESIAN_POINT('Ctrl Pts',(2.70965695523776,1.,-2.93442516311168));
#59835=CARTESIAN_POINT('Ctrl Pts',(2.70292247416881,1.,-2.93089438233746));
#59836=CARTESIAN_POINT('Ctrl Pts',(2.69621932864302,1.,-2.92733294395268));
#59837=CARTESIAN_POINT('Ctrl Pts',(2.68954721165342,1.,-2.92373955325876));
#59838=CARTESIAN_POINT('Ctrl Pts',(2.68290409279689,1.,-2.92011090722152));
#59839=CARTESIAN_POINT('Ctrl Pts',(2.67628728855309,1.,-2.91644290704281));
#59840=CARTESIAN_POINT('Ctrl Pts',(2.66969458792627,1.,-2.91273193382876));
#59841=CARTESIAN_POINT('Ctrl Pts',(2.66312542616808,1.,-2.90897617968921));
#59842=CARTESIAN_POINT('Ctrl Pts',(2.65658188464287,1.,-2.90517678087467));
#59843=CARTESIAN_POINT('Ctrl Pts',(2.65007017365576,1.,-2.90133950224879));
#59844=CARTESIAN_POINT('Ctrl Pts',(2.64359851684146,1.,-2.89747231723361));
#59845=CARTESIAN_POINT('Ctrl Pts',(2.63717442263944,1.,-2.89358228854557));
#59846=CARTESIAN_POINT('Ctrl Pts',(2.63080195420771,1.,-2.88967244854243));
#59847=CARTESIAN_POINT('Ctrl Pts',(2.62447947640253,1.,-2.88573922195049));
#59848=CARTESIAN_POINT('Ctrl Pts',(2.61819596473087,1.,-2.88176821427502));
#59849=CARTESIAN_POINT('Ctrl Pts',(2.61193507170928,1.,-2.87773881947885));
#59850=CARTESIAN_POINT('Ctrl Pts',(2.6056817788128,1.,-2.87363176656475));
#59851=CARTESIAN_POINT('Ctrl Pts',(2.59942875223202,1.,-2.86943633170712));
#59852=CARTESIAN_POINT('Ctrl Pts',(2.59318160184921,1.,-2.86515629953528));
#59853=CARTESIAN_POINT('Ctrl Pts',(2.5869677064356,1.,-2.86081999003668));
#59854=CARTESIAN_POINT('Ctrl Pts',(2.58082875254407,1.,-2.85647171715147));
#59855=CARTESIAN_POINT('Ctrl Pts',(2.57480482727128,1.,-2.85215360144483));
#59856=CARTESIAN_POINT('Ctrl Pts',(2.56891984251743,1.,-2.84788893329091));
#59857=CARTESIAN_POINT('Ctrl Pts',(2.56316920798489,1.,-2.84366802680211));
#59858=CARTESIAN_POINT('Ctrl Pts',(2.55749952145165,1.,-2.83942515220699));
#59859=CARTESIAN_POINT('Ctrl Pts',(2.55182152806964,1.,-2.83505269592412));
#59860=CARTESIAN_POINT('Ctrl Pts',(2.54604736792542,1.,-2.83044254225794));
#59861=CARTESIAN_POINT('Ctrl Pts',(2.54012272520141,1.,-2.82552167649157));
#59862=CARTESIAN_POINT('Ctrl Pts',(2.53405679667463,1.,-2.82028550483744));
#59863=CARTESIAN_POINT('Ctrl Pts',(2.52796388055457,1.,-2.8148437904867));
#59864=CARTESIAN_POINT('Ctrl Pts',(2.52205778589922,1.,-2.80941521967234));
#59865=CARTESIAN_POINT('Ctrl Pts',(2.51660190466067,1.,-2.80427363984939));
#59866=CARTESIAN_POINT('Ctrl Pts',(2.51186983687947,1.,-2.79970585014308));
#59867=CARTESIAN_POINT('Ctrl Pts',(2.50810555977564,1.,-2.7959687805717));
#59868=CARTESIAN_POINT('Ctrl Pts',(2.50567182569153,1.,-2.79344192164204));
#59869=CARTESIAN_POINT('Ctrl Pts',(2.50455968395235,1.,-2.79217568804874));
#59870=CARTESIAN_POINT('Ctrl Pts',(2.50417932839344,1.,-2.79164172519039));
#59871=CARTESIAN_POINT('Ctrl Pts',(2.50410700351427,1.,-2.79145823440899));
#59872=CARTESIAN_POINT('Ctrl Pts',(2.50410331873043,1.,-2.79140942341378));
#59873=CARTESIAN_POINT('',(2.91557726271063,0.,-3.02314558451372));
#59874=CARTESIAN_POINT('Ctrl Pts',(2.79134130681569,-1.,-2.50417924854921));
#59875=CARTESIAN_POINT('Ctrl Pts',(2.79134130681569,1.,-2.50417924854921));
#59876=CARTESIAN_POINT('Ctrl Pts',(2.7913358110015,-1.,-2.50409239460108));
#59877=CARTESIAN_POINT('Ctrl Pts',(2.7913358110015,1.,-2.50409239460108));
#59878=CARTESIAN_POINT('Ctrl Pts',(2.79143626022503,-1.,-2.50404230339286));
#59879=CARTESIAN_POINT('Ctrl Pts',(2.79143626022503,1.,-2.50404230339286));
#59880=CARTESIAN_POINT('Ctrl Pts',(2.79192122907148,-1.,-2.5043379907732));
#59881=CARTESIAN_POINT('Ctrl Pts',(2.79192122907148,1.,-2.5043379907732));
#59882=CARTESIAN_POINT('Ctrl Pts',(2.7932369408851,-1.,-2.50547439929414));
#59883=CARTESIAN_POINT('Ctrl Pts',(2.7932369408851,1.,-2.50547439929414));
#59884=CARTESIAN_POINT('Ctrl Pts',(2.79596878057287,-1.,-2.50810555977671));
#59885=CARTESIAN_POINT('Ctrl Pts',(2.79596878057287,1.,-2.50810555977671));
#59886=CARTESIAN_POINT('Ctrl Pts',(2.79970585014168,-1.,-2.51186983687818));
#59887=CARTESIAN_POINT('Ctrl Pts',(2.79970585014168,1.,-2.51186983687818));
#59888=CARTESIAN_POINT('Ctrl Pts',(2.80427363984653,-1.,-2.51660190465805));
#59889=CARTESIAN_POINT('Ctrl Pts',(2.80427363984653,1.,-2.51660190465805));
#59890=CARTESIAN_POINT('Ctrl Pts',(2.80941521966941,-1.,-2.52205778589653));
#59891=CARTESIAN_POINT('Ctrl Pts',(2.80941521966941,1.,-2.52205778589653));
#59892=CARTESIAN_POINT('Ctrl Pts',(2.81484379048475,-1.,-2.52796388055278));
#59893=CARTESIAN_POINT('Ctrl Pts',(2.81484379048475,1.,-2.52796388055278));
#59894=CARTESIAN_POINT('Ctrl Pts',(2.82028550483689,-1.,-2.53405679667412));
#59895=CARTESIAN_POINT('Ctrl Pts',(2.82028550483689,1.,-2.53405679667412));
#59896=CARTESIAN_POINT('Ctrl Pts',(2.8255216764922,-1.,-2.54012272520199));
#59897=CARTESIAN_POINT('Ctrl Pts',(2.8255216764922,1.,-2.54012272520199));
#59898=CARTESIAN_POINT('Ctrl Pts',(2.83044254225917,-1.,-2.54604736792655));
#59899=CARTESIAN_POINT('Ctrl Pts',(2.83044254225917,1.,-2.54604736792655));
#59900=CARTESIAN_POINT('Ctrl Pts',(2.83505269592536,-1.,-2.55182152807077));
#59901=CARTESIAN_POINT('Ctrl Pts',(2.83505269592536,1.,-2.55182152807077));
#59902=CARTESIAN_POINT('Ctrl Pts',(2.83942515220782,-1.,-2.55749952145241));
#59903=CARTESIAN_POINT('Ctrl Pts',(2.83942515220782,1.,-2.55749952145241));
#59904=CARTESIAN_POINT('Ctrl Pts',(2.84366802680237,-1.,-2.56316920798513));
#59905=CARTESIAN_POINT('Ctrl Pts',(2.84366802680237,1.,-2.56316920798513));
#59906=CARTESIAN_POINT('Ctrl Pts',(2.84788893329067,-1.,-2.56891984251721));
#59907=CARTESIAN_POINT('Ctrl Pts',(2.84788893329067,1.,-2.56891984251721));
#59908=CARTESIAN_POINT('Ctrl Pts',(2.85215360144431,-1.,-2.57480482727081));
#59909=CARTESIAN_POINT('Ctrl Pts',(2.85215360144431,1.,-2.57480482727081));
#59910=CARTESIAN_POINT('Ctrl Pts',(2.85647171715092,-1.,-2.58082875254357));
#59911=CARTESIAN_POINT('Ctrl Pts',(2.85647171715092,1.,-2.58082875254357));
#59912=CARTESIAN_POINT('Ctrl Pts',(2.86081999003629,-1.,-2.58696770643524));
#59913=CARTESIAN_POINT('Ctrl Pts',(2.86081999003629,1.,-2.58696770643524));
#59914=CARTESIAN_POINT('Ctrl Pts',(2.86515629953513,-1.,-2.59318160184908));
#59915=CARTESIAN_POINT('Ctrl Pts',(2.86515629953513,1.,-2.59318160184908));
#59916=CARTESIAN_POINT('Ctrl Pts',(2.86943633170722,-1.,-2.5994287522321));
#59917=CARTESIAN_POINT('Ctrl Pts',(2.86943633170722,1.,-2.5994287522321));
#59918=CARTESIAN_POINT('Ctrl Pts',(2.87363176656501,-1.,-2.60568177881303));
#59919=CARTESIAN_POINT('Ctrl Pts',(2.87363176656501,1.,-2.60568177881303));
#59920=CARTESIAN_POINT('Ctrl Pts',(2.87773881947915,-1.,-2.61193507170955));
#59921=CARTESIAN_POINT('Ctrl Pts',(2.87773881947915,1.,-2.61193507170955));
#59922=CARTESIAN_POINT('Ctrl Pts',(2.88176821427525,-1.,-2.61819596473108));
#59923=CARTESIAN_POINT('Ctrl Pts',(2.88176821427525,1.,-2.61819596473108));
#59924=CARTESIAN_POINT('Ctrl Pts',(2.88573922195059,-1.,-2.62447947640262));
#59925=CARTESIAN_POINT('Ctrl Pts',(2.88573922195059,1.,-2.62447947640262));
#59926=CARTESIAN_POINT('Ctrl Pts',(2.88967244854239,-1.,-2.63080195420767));
#59927=CARTESIAN_POINT('Ctrl Pts',(2.88967244854239,1.,-2.63080195420767));
#59928=CARTESIAN_POINT('Ctrl Pts',(2.89358228854544,-1.,-2.63717442263932));
#59929=CARTESIAN_POINT('Ctrl Pts',(2.89358228854544,1.,-2.63717442263932));
#59930=CARTESIAN_POINT('Ctrl Pts',(2.89747231723345,-1.,-2.64359851684131));
#59931=CARTESIAN_POINT('Ctrl Pts',(2.89747231723345,1.,-2.64359851684131));
#59932=CARTESIAN_POINT('Ctrl Pts',(2.90133950224867,-1.,-2.65007017365564));
#59933=CARTESIAN_POINT('Ctrl Pts',(2.90133950224867,1.,-2.65007017365564));
#59934=CARTESIAN_POINT('Ctrl Pts',(2.90517678087461,-1.,-2.65658188464282));
#59935=CARTESIAN_POINT('Ctrl Pts',(2.90517678087461,1.,-2.65658188464282));
#59936=CARTESIAN_POINT('Ctrl Pts',(2.90897617968923,-1.,-2.6631254261681));
#59937=CARTESIAN_POINT('Ctrl Pts',(2.90897617968923,1.,-2.6631254261681));
#59938=CARTESIAN_POINT('Ctrl Pts',(2.91273193382882,-1.,-2.66969458792631));
#59939=CARTESIAN_POINT('Ctrl Pts',(2.91273193382882,1.,-2.66969458792631));
#59940=CARTESIAN_POINT('Ctrl Pts',(2.91644290704285,-1.,-2.67628728855312));
#59941=CARTESIAN_POINT('Ctrl Pts',(2.91644290704285,1.,-2.67628728855312));
#59942=CARTESIAN_POINT('Ctrl Pts',(2.92011090722152,-1.,-2.68290409279688));
#59943=CARTESIAN_POINT('Ctrl Pts',(2.92011090722152,1.,-2.68290409279688));
#59944=CARTESIAN_POINT('Ctrl Pts',(2.92373955325875,-1.,-2.68954721165339));
#59945=CARTESIAN_POINT('Ctrl Pts',(2.92373955325875,1.,-2.68954721165339));
#59946=CARTESIAN_POINT('Ctrl Pts',(2.92733294395267,-1.,-2.69621932864301));
#59947=CARTESIAN_POINT('Ctrl Pts',(2.92733294395267,1.,-2.69621932864301));
#59948=CARTESIAN_POINT('Ctrl Pts',(2.93089438233749,-1.,-2.70292247416885));
#59949=CARTESIAN_POINT('Ctrl Pts',(2.93089438233749,1.,-2.70292247416885));
#59950=CARTESIAN_POINT('Ctrl Pts',(2.93442516311179,-1.,-2.70965695523787));
#59951=CARTESIAN_POINT('Ctrl Pts',(2.93442516311179,1.,-2.70965695523787));
#59952=CARTESIAN_POINT('Ctrl Pts',(2.93792519474972,-1.,-2.71642190053592));
#59953=CARTESIAN_POINT('Ctrl Pts',(2.93792519474972,1.,-2.71642190053592));
#59954=CARTESIAN_POINT('Ctrl Pts',(2.94139351933897,-1.,-2.72321571511337));
#59955=CARTESIAN_POINT('Ctrl Pts',(2.94139351933897,1.,-2.72321571511337));
#59956=CARTESIAN_POINT('Ctrl Pts',(2.94482887675143,-1.,-2.73003657371617));
#59957=CARTESIAN_POINT('Ctrl Pts',(2.94482887675143,1.,-2.73003657371617));
#59958=CARTESIAN_POINT('Ctrl Pts',(2.94823023414364,-1.,-2.73688288329808));
#59959=CARTESIAN_POINT('Ctrl Pts',(2.94823023414364,1.,-2.73688288329808));
#59960=CARTESIAN_POINT('Ctrl Pts',(2.95159737214266,-1.,-2.74375379492172));
#59961=CARTESIAN_POINT('Ctrl Pts',(2.95159737214266,1.,-2.74375379492172));
#59962=CARTESIAN_POINT('Ctrl Pts',(2.95493069316161,-1.,-2.75064903318947));
#59963=CARTESIAN_POINT('Ctrl Pts',(2.95493069316161,1.,-2.75064903318947));
#59964=CARTESIAN_POINT('Ctrl Pts',(2.95823097665896,-1.,-2.7575686788835));
#59965=CARTESIAN_POINT('Ctrl Pts',(2.95823097665896,1.,-2.7575686788835));
#59966=CARTESIAN_POINT('Ctrl Pts',(2.96149914764818,-1.,-2.76451296269557));
#59967=CARTESIAN_POINT('Ctrl Pts',(2.96149914764818,1.,-2.76451296269557));
#59968=CARTESIAN_POINT('Ctrl Pts',(2.96473605585583,-1.,-2.77148206836498));
#59969=CARTESIAN_POINT('Ctrl Pts',(2.96473605585583,1.,-2.77148206836498));
#59970=CARTESIAN_POINT('Ctrl Pts',(2.96794221043036,-1.,-2.7784758954285));
#59971=CARTESIAN_POINT('Ctrl Pts',(2.96794221043036,1.,-2.7784758954285));
#59972=CARTESIAN_POINT('Ctrl Pts',(2.97111781461465,-1.,-2.78549409123769));
#59973=CARTESIAN_POINT('Ctrl Pts',(2.97111781461465,1.,-2.78549409123769));
#59974=CARTESIAN_POINT('Ctrl Pts',(2.9742628834758,-1.,-2.79253615718248));
#59975=CARTESIAN_POINT('Ctrl Pts',(2.9742628834758,1.,-2.79253615718248));
#59976=CARTESIAN_POINT('Ctrl Pts',(2.97737733718287,-1.,-2.7996015327823));
#59977=CARTESIAN_POINT('Ctrl Pts',(2.97737733718287,1.,-2.7996015327823));
#59978=CARTESIAN_POINT('Ctrl Pts',(2.98046109647241,-1.,-2.80668968101106));
#59979=CARTESIAN_POINT('Ctrl Pts',(2.98046109647241,1.,-2.80668968101106));
#59980=CARTESIAN_POINT('Ctrl Pts',(2.98351419779767,-1.,-2.81380019196286));
#59981=CARTESIAN_POINT('Ctrl Pts',(2.98351419779767,1.,-2.81380019196286));
#59982=CARTESIAN_POINT('Ctrl Pts',(2.9865368066918,-1.,-2.82093279065457));
#59983=CARTESIAN_POINT('Ctrl Pts',(2.9865368066918,1.,-2.82093279065457));
#59984=CARTESIAN_POINT('Ctrl Pts',(2.98952916401446,-1.,-2.82808728190157));
#59985=CARTESIAN_POINT('Ctrl Pts',(2.98952916401446,1.,-2.82808728190157));
#59986=CARTESIAN_POINT('Ctrl Pts',(2.99249155170339,-1.,-2.83526351254248));
#59987=CARTESIAN_POINT('Ctrl Pts',(2.99249155170339,1.,-2.83526351254248));
#59988=CARTESIAN_POINT('Ctrl Pts',(2.99542425341685,-1.,-2.84246132984415));
#59989=CARTESIAN_POINT('Ctrl Pts',(2.99542425341685,1.,-2.84246132984415));
#59990=CARTESIAN_POINT('Ctrl Pts',(2.99832751144925,-1.,-2.84968053289451));
#59991=CARTESIAN_POINT('Ctrl Pts',(2.99832751144925,1.,-2.84968053289451));
#59992=CARTESIAN_POINT('Ctrl Pts',(3.00120150796095,-1.,-2.85692085715686));
#59993=CARTESIAN_POINT('Ctrl Pts',(3.00120150796095,1.,-2.85692085715686));
#59994=CARTESIAN_POINT('Ctrl Pts',(3.00404638316867,-1.,-2.86418200833667));
#59995=CARTESIAN_POINT('Ctrl Pts',(3.00404638316867,1.,-2.86418200833667));
#59996=CARTESIAN_POINT('Ctrl Pts',(3.00686224485784,-1.,-2.87146368430502));
#59997=CARTESIAN_POINT('Ctrl Pts',(3.00686224485784,1.,-2.87146368430502));
#59998=CARTESIAN_POINT('Ctrl Pts',(3.00964918108476,-1.,-2.87876560072727));
#59999=CARTESIAN_POINT('Ctrl Pts',(3.00964918108476,1.,-2.87876560072727));
#60000=CARTESIAN_POINT('Ctrl Pts',(3.01240727308829,-1.,-2.8860875170608));
#60001=CARTESIAN_POINT('Ctrl Pts',(3.01240727308829,1.,-2.8860875170608));
#60002=CARTESIAN_POINT('Ctrl Pts',(3.01513660431928,-1.,-2.89342925566321));
#60003=CARTESIAN_POINT('Ctrl Pts',(3.01513660431928,1.,-2.89342925566321));
#60004=CARTESIAN_POINT('Ctrl Pts',(3.01783725121981,-1.,-2.9007906910105));
#60005=CARTESIAN_POINT('Ctrl Pts',(3.01783725121981,1.,-2.9007906910105));
#60006=CARTESIAN_POINT('Ctrl Pts',(3.01997487193503,-1.,-2.90669553302526));
#60007=CARTESIAN_POINT('Ctrl Pts',(3.01997487193503,1.,-2.90669553302526));
#60008=CARTESIAN_POINT('Ctrl Pts',(3.02156522742431,-1.,-2.91113297348212));
#60009=CARTESIAN_POINT('Ctrl Pts',(3.02156522742431,1.,-2.91113297348212));
#60010=CARTESIAN_POINT('Ctrl Pts',(3.02261975104593,-1.,-2.91409518070399));
#60011=CARTESIAN_POINT('Ctrl Pts',(3.02261975104593,1.,-2.91409518070399));
#60012=CARTESIAN_POINT('Ctrl Pts',(3.02314558451372,-1.,-2.91557726271063));
#60013=CARTESIAN_POINT('Ctrl Pts',(3.02314558451372,1.,-2.91557726271063));
#60014=CARTESIAN_POINT('',(2.79140942341258,1.,-2.50410331873176));
#60015=CARTESIAN_POINT('Ctrl Pts',(2.79140942341258,-1.,-2.50410331873176));
#60016=CARTESIAN_POINT('Ctrl Pts',(2.79140942341258,-0.666666666666667,
-2.50410331873176));
#60017=CARTESIAN_POINT('Ctrl Pts',(2.79140942341258,-0.333333333333333,
-2.50410331873176));
#60018=CARTESIAN_POINT('Ctrl Pts',(2.79140942341258,0.333333333333333,-2.50410331873176));
#60019=CARTESIAN_POINT('Ctrl Pts',(2.79140942341258,0.666666666666667,-2.50410331873176));
#60020=CARTESIAN_POINT('Ctrl Pts',(2.79140942341258,1.,-2.50410331873176));
#60021=CARTESIAN_POINT('',(3.02314558451372,1.,-2.91557726271063));
#60022=CARTESIAN_POINT('',(3.02314558451372,0.,-2.91557726271063));
#60023=CARTESIAN_POINT('Ctrl Pts',(2.79140942341258,1.,-2.50410331873176));
#60024=CARTESIAN_POINT('Ctrl Pts',(2.79145823440781,1.,-2.50410700351493));
#60025=CARTESIAN_POINT('Ctrl Pts',(2.79164172518905,1.,-2.50417932839313));
#60026=CARTESIAN_POINT('Ctrl Pts',(2.79217568804755,1.,-2.50455968395146));
#60027=CARTESIAN_POINT('Ctrl Pts',(2.79344192164147,1.,-2.50567182569081));
#60028=CARTESIAN_POINT('Ctrl Pts',(2.79596878057287,1.,-2.50810555977671));
#60029=CARTESIAN_POINT('Ctrl Pts',(2.79970585014168,1.,-2.51186983687818));
#60030=CARTESIAN_POINT('Ctrl Pts',(2.80427363984653,1.,-2.51660190465805));
#60031=CARTESIAN_POINT('Ctrl Pts',(2.80941521966941,1.,-2.52205778589653));
#60032=CARTESIAN_POINT('Ctrl Pts',(2.81484379048475,1.,-2.52796388055278));
#60033=CARTESIAN_POINT('Ctrl Pts',(2.82028550483689,1.,-2.53405679667412));
#60034=CARTESIAN_POINT('Ctrl Pts',(2.8255216764922,1.,-2.54012272520199));
#60035=CARTESIAN_POINT('Ctrl Pts',(2.83044254225917,1.,-2.54604736792655));
#60036=CARTESIAN_POINT('Ctrl Pts',(2.83505269592536,1.,-2.55182152807077));
#60037=CARTESIAN_POINT('Ctrl Pts',(2.83942515220782,1.,-2.55749952145241));
#60038=CARTESIAN_POINT('Ctrl Pts',(2.84366802680237,1.,-2.56316920798513));
#60039=CARTESIAN_POINT('Ctrl Pts',(2.84788893329067,1.,-2.56891984251721));
#60040=CARTESIAN_POINT('Ctrl Pts',(2.85215360144431,1.,-2.57480482727081));
#60041=CARTESIAN_POINT('Ctrl Pts',(2.85647171715092,1.,-2.58082875254357));
#60042=CARTESIAN_POINT('Ctrl Pts',(2.86081999003629,1.,-2.58696770643524));
#60043=CARTESIAN_POINT('Ctrl Pts',(2.86515629953513,1.,-2.59318160184908));
#60044=CARTESIAN_POINT('Ctrl Pts',(2.86943633170722,1.,-2.5994287522321));
#60045=CARTESIAN_POINT('Ctrl Pts',(2.87363176656501,1.,-2.60568177881303));
#60046=CARTESIAN_POINT('Ctrl Pts',(2.87773881947915,1.,-2.61193507170955));
#60047=CARTESIAN_POINT('Ctrl Pts',(2.88176821427525,1.,-2.61819596473108));
#60048=CARTESIAN_POINT('Ctrl Pts',(2.88573922195059,1.,-2.62447947640262));
#60049=CARTESIAN_POINT('Ctrl Pts',(2.88967244854239,1.,-2.63080195420767));
#60050=CARTESIAN_POINT('Ctrl Pts',(2.89358228854544,1.,-2.63717442263932));
#60051=CARTESIAN_POINT('Ctrl Pts',(2.89747231723345,1.,-2.64359851684131));
#60052=CARTESIAN_POINT('Ctrl Pts',(2.90133950224867,1.,-2.65007017365564));
#60053=CARTESIAN_POINT('Ctrl Pts',(2.90517678087461,1.,-2.65658188464282));
#60054=CARTESIAN_POINT('Ctrl Pts',(2.90897617968923,1.,-2.6631254261681));
#60055=CARTESIAN_POINT('Ctrl Pts',(2.91273193382882,1.,-2.66969458792631));
#60056=CARTESIAN_POINT('Ctrl Pts',(2.91644290704285,1.,-2.67628728855312));
#60057=CARTESIAN_POINT('Ctrl Pts',(2.92011090722152,1.,-2.68290409279688));
#60058=CARTESIAN_POINT('Ctrl Pts',(2.92373955325875,1.,-2.68954721165339));
#60059=CARTESIAN_POINT('Ctrl Pts',(2.92733294395267,1.,-2.69621932864301));
#60060=CARTESIAN_POINT('Ctrl Pts',(2.93089438233749,1.,-2.70292247416885));
#60061=CARTESIAN_POINT('Ctrl Pts',(2.93442516311179,1.,-2.70965695523787));
#60062=CARTESIAN_POINT('Ctrl Pts',(2.93792519474972,1.,-2.71642190053592));
#60063=CARTESIAN_POINT('Ctrl Pts',(2.94139351933897,1.,-2.72321571511337));
#60064=CARTESIAN_POINT('Ctrl Pts',(2.94482887675143,1.,-2.73003657371617));
#60065=CARTESIAN_POINT('Ctrl Pts',(2.94823023414364,1.,-2.73688288329808));
#60066=CARTESIAN_POINT('Ctrl Pts',(2.95159737214266,1.,-2.74375379492172));
#60067=CARTESIAN_POINT('Ctrl Pts',(2.95493069316161,1.,-2.75064903318947));
#60068=CARTESIAN_POINT('Ctrl Pts',(2.95823097665896,1.,-2.7575686788835));
#60069=CARTESIAN_POINT('Ctrl Pts',(2.96149914764818,1.,-2.76451296269557));
#60070=CARTESIAN_POINT('Ctrl Pts',(2.96473605585583,1.,-2.77148206836498));
#60071=CARTESIAN_POINT('Ctrl Pts',(2.96794221043036,1.,-2.7784758954285));
#60072=CARTESIAN_POINT('Ctrl Pts',(2.97111781461465,1.,-2.78549409123769));
#60073=CARTESIAN_POINT('Ctrl Pts',(2.9742628834758,1.,-2.79253615718248));
#60074=CARTESIAN_POINT('Ctrl Pts',(2.97737733718287,1.,-2.7996015327823));
#60075=CARTESIAN_POINT('Ctrl Pts',(2.98046109647241,1.,-2.80668968101106));
#60076=CARTESIAN_POINT('Ctrl Pts',(2.98351419779767,1.,-2.81380019196286));
#60077=CARTESIAN_POINT('Ctrl Pts',(2.9865368066918,1.,-2.82093279065457));
#60078=CARTESIAN_POINT('Ctrl Pts',(2.98952916401446,1.,-2.82808728190157));
#60079=CARTESIAN_POINT('Ctrl Pts',(2.99249155170339,1.,-2.83526351254248));
#60080=CARTESIAN_POINT('Ctrl Pts',(2.99542425341685,1.,-2.84246132984415));
#60081=CARTESIAN_POINT('Ctrl Pts',(2.99832751144925,1.,-2.84968053289451));
#60082=CARTESIAN_POINT('Ctrl Pts',(3.00120150796095,1.,-2.85692085715686));
#60083=CARTESIAN_POINT('Ctrl Pts',(3.00404638316867,1.,-2.86418200833667));
#60084=CARTESIAN_POINT('Ctrl Pts',(3.00686224485784,1.,-2.87146368430502));
#60085=CARTESIAN_POINT('Ctrl Pts',(3.00964918108476,1.,-2.87876560072727));
#60086=CARTESIAN_POINT('Ctrl Pts',(3.01240727308829,1.,-2.8860875170608));
#60087=CARTESIAN_POINT('Ctrl Pts',(3.01513660431928,1.,-2.89342925566321));
#60088=CARTESIAN_POINT('Ctrl Pts',(3.01783725121981,1.,-2.9007906910105));
#60089=CARTESIAN_POINT('Ctrl Pts',(3.01997487193503,1.,-2.90669553302526));
#60090=CARTESIAN_POINT('Ctrl Pts',(3.02156522742431,1.,-2.91113297348212));
#60091=CARTESIAN_POINT('Ctrl Pts',(3.02261975104593,1.,-2.91409518070399));
#60092=CARTESIAN_POINT('Ctrl Pts',(3.02314558451372,1.,-2.91557726271063));
#60093=CARTESIAN_POINT('Origin',(3.02314558451372,0.,-2.91557726271063));
#60094=CARTESIAN_POINT('',(2.91557726271063,1.,-3.02314558451372));
#60095=CARTESIAN_POINT('Origin',(0.,0.,0.));
#60096=CARTESIAN_POINT('',(2.90994629141562,1.,-2.36531447826213));
#60097=CARTESIAN_POINT('Origin',(0.,1.,0.));
#60098=CARTESIAN_POINT('Ctrl Pts',(2.90994629141562,1.,-2.36531447826213));
#60099=CARTESIAN_POINT('Ctrl Pts',(2.90994629141562,0.666666666666667,-2.36531447826213));
#60100=CARTESIAN_POINT('Ctrl Pts',(2.90994629141562,0.333333333333333,-2.36531447826213));
#60101=CARTESIAN_POINT('Ctrl Pts',(2.90994629141562,-0.333333333333333,
-2.36531447826213));
#60102=CARTESIAN_POINT('Ctrl Pts',(2.90994629141562,-0.666666666666667,
-2.36531447826213));
#60103=CARTESIAN_POINT('Ctrl Pts',(2.90994629141562,-1.,-2.36531447826213));
#60104=CARTESIAN_POINT('Ctrl Pts',(3.35260583073571,-1.,-2.52982887637028));
#60105=CARTESIAN_POINT('Ctrl Pts',(3.35260583073571,1.,-2.52982887637028));
#60106=CARTESIAN_POINT('Ctrl Pts',(3.35105973714426,-1.,-2.52954136549357));
#60107=CARTESIAN_POINT('Ctrl Pts',(3.35105973714426,1.,-2.52954136549357));
#60108=CARTESIAN_POINT('Ctrl Pts',(3.34796903577628,-1.,-2.5289632161143));
#60109=CARTESIAN_POINT('Ctrl Pts',(3.34796903577628,1.,-2.5289632161143));
#60110=CARTESIAN_POINT('Ctrl Pts',(3.34333744117093,-1.,-2.52808660916879));
#60111=CARTESIAN_POINT('Ctrl Pts',(3.34333744117093,1.,-2.52808660916879));
#60112=CARTESIAN_POINT('Ctrl Pts',(3.33717090000955,-1.,-2.52689902691551));
#60113=CARTESIAN_POINT('Ctrl Pts',(3.33717090000955,1.,-2.52689902691551));
#60114=CARTESIAN_POINT('Ctrl Pts',(3.32947762189049,-1.,-2.52538321165774));
#60115=CARTESIAN_POINT('Ctrl Pts',(3.32947762189049,1.,-2.52538321165774));
#60116=CARTESIAN_POINT('Ctrl Pts',(3.32179931079521,-1.,-2.52383598396878));
#60117=CARTESIAN_POINT('Ctrl Pts',(3.32179931079521,1.,-2.52383598396878));
#60118=CARTESIAN_POINT('Ctrl Pts',(3.31413607874727,-1.,-2.52225724871375));
#60119=CARTESIAN_POINT('Ctrl Pts',(3.31413607874727,1.,-2.52225724871375));
#60120=CARTESIAN_POINT('Ctrl Pts',(3.30648808814986,-1.,-2.52064689568167));
#60121=CARTESIAN_POINT('Ctrl Pts',(3.30648808814986,1.,-2.52064689568167));
#60122=CARTESIAN_POINT('Ctrl Pts',(3.29885556387661,-1.,-2.51900480700548));
#60123=CARTESIAN_POINT('Ctrl Pts',(3.29885556387661,1.,-2.51900480700548));
#60124=CARTESIAN_POINT('Ctrl Pts',(3.2912387729863,-1.,-2.51733085123316));
#60125=CARTESIAN_POINT('Ctrl Pts',(3.2912387729863,1.,-2.51733085123316));
#60126=CARTESIAN_POINT('Ctrl Pts',(3.28363799702583,-1.,-2.51562487464215));
#60127=CARTESIAN_POINT('Ctrl Pts',(3.28363799702583,1.,-2.51562487464215));
#60128=CARTESIAN_POINT('Ctrl Pts',(3.27605350473048,-1.,-2.51388669270329));
#60129=CARTESIAN_POINT('Ctrl Pts',(3.27605350473048,1.,-2.51388669270329));
#60130=CARTESIAN_POINT('Ctrl Pts',(3.26848552888271,-1.,-2.51211608411539));
#60131=CARTESIAN_POINT('Ctrl Pts',(3.26848552888271,1.,-2.51211608411539));
#60132=CARTESIAN_POINT('Ctrl Pts',(3.26093423001716,-1.,-2.51031277813697));
#60133=CARTESIAN_POINT('Ctrl Pts',(3.26093423001716,1.,-2.51031277813697));
#60134=CARTESIAN_POINT('Ctrl Pts',(3.25339971461265,-1.,-2.50847647070936));
#60135=CARTESIAN_POINT('Ctrl Pts',(3.25339971461265,1.,-2.50847647070936));
#60136=CARTESIAN_POINT('Ctrl Pts',(3.24588208984042,-1.,-2.50660685940645));
#60137=CARTESIAN_POINT('Ctrl Pts',(3.24588208984042,1.,-2.50660685940645));
#60138=CARTESIAN_POINT('Ctrl Pts',(3.23838151080383,-1.,-2.50470367580078));
#60139=CARTESIAN_POINT('Ctrl Pts',(3.23838151080383,1.,-2.50470367580078));
#60140=CARTESIAN_POINT('Ctrl Pts',(3.23089822320596,-1.,-2.50276671338074));
#60141=CARTESIAN_POINT('Ctrl Pts',(3.23089822320596,1.,-2.50276671338074));
#60142=CARTESIAN_POINT('Ctrl Pts',(3.22343262620387,-1.,-2.5007958720187));
#60143=CARTESIAN_POINT('Ctrl Pts',(3.22343262620387,1.,-2.5007958720187));
#60144=CARTESIAN_POINT('Ctrl Pts',(3.21598526261157,-1.,-2.49879114599293));
#60145=CARTESIAN_POINT('Ctrl Pts',(3.21598526261157,1.,-2.49879114599293));
#60146=CARTESIAN_POINT('Ctrl Pts',(3.2085566984974,-1.,-2.49675252647298));
#60147=CARTESIAN_POINT('Ctrl Pts',(3.2085566984974,1.,-2.49675252647298));
#60148=CARTESIAN_POINT('Ctrl Pts',(3.20114742397549,-1.,-2.49467992057726));
#60149=CARTESIAN_POINT('Ctrl Pts',(3.20114742397549,1.,-2.49467992057726));
#60150=CARTESIAN_POINT('Ctrl Pts',(3.19375775555814,-1.,-2.4925730723986));
#60151=CARTESIAN_POINT('Ctrl Pts',(3.19375775555814,1.,-2.4925730723986));
#60152=CARTESIAN_POINT('Ctrl Pts',(3.18638771282315,-1.,-2.49043146334095));
#60153=CARTESIAN_POINT('Ctrl Pts',(3.18638771282315,1.,-2.49043146334095));
#60154=CARTESIAN_POINT('Ctrl Pts',(3.17903698136678,-1.,-2.48825428288243));
#60155=CARTESIAN_POINT('Ctrl Pts',(3.17903698136678,1.,-2.48825428288243));
#60156=CARTESIAN_POINT('Ctrl Pts',(3.17170518863357,-1.,-2.48604065348619));
#60157=CARTESIAN_POINT('Ctrl Pts',(3.17170518863357,1.,-2.48604065348619));
#60158=CARTESIAN_POINT('Ctrl Pts',(3.16439213290181,-1.,-2.48378981792739));
#60159=CARTESIAN_POINT('Ctrl Pts',(3.16439213290181,1.,-2.48378981792739));
#60160=CARTESIAN_POINT('Ctrl Pts',(3.15709802322735,-1.,-2.48150133566568));
#60161=CARTESIAN_POINT('Ctrl Pts',(3.15709802322735,1.,-2.48150133566568));
#60162=CARTESIAN_POINT('Ctrl Pts',(3.14982373241335,-1.,-2.47917529057016));
#60163=CARTESIAN_POINT('Ctrl Pts',(3.14982373241335,1.,-2.47917529057016));
#60164=CARTESIAN_POINT('Ctrl Pts',(3.14257099546531,-1.,-2.47681245356095));
#60165=CARTESIAN_POINT('Ctrl Pts',(3.14257099546531,1.,-2.47681245356095));
#60166=CARTESIAN_POINT('Ctrl Pts',(3.13534181229282,-1.,-2.47441378371923));
#60167=CARTESIAN_POINT('Ctrl Pts',(3.13534181229282,1.,-2.47441378371923));
#60168=CARTESIAN_POINT('Ctrl Pts',(3.12813790805948,-1.,-2.47197997765868));
#60169=CARTESIAN_POINT('Ctrl Pts',(3.12813790805948,1.,-2.47197997765868));
#60170=CARTESIAN_POINT('Ctrl Pts',(3.12096015766984,-1.,-2.4695109894747));
#60171=CARTESIAN_POINT('Ctrl Pts',(3.12096015766984,1.,-2.4695109894747));
#60172=CARTESIAN_POINT('Ctrl Pts',(3.11380805536124,-1.,-2.46700558843507));
#60173=CARTESIAN_POINT('Ctrl Pts',(3.11380805536124,1.,-2.46700558843507));
#60174=CARTESIAN_POINT('Ctrl Pts',(3.10667907901981,-1.,-2.46446082979645));
#60175=CARTESIAN_POINT('Ctrl Pts',(3.10667907901981,1.,-2.46446082979645));
#60176=CARTESIAN_POINT('Ctrl Pts',(3.09956993697048,-1.,-2.4618730850188));
#60177=CARTESIAN_POINT('Ctrl Pts',(3.09956993697048,1.,-2.4618730850188));
#60178=CARTESIAN_POINT('Ctrl Pts',(3.09247787931881,-1.,-2.45923912563875));
#60179=CARTESIAN_POINT('Ctrl Pts',(3.09247787931881,1.,-2.45923912563875));
#60180=CARTESIAN_POINT('Ctrl Pts',(3.08540206545313,-1.,-2.45655725437037));
#60181=CARTESIAN_POINT('Ctrl Pts',(3.08540206545313,1.,-2.45655725437037));
#60182=CARTESIAN_POINT('Ctrl Pts',(3.07834472886145,-1.,-2.45382826787795));
#60183=CARTESIAN_POINT('Ctrl Pts',(3.07834472886145,1.,-2.45382826787795));
#60184=CARTESIAN_POINT('Ctrl Pts',(3.0713129052131,-1.,-2.45105688854432));
#60185=CARTESIAN_POINT('Ctrl Pts',(3.0713129052131,1.,-2.45105688854432));
#60186=CARTESIAN_POINT('Ctrl Pts',(3.06431596421422,-1.,-2.44824970516558));
#60187=CARTESIAN_POINT('Ctrl Pts',(3.06431596421422,1.,-2.44824970516558));
#60188=CARTESIAN_POINT('Ctrl Pts',(3.05736242671521,-1.,-2.44541251892568));
#60189=CARTESIAN_POINT('Ctrl Pts',(3.05736242671521,1.,-2.44541251892568));
#60190=CARTESIAN_POINT('Ctrl Pts',(3.05045678021509,-1.,-2.44254768923109));
#60191=CARTESIAN_POINT('Ctrl Pts',(3.05045678021509,1.,-2.44254768923109));
#60192=CARTESIAN_POINT('Ctrl Pts',(3.04359685040545,-1.,-2.43965194061849));
#60193=CARTESIAN_POINT('Ctrl Pts',(3.04359685040545,1.,-2.43965194061849));
#60194=CARTESIAN_POINT('Ctrl Pts',(3.03676949672797,-1.,-2.43671278042394));
#60195=CARTESIAN_POINT('Ctrl Pts',(3.03676949672797,1.,-2.43671278042394));
#60196=CARTESIAN_POINT('Ctrl Pts',(3.02995534946946,-1.,-2.43371241361462));
#60197=CARTESIAN_POINT('Ctrl Pts',(3.02995534946946,1.,-2.43371241361462));
#60198=CARTESIAN_POINT('Ctrl Pts',(3.02313656035977,-1.,-2.43063415586615));
#60199=CARTESIAN_POINT('Ctrl Pts',(3.02313656035977,1.,-2.43063415586615));
#60200=CARTESIAN_POINT('Ctrl Pts',(3.01630420830493,-1.,-2.4274685626416));
#60201=CARTESIAN_POINT('Ctrl Pts',(3.01630420830493,1.,-2.4274685626416));
#60202=CARTESIAN_POINT('Ctrl Pts',(3.00946442616674,-1.,-2.42421849439625));
#60203=CARTESIAN_POINT('Ctrl Pts',(3.00946442616674,1.,-2.42421849439625));
#60204=CARTESIAN_POINT('Ctrl Pts',(3.00264868586038,-1.,-2.42090763946812));
#60205=CARTESIAN_POINT('Ctrl Pts',(3.00264868586038,1.,-2.42090763946812));
#60206=CARTESIAN_POINT('Ctrl Pts',(2.99590509293561,-1.,-2.4175732450056));
#60207=CARTESIAN_POINT('Ctrl Pts',(2.99590509293561,1.,-2.4175732450056));
#60208=CARTESIAN_POINT('Ctrl Pts',(2.98927983005851,-1.,-2.4142506419963));
#60209=CARTESIAN_POINT('Ctrl Pts',(2.98927983005851,1.,-2.4142506419963));
#60210=CARTESIAN_POINT('Ctrl Pts',(2.98280015815132,-1.,-2.41095909342591));
#60211=CARTESIAN_POINT('Ctrl Pts',(2.98280015815132,1.,-2.41095909342591));
#60212=CARTESIAN_POINT('Ctrl Pts',(2.97646002822395,-1.,-2.40768975073691));
#60213=CARTESIAN_POINT('Ctrl Pts',(2.97646002822395,1.,-2.40768975073691));
#60214=CARTESIAN_POINT('Ctrl Pts',(2.97019641312272,-1.,-2.40438604734848));
#60215=CARTESIAN_POINT('Ctrl Pts',(2.97019641312272,1.,-2.40438604734848));
#60216=CARTESIAN_POINT('Ctrl Pts',(2.9639043224018,-1.,-2.40095565711535));
#60217=CARTESIAN_POINT('Ctrl Pts',(2.9639043224018,1.,-2.40095565711535));
#60218=CARTESIAN_POINT('Ctrl Pts',(2.95748006482811,-1.,-2.39730553974412));
#60219=CARTESIAN_POINT('Ctrl Pts',(2.95748006482811,1.,-2.39730553974412));
#60220=CARTESIAN_POINT('Ctrl Pts',(2.95085857128372,-1.,-2.39337207631613));
#60221=CARTESIAN_POINT('Ctrl Pts',(2.95085857128372,1.,-2.39337207631613));
#60222=CARTESIAN_POINT('Ctrl Pts',(2.94404820669135,-1.,-2.38914929090806));
#60223=CARTESIAN_POINT('Ctrl Pts',(2.94404820669135,1.,-2.38914929090806));
#60224=CARTESIAN_POINT('Ctrl Pts',(2.93717903280599,-1.,-2.38472771516476));
#60225=CARTESIAN_POINT('Ctrl Pts',(2.93717903280599,1.,-2.38472771516476));
#60226=CARTESIAN_POINT('Ctrl Pts',(2.93049643640517,-1.,-2.3802898958232));
#60227=CARTESIAN_POINT('Ctrl Pts',(2.93049643640517,1.,-2.3802898958232));
#60228=CARTESIAN_POINT('Ctrl Pts',(2.92430340582912,-1.,-2.37606510524271));
#60229=CARTESIAN_POINT('Ctrl Pts',(2.92430340582912,1.,-2.37606510524271));
#60230=CARTESIAN_POINT('Ctrl Pts',(2.9189150379156,-1.,-2.37229381109939));
#60231=CARTESIAN_POINT('Ctrl Pts',(2.9189150379156,1.,-2.37229381109939));
#60232=CARTESIAN_POINT('Ctrl Pts',(2.91461249883016,-1.,-2.36919161373074));
#60233=CARTESIAN_POINT('Ctrl Pts',(2.91461249883016,1.,-2.36919161373074));
#60234=CARTESIAN_POINT('Ctrl Pts',(2.9115863784165,-1.,-2.36690501170317));
#60235=CARTESIAN_POINT('Ctrl Pts',(2.9115863784165,1.,-2.36690501170317));
#60236=CARTESIAN_POINT('Ctrl Pts',(2.91025813829606,-1.,-2.36578327194396));
#60237=CARTESIAN_POINT('Ctrl Pts',(2.91025813829606,1.,-2.36578327194396));
#60238=CARTESIAN_POINT('Ctrl Pts',(2.90989022547738,-1.,-2.36535052956704));
#60239=CARTESIAN_POINT('Ctrl Pts',(2.90989022547738,1.,-2.36535052956704));
#60240=CARTESIAN_POINT('Ctrl Pts',(2.90992398626098,-1.,-2.36524348105023));
#60241=CARTESIAN_POINT('Ctrl Pts',(2.90992398626098,1.,-2.36524348105023));
#60242=CARTESIAN_POINT('Ctrl Pts',(2.91001063062876,-1.,-2.36523532225181));
#60243=CARTESIAN_POINT('Ctrl Pts',(2.91001063062876,1.,-2.36523532225181));
#60244=CARTESIAN_POINT('',(3.35260583073571,1.,-2.52982887637028));
#60245=CARTESIAN_POINT('Ctrl Pts',(3.35260583073571,1.,-2.52982887637028));
#60246=CARTESIAN_POINT('Ctrl Pts',(3.35105973714426,1.,-2.52954136549357));
#60247=CARTESIAN_POINT('Ctrl Pts',(3.34796903577628,1.,-2.5289632161143));
#60248=CARTESIAN_POINT('Ctrl Pts',(3.34333744117093,1.,-2.52808660916879));
#60249=CARTESIAN_POINT('Ctrl Pts',(3.33717090000955,1.,-2.52689902691551));
#60250=CARTESIAN_POINT('Ctrl Pts',(3.32947762189049,1.,-2.52538321165774));
#60251=CARTESIAN_POINT('Ctrl Pts',(3.32179931079521,1.,-2.52383598396878));
#60252=CARTESIAN_POINT('Ctrl Pts',(3.31413607874727,1.,-2.52225724871375));
#60253=CARTESIAN_POINT('Ctrl Pts',(3.30648808814986,1.,-2.52064689568167));
#60254=CARTESIAN_POINT('Ctrl Pts',(3.29885556387661,1.,-2.51900480700548));
#60255=CARTESIAN_POINT('Ctrl Pts',(3.2912387729863,1.,-2.51733085123316));
#60256=CARTESIAN_POINT('Ctrl Pts',(3.28363799702583,1.,-2.51562487464215));
#60257=CARTESIAN_POINT('Ctrl Pts',(3.27605350473048,1.,-2.51388669270329));
#60258=CARTESIAN_POINT('Ctrl Pts',(3.26848552888271,1.,-2.51211608411539));
#60259=CARTESIAN_POINT('Ctrl Pts',(3.26093423001716,1.,-2.51031277813697));
#60260=CARTESIAN_POINT('Ctrl Pts',(3.25339971461265,1.,-2.50847647070936));
#60261=CARTESIAN_POINT('Ctrl Pts',(3.24588208984042,1.,-2.50660685940645));
#60262=CARTESIAN_POINT('Ctrl Pts',(3.23838151080383,1.,-2.50470367580078));
#60263=CARTESIAN_POINT('Ctrl Pts',(3.23089822320596,1.,-2.50276671338074));
#60264=CARTESIAN_POINT('Ctrl Pts',(3.22343262620387,1.,-2.5007958720187));
#60265=CARTESIAN_POINT('Ctrl Pts',(3.21598526261157,1.,-2.49879114599293));
#60266=CARTESIAN_POINT('Ctrl Pts',(3.2085566984974,1.,-2.49675252647298));
#60267=CARTESIAN_POINT('Ctrl Pts',(3.20114742397549,1.,-2.49467992057726));
#60268=CARTESIAN_POINT('Ctrl Pts',(3.19375775555814,1.,-2.4925730723986));
#60269=CARTESIAN_POINT('Ctrl Pts',(3.18638771282315,1.,-2.49043146334095));
#60270=CARTESIAN_POINT('Ctrl Pts',(3.17903698136678,1.,-2.48825428288243));
#60271=CARTESIAN_POINT('Ctrl Pts',(3.17170518863357,1.,-2.48604065348619));
#60272=CARTESIAN_POINT('Ctrl Pts',(3.16439213290181,1.,-2.48378981792739));
#60273=CARTESIAN_POINT('Ctrl Pts',(3.15709802322735,1.,-2.48150133566568));
#60274=CARTESIAN_POINT('Ctrl Pts',(3.14982373241335,1.,-2.47917529057016));
#60275=CARTESIAN_POINT('Ctrl Pts',(3.14257099546531,1.,-2.47681245356095));
#60276=CARTESIAN_POINT('Ctrl Pts',(3.13534181229282,1.,-2.47441378371923));
#60277=CARTESIAN_POINT('Ctrl Pts',(3.12813790805948,1.,-2.47197997765868));
#60278=CARTESIAN_POINT('Ctrl Pts',(3.12096015766984,1.,-2.4695109894747));
#60279=CARTESIAN_POINT('Ctrl Pts',(3.11380805536124,1.,-2.46700558843507));
#60280=CARTESIAN_POINT('Ctrl Pts',(3.10667907901981,1.,-2.46446082979645));
#60281=CARTESIAN_POINT('Ctrl Pts',(3.09956993697048,1.,-2.4618730850188));
#60282=CARTESIAN_POINT('Ctrl Pts',(3.09247787931881,1.,-2.45923912563875));
#60283=CARTESIAN_POINT('Ctrl Pts',(3.08540206545313,1.,-2.45655725437037));
#60284=CARTESIAN_POINT('Ctrl Pts',(3.07834472886145,1.,-2.45382826787795));
#60285=CARTESIAN_POINT('Ctrl Pts',(3.0713129052131,1.,-2.45105688854432));
#60286=CARTESIAN_POINT('Ctrl Pts',(3.06431596421422,1.,-2.44824970516558));
#60287=CARTESIAN_POINT('Ctrl Pts',(3.05736242671521,1.,-2.44541251892568));
#60288=CARTESIAN_POINT('Ctrl Pts',(3.05045678021509,1.,-2.44254768923109));
#60289=CARTESIAN_POINT('Ctrl Pts',(3.04359685040545,1.,-2.43965194061849));
#60290=CARTESIAN_POINT('Ctrl Pts',(3.03676949672797,1.,-2.43671278042394));
#60291=CARTESIAN_POINT('Ctrl Pts',(3.02995534946946,1.,-2.43371241361462));
#60292=CARTESIAN_POINT('Ctrl Pts',(3.02313656035977,1.,-2.43063415586615));
#60293=CARTESIAN_POINT('Ctrl Pts',(3.01630420830493,1.,-2.4274685626416));
#60294=CARTESIAN_POINT('Ctrl Pts',(3.00946442616674,1.,-2.42421849439625));
#60295=CARTESIAN_POINT('Ctrl Pts',(3.00264868586038,1.,-2.42090763946812));
#60296=CARTESIAN_POINT('Ctrl Pts',(2.99590509293561,1.,-2.4175732450056));
#60297=CARTESIAN_POINT('Ctrl Pts',(2.98927983005851,1.,-2.4142506419963));
#60298=CARTESIAN_POINT('Ctrl Pts',(2.98280015815132,1.,-2.41095909342591));
#60299=CARTESIAN_POINT('Ctrl Pts',(2.97646002822395,1.,-2.40768975073691));
#60300=CARTESIAN_POINT('Ctrl Pts',(2.97019641312272,1.,-2.40438604734848));
#60301=CARTESIAN_POINT('Ctrl Pts',(2.9639043224018,1.,-2.40095565711535));
#60302=CARTESIAN_POINT('Ctrl Pts',(2.95748006482811,1.,-2.39730553974412));
#60303=CARTESIAN_POINT('Ctrl Pts',(2.95085857128372,1.,-2.39337207631613));
#60304=CARTESIAN_POINT('Ctrl Pts',(2.94404820669135,1.,-2.38914929090806));
#60305=CARTESIAN_POINT('Ctrl Pts',(2.93717903280599,1.,-2.38472771516476));
#60306=CARTESIAN_POINT('Ctrl Pts',(2.93049643640517,1.,-2.3802898958232));
#60307=CARTESIAN_POINT('Ctrl Pts',(2.92430340582912,1.,-2.37606510524271));
#60308=CARTESIAN_POINT('Ctrl Pts',(2.9189150379156,1.,-2.37229381109939));
#60309=CARTESIAN_POINT('Ctrl Pts',(2.91461249883016,1.,-2.36919161373074));
#60310=CARTESIAN_POINT('Ctrl Pts',(2.91181344022628,1.,-2.36707658451709));
#60311=CARTESIAN_POINT('Ctrl Pts',(2.91051690822262,1.,-2.36599991765853));
#60312=CARTESIAN_POINT('Ctrl Pts',(2.9100577052777,1.,-2.36553202948741));
#60313=CARTESIAN_POINT('Ctrl Pts',(2.90995756655558,1.,-2.3653621118858));
#60314=CARTESIAN_POINT('Ctrl Pts',(2.90994629141562,1.,-2.36531447826213));
#60315=CARTESIAN_POINT('',(3.35260583073571,0.,-2.52982887637028));
#60316=CARTESIAN_POINT('Ctrl Pts',(3.1487152044751,-1.,-2.03668666247593));
#60317=CARTESIAN_POINT('Ctrl Pts',(3.1487152044751,1.,-2.03668666247593));
#60318=CARTESIAN_POINT('Ctrl Pts',(3.14869618937258,-1.,-2.03660173757879));
#60319=CARTESIAN_POINT('Ctrl Pts',(3.14869618937258,1.,-2.03660173757879));
#60320=CARTESIAN_POINT('Ctrl Pts',(3.14878756590812,-1.,-2.03653654935592));
#60321=CARTESIAN_POINT('Ctrl Pts',(3.14878756590812,1.,-2.03653654935592));
#60322=CARTESIAN_POINT('Ctrl Pts',(3.14931281968048,-1.,-2.03675273049189));
#60323=CARTESIAN_POINT('Ctrl Pts',(3.14931281968048,1.,-2.03675273049189));
#60324=CARTESIAN_POINT('Ctrl Pts',(3.15079010635742,-1.,-2.03766932526445));
#60325=CARTESIAN_POINT('Ctrl Pts',(3.15079010635742,1.,-2.03766932526445));
#60326=CARTESIAN_POINT('Ctrl Pts',(3.15389991674792,-1.,-2.03984073791519));
#60327=CARTESIAN_POINT('Ctrl Pts',(3.15389991674792,1.,-2.03984073791519));
#60328=CARTESIAN_POINT('Ctrl Pts',(3.15817983946367,-1.,-2.04297406404027));
#60329=CARTESIAN_POINT('Ctrl Pts',(3.15817983946367,1.,-2.04297406404027));
#60330=CARTESIAN_POINT('Ctrl Pts',(3.16343165058912,-1.,-2.04693331247446));
#60331=CARTESIAN_POINT('Ctrl Pts',(3.16343165058912,1.,-2.04693331247446));
#60332=CARTESIAN_POINT('Ctrl Pts',(3.16936341689527,-1.,-2.05151770247233));
#60333=CARTESIAN_POINT('Ctrl Pts',(3.16936341689527,1.,-2.05151770247233));
#60334=CARTESIAN_POINT('Ctrl Pts',(3.17564906975371,-1.,-2.05650186773132));
#60335=CARTESIAN_POINT('Ctrl Pts',(3.17564906975371,1.,-2.05650186773132));
#60336=CARTESIAN_POINT('Ctrl Pts',(3.18197692964614,-1.,-2.06166849827101));
#60337=CARTESIAN_POINT('Ctrl Pts',(3.18197692964614,1.,-2.06166849827101));
#60338=CARTESIAN_POINT('Ctrl Pts',(3.18809755562368,-1.,-2.06684062744112));
#60339=CARTESIAN_POINT('Ctrl Pts',(3.18809755562368,1.,-2.06684062744112));
#60340=CARTESIAN_POINT('Ctrl Pts',(3.19388465568252,-1.,-2.07192253497857));
#60341=CARTESIAN_POINT('Ctrl Pts',(3.19388465568252,1.,-2.07192253497857));
#60342=CARTESIAN_POINT('Ctrl Pts',(3.19934132836019,-1.,-2.07690441870722));
#60343=CARTESIAN_POINT('Ctrl Pts',(3.19934132836019,1.,-2.07690441870722));
#60344=CARTESIAN_POINT('Ctrl Pts',(3.2045481863073,-1.,-2.08182850370878));
#60345=CARTESIAN_POINT('Ctrl Pts',(3.2045481863073,1.,-2.08182850370878));
#60346=CARTESIAN_POINT('Ctrl Pts',(3.20962575845463,-1.,-2.08676465517455));
#60347=CARTESIAN_POINT('Ctrl Pts',(3.20962575845463,1.,-2.08676465517455));
#60348=CARTESIAN_POINT('Ctrl Pts',(3.21469429601654,-1.,-2.09178419460443));
#60349=CARTESIAN_POINT('Ctrl Pts',(3.21469429601654,1.,-2.09178419460443));
#60350=CARTESIAN_POINT('Ctrl Pts',(3.21982707347009,-1.,-2.09692958434895));
#60351=CARTESIAN_POINT('Ctrl Pts',(3.21982707347009,1.,-2.09692958434895));
#60352=CARTESIAN_POINT('Ctrl Pts',(3.22503437553434,-1.,-2.10220384298492));
#60353=CARTESIAN_POINT('Ctrl Pts',(3.22503437553434,1.,-2.10220384298492));
#60354=CARTESIAN_POINT('Ctrl Pts',(3.23028945793289,-1.,-2.10758699642451));
#60355=CARTESIAN_POINT('Ctrl Pts',(3.23028945793289,1.,-2.10758699642451));
#60356=CARTESIAN_POINT('Ctrl Pts',(3.23554444767099,-1.,-2.11304604021773));
#60357=CARTESIAN_POINT('Ctrl Pts',(3.23554444767099,1.,-2.11304604021773));
#60358=CARTESIAN_POINT('Ctrl Pts',(3.24074905517293,-1.,-2.11854673326979));
#60359=CARTESIAN_POINT('Ctrl Pts',(3.24074905517293,1.,-2.11854673326979));
#60360=CARTESIAN_POINT('Ctrl Pts',(3.24587102613376,-1.,-2.12406646410962));
#60361=CARTESIAN_POINT('Ctrl Pts',(3.24587102613376,1.,-2.12406646410962));
#60362=CARTESIAN_POINT('Ctrl Pts',(3.25090574494028,-1.,-2.12960028396832));
#60363=CARTESIAN_POINT('Ctrl Pts',(3.25090574494028,1.,-2.12960028396832));
#60364=CARTESIAN_POINT('Ctrl Pts',(3.25586495065054,-1.,-2.13515375878803));
#60365=CARTESIAN_POINT('Ctrl Pts',(3.25586495065054,1.,-2.13515375878803));
#60366=CARTESIAN_POINT('Ctrl Pts',(3.26077002641879,-1.,-2.14073870754264));
#60367=CARTESIAN_POINT('Ctrl Pts',(3.26077002641879,1.,-2.14073870754264));
#60368=CARTESIAN_POINT('Ctrl Pts',(3.26564388189759,-1.,-2.1463680529566));
#60369=CARTESIAN_POINT('Ctrl Pts',(3.26564388189759,1.,-2.1463680529566));
#60370=CARTESIAN_POINT('Ctrl Pts',(3.27050245897228,-1.,-2.15205043199808));
#60371=CARTESIAN_POINT('Ctrl Pts',(3.27050245897228,1.,-2.15205043199808));
#60372=CARTESIAN_POINT('Ctrl Pts',(3.27534954469187,-1.,-2.15778690038347));
#60373=CARTESIAN_POINT('Ctrl Pts',(3.27534954469187,1.,-2.15778690038347));
#60374=CARTESIAN_POINT('Ctrl Pts',(3.280181508414,-1.,-2.16357391934425));
#60375=CARTESIAN_POINT('Ctrl Pts',(3.280181508414,1.,-2.16357391934425));
#60376=CARTESIAN_POINT('Ctrl Pts',(3.28499019979724,-1.,-2.16940517773455));
#60377=CARTESIAN_POINT('Ctrl Pts',(3.28499019979724,1.,-2.16940517773455));
#60378=CARTESIAN_POINT('Ctrl Pts',(3.28976645712568,-1.,-2.17527380048423));
#60379=CARTESIAN_POINT('Ctrl Pts',(3.28976645712568,1.,-2.17527380048423));
#60380=CARTESIAN_POINT('Ctrl Pts',(3.2945036150049,-1.,-2.18117455557065));
#60381=CARTESIAN_POINT('Ctrl Pts',(3.2945036150049,1.,-2.18117455557065));
#60382=CARTESIAN_POINT('Ctrl Pts',(3.29920022557639,-1.,-2.18710556500327));
#60383=CARTESIAN_POINT('Ctrl Pts',(3.29920022557639,1.,-2.18710556500327));
#60384=CARTESIAN_POINT('Ctrl Pts',(3.30385816281831,-1.,-2.19306710376111));
#60385=CARTESIAN_POINT('Ctrl Pts',(3.30385816281831,1.,-2.19306710376111));
#60386=CARTESIAN_POINT('Ctrl Pts',(3.30848134694595,-1.,-2.19906078949923));
#60387=CARTESIAN_POINT('Ctrl Pts',(3.30848134694595,1.,-2.19906078949923));
#60388=CARTESIAN_POINT('Ctrl Pts',(3.31307424608949,-1.,-2.20508863150607));
#60389=CARTESIAN_POINT('Ctrl Pts',(3.31307424608949,1.,-2.20508863150607));
#60390=CARTESIAN_POINT('Ctrl Pts',(3.31764044024235,-1.,-2.21115211847875));
#60391=CARTESIAN_POINT('Ctrl Pts',(3.31764044024235,1.,-2.21115211847875));
#60392=CARTESIAN_POINT('Ctrl Pts',(3.32218125618968,-1.,-2.21725135110898));
#60393=CARTESIAN_POINT('Ctrl Pts',(3.32218125618968,1.,-2.21725135110898));
#60394=CARTESIAN_POINT('Ctrl Pts',(3.3266964672289,-1.,-2.22338548312772));
#60395=CARTESIAN_POINT('Ctrl Pts',(3.3266964672289,1.,-2.22338548312772));
#60396=CARTESIAN_POINT('Ctrl Pts',(3.33118487773611,-1.,-2.22955308907233));
#60397=CARTESIAN_POINT('Ctrl Pts',(3.33118487773611,1.,-2.22955308907233));
#60398=CARTESIAN_POINT('Ctrl Pts',(3.33564495756481,-1.,-2.23575256328812));
#60399=CARTESIAN_POINT('Ctrl Pts',(3.33564495756481,1.,-2.23575256328812));
#60400=CARTESIAN_POINT('Ctrl Pts',(3.34007543738025,-1.,-2.24198249391422));
#60401=CARTESIAN_POINT('Ctrl Pts',(3.34007543738025,1.,-2.24198249391422));
#60402=CARTESIAN_POINT('Ctrl Pts',(3.34447596770723,-1.,-2.24824207678256));
#60403=CARTESIAN_POINT('Ctrl Pts',(3.34447596770723,1.,-2.24824207678256));
#60404=CARTESIAN_POINT('Ctrl Pts',(3.34884690292285,-1.,-2.25453097693483));
#60405=CARTESIAN_POINT('Ctrl Pts',(3.34884690292285,1.,-2.25453097693483));
#60406=CARTESIAN_POINT('Ctrl Pts',(3.35318902552626,-1.,-2.26084915222449));
#60407=CARTESIAN_POINT('Ctrl Pts',(3.35318902552626,1.,-2.26084915222449));
#60408=CARTESIAN_POINT('Ctrl Pts',(3.35750328523061,-1.,-2.2671966857991));
#60409=CARTESIAN_POINT('Ctrl Pts',(3.35750328523061,1.,-2.2671966857991));
#60410=CARTESIAN_POINT('Ctrl Pts',(3.36179055004409,-1.,-2.2735736262093));
#60411=CARTESIAN_POINT('Ctrl Pts',(3.36179055004409,1.,-2.2735736262093));
#60412=CARTESIAN_POINT('Ctrl Pts',(3.36605130713076,-1.,-2.27997979458037));
#60413=CARTESIAN_POINT('Ctrl Pts',(3.36605130713076,1.,-2.27997979458037));
#60414=CARTESIAN_POINT('Ctrl Pts',(3.37028570206488,-1.,-2.28641481081137));
#60415=CARTESIAN_POINT('Ctrl Pts',(3.37028570206488,1.,-2.28641481081137));
#60416=CARTESIAN_POINT('Ctrl Pts',(3.37449367172826,-1.,-2.29287818007393));
#60417=CARTESIAN_POINT('Ctrl Pts',(3.37449367172826,1.,-2.29287818007393));
#60418=CARTESIAN_POINT('Ctrl Pts',(3.37867504959433,-1.,-2.29936936127624));
#60419=CARTESIAN_POINT('Ctrl Pts',(3.37867504959433,1.,-2.29936936127624));
#60420=CARTESIAN_POINT('Ctrl Pts',(3.3828296733661,-1.,-2.30588783640343));
#60421=CARTESIAN_POINT('Ctrl Pts',(3.3828296733661,1.,-2.30588783640343));
#60422=CARTESIAN_POINT('Ctrl Pts',(3.38695751492462,-1.,-2.31243319489367));
#60423=CARTESIAN_POINT('Ctrl Pts',(3.38695751492462,1.,-2.31243319489367));
#60424=CARTESIAN_POINT('Ctrl Pts',(3.39105869474822,-1.,-2.31900513925424));
#60425=CARTESIAN_POINT('Ctrl Pts',(3.39105869474822,1.,-2.31900513925424));
#60426=CARTESIAN_POINT('Ctrl Pts',(3.39513342019756,-1.,-2.3256034390248));
#60427=CARTESIAN_POINT('Ctrl Pts',(3.39513342019756,1.,-2.3256034390248));
#60428=CARTESIAN_POINT('Ctrl Pts',(3.39918194577956,-1.,-2.33222789882489));
#60429=CARTESIAN_POINT('Ctrl Pts',(3.39918194577956,1.,-2.33222789882489));
#60430=CARTESIAN_POINT('Ctrl Pts',(3.40320452776743,-1.,-2.33887832342782));
#60431=CARTESIAN_POINT('Ctrl Pts',(3.40320452776743,1.,-2.33887832342782));
#60432=CARTESIAN_POINT('Ctrl Pts',(3.40720137404297,-1.,-2.34555447649188));
#60433=CARTESIAN_POINT('Ctrl Pts',(3.40720137404297,1.,-2.34555447649188));
#60434=CARTESIAN_POINT('Ctrl Pts',(3.41117262314119,-1.,-2.35225606824109));
#60435=CARTESIAN_POINT('Ctrl Pts',(3.41117262314119,1.,-2.35225606824109));
#60436=CARTESIAN_POINT('Ctrl Pts',(3.41511836751469,-1.,-2.35898278606946));
#60437=CARTESIAN_POINT('Ctrl Pts',(3.41511836751469,1.,-2.35898278606946));
#60438=CARTESIAN_POINT('Ctrl Pts',(3.41903866635852,-1.,-2.36573431470642));
#60439=CARTESIAN_POINT('Ctrl Pts',(3.41903866635852,1.,-2.36573431470642));
#60440=CARTESIAN_POINT('Ctrl Pts',(3.42293356216511,-1.,-2.37251035954292));
#60441=CARTESIAN_POINT('Ctrl Pts',(3.42293356216511,1.,-2.37251035954292));
#60442=CARTESIAN_POINT('Ctrl Pts',(3.42680309754399,-1.,-2.37931067028926));
#60443=CARTESIAN_POINT('Ctrl Pts',(3.42680309754399,1.,-2.37931067028926));
#60444=CARTESIAN_POINT('Ctrl Pts',(3.43064732712919,-1.,-2.38613505843552));
#60445=CARTESIAN_POINT('Ctrl Pts',(3.43064732712919,1.,-2.38613505843552));
#60446=CARTESIAN_POINT('Ctrl Pts',(3.4344663067854,-1.,-2.39298338804493));
#60447=CARTESIAN_POINT('Ctrl Pts',(3.4344663067854,1.,-2.39298338804493));
#60448=CARTESIAN_POINT('Ctrl Pts',(3.43750133064416,-1.,-2.39848113410292));
#60449=CARTESIAN_POINT('Ctrl Pts',(3.43750133064416,1.,-2.39848113410292));
#60450=CARTESIAN_POINT('Ctrl Pts',(3.43976627484234,-1.,-2.40261515589405));
#60451=CARTESIAN_POINT('Ctrl Pts',(3.43976627484234,1.,-2.40261515589405));
#60452=CARTESIAN_POINT('Ctrl Pts',(3.44127120683039,-1.,-2.4053759295909));
#60453=CARTESIAN_POINT('Ctrl Pts',(3.44127120683039,1.,-2.4053759295909));
#60454=CARTESIAN_POINT('Ctrl Pts',(3.44202241512147,-1.,-2.40675750623143));
#60455=CARTESIAN_POINT('Ctrl Pts',(3.44202241512147,1.,-2.40675750623143));
#60456=CARTESIAN_POINT('',(3.14877060440327,1.,-2.03660101169715));
#60457=CARTESIAN_POINT('Ctrl Pts',(3.14877060440327,-1.,-2.03660101169715));
#60458=CARTESIAN_POINT('Ctrl Pts',(3.14877060440327,-0.666666666666667,
-2.03660101169715));
#60459=CARTESIAN_POINT('Ctrl Pts',(3.14877060440327,-0.333333333333333,
-2.03660101169715));
#60460=CARTESIAN_POINT('Ctrl Pts',(3.14877060440327,0.333333333333333,-2.03660101169715));
#60461=CARTESIAN_POINT('Ctrl Pts',(3.14877060440328,0.666666666666667,-2.03660101169714));
#60462=CARTESIAN_POINT('Ctrl Pts',(3.14877060440328,1.,-2.03660101169714));
#60463=CARTESIAN_POINT('',(3.44202241512147,1.,-2.40675750623143));
#60464=CARTESIAN_POINT('',(3.44202241512147,0.,-2.40675750623143));
#60465=CARTESIAN_POINT('Ctrl Pts',(3.14877060440327,1.,-2.03660101169715));
#60466=CARTESIAN_POINT('Ctrl Pts',(3.14881939088124,1.,-2.03659701539259));
#60467=CARTESIAN_POINT('Ctrl Pts',(3.1490119366901,1.,-2.03663974554932));
#60468=CARTESIAN_POINT('Ctrl Pts',(3.14959882629804,1.,-2.03693188810544));
#60469=CARTESIAN_POINT('Ctrl Pts',(3.15102344775328,1.,-2.03783225495961));
#60470=CARTESIAN_POINT('Ctrl Pts',(3.15389991674792,1.,-2.03984073791519));
#60471=CARTESIAN_POINT('Ctrl Pts',(3.15817983946367,1.,-2.04297406404027));
#60472=CARTESIAN_POINT('Ctrl Pts',(3.16343165058912,1.,-2.04693331247446));
#60473=CARTESIAN_POINT('Ctrl Pts',(3.16936341689527,1.,-2.05151770247233));
#60474=CARTESIAN_POINT('Ctrl Pts',(3.17564906975371,1.,-2.05650186773132));
#60475=CARTESIAN_POINT('Ctrl Pts',(3.18197692964614,1.,-2.06166849827101));
#60476=CARTESIAN_POINT('Ctrl Pts',(3.18809755562368,1.,-2.06684062744112));
#60477=CARTESIAN_POINT('Ctrl Pts',(3.19388465568252,1.,-2.07192253497857));
#60478=CARTESIAN_POINT('Ctrl Pts',(3.19934132836019,1.,-2.07690441870722));
#60479=CARTESIAN_POINT('Ctrl Pts',(3.2045481863073,1.,-2.08182850370878));
#60480=CARTESIAN_POINT('Ctrl Pts',(3.20962575845463,1.,-2.08676465517455));
#60481=CARTESIAN_POINT('Ctrl Pts',(3.21469429601654,1.,-2.09178419460443));
#60482=CARTESIAN_POINT('Ctrl Pts',(3.21982707347009,1.,-2.09692958434895));
#60483=CARTESIAN_POINT('Ctrl Pts',(3.22503437553434,1.,-2.10220384298492));
#60484=CARTESIAN_POINT('Ctrl Pts',(3.23028945793289,1.,-2.10758699642451));
#60485=CARTESIAN_POINT('Ctrl Pts',(3.23554444767099,1.,-2.11304604021773));
#60486=CARTESIAN_POINT('Ctrl Pts',(3.24074905517293,1.,-2.11854673326979));
#60487=CARTESIAN_POINT('Ctrl Pts',(3.24587102613376,1.,-2.12406646410962));
#60488=CARTESIAN_POINT('Ctrl Pts',(3.25090574494028,1.,-2.12960028396832));
#60489=CARTESIAN_POINT('Ctrl Pts',(3.25586495065054,1.,-2.13515375878803));
#60490=CARTESIAN_POINT('Ctrl Pts',(3.26077002641879,1.,-2.14073870754264));
#60491=CARTESIAN_POINT('Ctrl Pts',(3.26564388189759,1.,-2.1463680529566));
#60492=CARTESIAN_POINT('Ctrl Pts',(3.27050245897228,1.,-2.15205043199808));
#60493=CARTESIAN_POINT('Ctrl Pts',(3.27534954469187,1.,-2.15778690038347));
#60494=CARTESIAN_POINT('Ctrl Pts',(3.280181508414,1.,-2.16357391934425));
#60495=CARTESIAN_POINT('Ctrl Pts',(3.28499019979724,1.,-2.16940517773455));
#60496=CARTESIAN_POINT('Ctrl Pts',(3.28976645712568,1.,-2.17527380048423));
#60497=CARTESIAN_POINT('Ctrl Pts',(3.2945036150049,1.,-2.18117455557065));
#60498=CARTESIAN_POINT('Ctrl Pts',(3.29920022557639,1.,-2.18710556500327));
#60499=CARTESIAN_POINT('Ctrl Pts',(3.30385816281831,1.,-2.19306710376111));
#60500=CARTESIAN_POINT('Ctrl Pts',(3.30848134694595,1.,-2.19906078949923));
#60501=CARTESIAN_POINT('Ctrl Pts',(3.31307424608949,1.,-2.20508863150607));
#60502=CARTESIAN_POINT('Ctrl Pts',(3.31764044024235,1.,-2.21115211847875));
#60503=CARTESIAN_POINT('Ctrl Pts',(3.32218125618968,1.,-2.21725135110898));
#60504=CARTESIAN_POINT('Ctrl Pts',(3.3266964672289,1.,-2.22338548312772));
#60505=CARTESIAN_POINT('Ctrl Pts',(3.33118487773611,1.,-2.22955308907233));
#60506=CARTESIAN_POINT('Ctrl Pts',(3.33564495756481,1.,-2.23575256328812));
#60507=CARTESIAN_POINT('Ctrl Pts',(3.34007543738025,1.,-2.24198249391422));
#60508=CARTESIAN_POINT('Ctrl Pts',(3.34447596770723,1.,-2.24824207678256));
#60509=CARTESIAN_POINT('Ctrl Pts',(3.34884690292285,1.,-2.25453097693483));
#60510=CARTESIAN_POINT('Ctrl Pts',(3.35318902552626,1.,-2.26084915222449));
#60511=CARTESIAN_POINT('Ctrl Pts',(3.35750328523061,1.,-2.2671966857991));
#60512=CARTESIAN_POINT('Ctrl Pts',(3.36179055004409,1.,-2.2735736262093));
#60513=CARTESIAN_POINT('Ctrl Pts',(3.36605130713076,1.,-2.27997979458037));
#60514=CARTESIAN_POINT('Ctrl Pts',(3.37028570206488,1.,-2.28641481081137));
#60515=CARTESIAN_POINT('Ctrl Pts',(3.37449367172826,1.,-2.29287818007393));
#60516=CARTESIAN_POINT('Ctrl Pts',(3.37867504959433,1.,-2.29936936127624));
#60517=CARTESIAN_POINT('Ctrl Pts',(3.3828296733661,1.,-2.30588783640343));
#60518=CARTESIAN_POINT('Ctrl Pts',(3.38695751492462,1.,-2.31243319489367));
#60519=CARTESIAN_POINT('Ctrl Pts',(3.39105869474822,1.,-2.31900513925424));
#60520=CARTESIAN_POINT('Ctrl Pts',(3.39513342019756,1.,-2.3256034390248));
#60521=CARTESIAN_POINT('Ctrl Pts',(3.39918194577956,1.,-2.33222789882489));
#60522=CARTESIAN_POINT('Ctrl Pts',(3.40320452776743,1.,-2.33887832342782));
#60523=CARTESIAN_POINT('Ctrl Pts',(3.40720137404297,1.,-2.34555447649188));
#60524=CARTESIAN_POINT('Ctrl Pts',(3.41117262314119,1.,-2.35225606824109));
#60525=CARTESIAN_POINT('Ctrl Pts',(3.41511836751469,1.,-2.35898278606946));
#60526=CARTESIAN_POINT('Ctrl Pts',(3.41903866635852,1.,-2.36573431470642));
#60527=CARTESIAN_POINT('Ctrl Pts',(3.42293356216511,1.,-2.37251035954292));
#60528=CARTESIAN_POINT('Ctrl Pts',(3.42680309754399,1.,-2.37931067028926));
#60529=CARTESIAN_POINT('Ctrl Pts',(3.43064732712919,1.,-2.38613505843552));
#60530=CARTESIAN_POINT('Ctrl Pts',(3.4344663067854,1.,-2.39298338804493));
#60531=CARTESIAN_POINT('Ctrl Pts',(3.43750133064416,1.,-2.39848113410292));
#60532=CARTESIAN_POINT('Ctrl Pts',(3.43976627484234,1.,-2.40261515589405));
#60533=CARTESIAN_POINT('Ctrl Pts',(3.44127120683039,1.,-2.4053759295909));
#60534=CARTESIAN_POINT('Ctrl Pts',(3.44202241512147,1.,-2.40675750623143));
#60535=CARTESIAN_POINT('Origin',(3.44202241512147,0.,-2.40675750623143));
#60536=CARTESIAN_POINT('',(3.35260583073571,1.,-2.52982887637028));
#60537=CARTESIAN_POINT('Origin',(0.,0.,0.));
#60538=CARTESIAN_POINT('',(3.24413672884812,1.,-1.88097764062697));
#60539=CARTESIAN_POINT('Origin',(0.,1.,0.));
#60540=CARTESIAN_POINT('Ctrl Pts',(3.24413672884812,1.,-1.88097764062697));
#60541=CARTESIAN_POINT('Ctrl Pts',(3.24413672884812,0.666666666666667,-1.88097764062697));
#60542=CARTESIAN_POINT('Ctrl Pts',(3.24413672884812,0.333333333333333,-1.88097764062697));
#60543=CARTESIAN_POINT('Ctrl Pts',(3.24413672884812,-0.333333333333333,
-1.88097764062697));
#60544=CARTESIAN_POINT('Ctrl Pts',(3.24413672884812,-0.666666666666667,
-1.88097764062697));
#60545=CARTESIAN_POINT('Ctrl Pts',(3.24413672884812,-1.,-1.88097764062697));
#60546=CARTESIAN_POINT('Ctrl Pts',(3.70708211654725,-1.,-1.97421938526992));
#60547=CARTESIAN_POINT('Ctrl Pts',(3.70708211654725,1.,-1.97421938526992));
#60548=CARTESIAN_POINT('Ctrl Pts',(3.70551008132332,-1.,-1.97417727645308));
#60549=CARTESIAN_POINT('Ctrl Pts',(3.70551008132332,1.,-1.97417727645308));
#60550=CARTESIAN_POINT('Ctrl Pts',(3.70236698912904,-1.,-1.97408973726715));
#60551=CARTESIAN_POINT('Ctrl Pts',(3.70236698912904,1.,-1.97408973726715));
#60552=CARTESIAN_POINT('Ctrl Pts',(3.6976552856004,-1.,-1.97394846383216));
#60553=CARTESIAN_POINT('Ctrl Pts',(3.6976552856004,1.,-1.97394846383216));
#60554=CARTESIAN_POINT('Ctrl Pts',(3.69137888599902,-1.,-1.97374016225483));
#60555=CARTESIAN_POINT('Ctrl Pts',(3.69137888599902,1.,-1.97374016225483));
#60556=CARTESIAN_POINT('Ctrl Pts',(3.68354319915092,-1.,-1.97344650304519));
#60557=CARTESIAN_POINT('Ctrl Pts',(3.68354319915092,1.,-1.97344650304519));
#60558=CARTESIAN_POINT('Ctrl Pts',(3.67571738107084,-1.,-1.97311947678517));
#60559=CARTESIAN_POINT('Ctrl Pts',(3.67571738107084,1.,-1.97311947678517));
#60560=CARTESIAN_POINT('Ctrl Pts',(3.66790152752075,-1.,-1.97275897198678));
#60561=CARTESIAN_POINT('Ctrl Pts',(3.66790152752075,1.,-1.97275897198678));
#60562=CARTESIAN_POINT('Ctrl Pts',(3.6600957816636,-1.,-1.9723648543905));
#60563=CARTESIAN_POINT('Ctrl Pts',(3.6600957816636,1.,-1.9723648543905));
#60564=CARTESIAN_POINT('Ctrl Pts',(3.652300347166,-1.,-1.9719369724024));
#60565=CARTESIAN_POINT('Ctrl Pts',(3.652300347166,1.,-1.9719369724024));
#60566=CARTESIAN_POINT('Ctrl Pts',(3.64451546723514,-1.,-1.97147515441164));
#60567=CARTESIAN_POINT('Ctrl Pts',(3.64451546723514,1.,-1.97147515441164));
#60568=CARTESIAN_POINT('Ctrl Pts',(3.63674139590412,-1.,-1.97097920454464));
#60569=CARTESIAN_POINT('Ctrl Pts',(3.63674139590412,1.,-1.97097920454464));
#60570=CARTESIAN_POINT('Ctrl Pts',(3.62897836973293,-1.,-1.97044889850463));
#60571=CARTESIAN_POINT('Ctrl Pts',(3.62897836973293,1.,-1.97044889850463));
#60572=CARTESIAN_POINT('Ctrl Pts',(3.62122658401893,-1.,-1.96988398129978));
#60573=CARTESIAN_POINT('Ctrl Pts',(3.62122658401893,1.,-1.96988398129978));
#60574=CARTESIAN_POINT('Ctrl Pts',(3.61348615496704,-1.,-1.96928416040877));
#60575=CARTESIAN_POINT('Ctrl Pts',(3.61348615496704,1.,-1.96928416040877));
#60576=CARTESIAN_POINT('Ctrl Pts',(3.60575714017989,-1.,-1.9686491188594));
#60577=CARTESIAN_POINT('Ctrl Pts',(3.60575714017989,1.,-1.9686491188594));
#60578=CARTESIAN_POINT('Ctrl Pts',(3.59803959819938,-1.,-1.96797854118369));
#60579=CARTESIAN_POINT('Ctrl Pts',(3.59803959819938,1.,-1.96797854118369));
#60580=CARTESIAN_POINT('Ctrl Pts',(3.59033364022801,-1.,-1.96727213799544));
#60581=CARTESIAN_POINT('Ctrl Pts',(3.59033364022801,1.,-1.96727213799544));
#60582=CARTESIAN_POINT('Ctrl Pts',(3.58263947663829,-1.,-1.96652966688911));
#60583=CARTESIAN_POINT('Ctrl Pts',(3.58263947663829,1.,-1.96652966688911));
#60584=CARTESIAN_POINT('Ctrl Pts',(3.57495748600959,-1.,-1.96575096652789));
#60585=CARTESIAN_POINT('Ctrl Pts',(3.57495748600959,1.,-1.96575096652789));
#60586=CARTESIAN_POINT('Ctrl Pts',(3.56728820357791,-1.,-1.96493594634567));
#60587=CARTESIAN_POINT('Ctrl Pts',(3.56728820357791,1.,-1.96493594634567));
#60588=CARTESIAN_POINT('Ctrl Pts',(3.55963218706096,-1.,-1.96408450906812));
#60589=CARTESIAN_POINT('Ctrl Pts',(3.55963218706096,1.,-1.96408450906812));
#60590=CARTESIAN_POINT('Ctrl Pts',(3.55198990600886,-1.,-1.96319648628644));
#60591=CARTESIAN_POINT('Ctrl Pts',(3.55198990600886,1.,-1.96319648628644));
#60592=CARTESIAN_POINT('Ctrl Pts',(3.54436163300443,-1.,-1.96227157573067));
#60593=CARTESIAN_POINT('Ctrl Pts',(3.54436163300443,1.,-1.96227157573067));
#60594=CARTESIAN_POINT('Ctrl Pts',(3.53674730625813,-1.,-1.96130926212689));
#60595=CARTESIAN_POINT('Ctrl Pts',(3.53674730625813,1.,-1.96130926212689));
#60596=CARTESIAN_POINT('Ctrl Pts',(3.52914648844351,-1.,-1.96030879411566));
#60597=CARTESIAN_POINT('Ctrl Pts',(3.52914648844351,1.,-1.96030879411566));
#60598=CARTESIAN_POINT('Ctrl Pts',(3.52155867431486,-1.,-1.95926936324461));
#60599=CARTESIAN_POINT('Ctrl Pts',(3.52155867431486,1.,-1.95926936324461));
#60600=CARTESIAN_POINT('Ctrl Pts',(3.51398354617794,-1.,-1.95819025316779));
#60601=CARTESIAN_POINT('Ctrl Pts',(3.51398354617794,1.,-1.95819025316779));
#60602=CARTESIAN_POINT('Ctrl Pts',(3.50642124159909,-1.,-1.95707099606511));
#60603=CARTESIAN_POINT('Ctrl Pts',(3.50642124159909,1.,-1.95707099606511));
#60604=CARTESIAN_POINT('Ctrl Pts',(3.49887263575583,-1.,-1.95591153823661));
#60605=CARTESIAN_POINT('Ctrl Pts',(3.49887263575583,1.,-1.95591153823661));
#60606=CARTESIAN_POINT('Ctrl Pts',(3.49133956289133,-1.,-1.95471236969643));
#60607=CARTESIAN_POINT('Ctrl Pts',(3.49133956289133,1.,-1.95471236969643));
#60608=CARTESIAN_POINT('Ctrl Pts',(3.48382414832634,-1.,-1.95347412486309));
#60609=CARTESIAN_POINT('Ctrl Pts',(3.48382414832634,1.,-1.95347412486309));
#60610=CARTESIAN_POINT('Ctrl Pts',(3.47632820495921,-1.,-1.95219722189876));
#60611=CARTESIAN_POINT('Ctrl Pts',(3.47632820495921,1.,-1.95219722189876));
#60612=CARTESIAN_POINT('Ctrl Pts',(3.46885258974191,-1.,-1.95088147859877));
#60613=CARTESIAN_POINT('Ctrl Pts',(3.46885258974191,1.,-1.95088147859877));
#60614=CARTESIAN_POINT('Ctrl Pts',(3.46139661060962,-1.,-1.94952575850197));
#60615=CARTESIAN_POINT('Ctrl Pts',(3.46139661060962,1.,-1.94952575850197));
#60616=CARTESIAN_POINT('Ctrl Pts',(3.45395731584051,-1.,-1.94812754766524));
#60617=CARTESIAN_POINT('Ctrl Pts',(3.45395731584051,1.,-1.94812754766524));
#60618=CARTESIAN_POINT('Ctrl Pts',(3.44653088665681,-1.,-1.94668377715329));
#60619=CARTESIAN_POINT('Ctrl Pts',(3.44653088665681,1.,-1.94668377715329));
#60620=CARTESIAN_POINT('Ctrl Pts',(3.43911410197687,-1.,-1.94519168842879));
#60621=CARTESIAN_POINT('Ctrl Pts',(3.43911410197687,1.,-1.94519168842879));
#60622=CARTESIAN_POINT('Ctrl Pts',(3.43170586602434,-1.,-1.94364973660284));
#60623=CARTESIAN_POINT('Ctrl Pts',(3.43170586602434,1.,-1.94364973660284));
#60624=CARTESIAN_POINT('Ctrl Pts',(3.42430850941503,-1.,-1.94205835913696));
#60625=CARTESIAN_POINT('Ctrl Pts',(3.42430850941503,1.,-1.94205835913696));
#60626=CARTESIAN_POINT('Ctrl Pts',(3.41692971994096,-1.,-1.94042111965246));
#60627=CARTESIAN_POINT('Ctrl Pts',(3.41692971994096,1.,-1.94042111965246));
#60628=CARTESIAN_POINT('Ctrl Pts',(3.40957978266642,-1.,-1.93874306008143));
#60629=CARTESIAN_POINT('Ctrl Pts',(3.40957978266642,1.,-1.93874306008143));
#60630=CARTESIAN_POINT('Ctrl Pts',(3.40226802104109,-1.,-1.93702857723098));
#60631=CARTESIAN_POINT('Ctrl Pts',(3.40226802104109,1.,-1.93702857723098));
#60632=CARTESIAN_POINT('Ctrl Pts',(3.39499923640795,-1.,-1.93527929945985));
#60633=CARTESIAN_POINT('Ctrl Pts',(3.39499923640795,1.,-1.93527929945985));
#60634=CARTESIAN_POINT('Ctrl Pts',(3.38777076883256,-1.,-1.93349233176788));
#60635=CARTESIAN_POINT('Ctrl Pts',(3.38777076883256,1.,-1.93349233176788));
#60636=CARTESIAN_POINT('Ctrl Pts',(3.3805676852555,-1.,-1.93165739093276));
#60637=CARTESIAN_POINT('Ctrl Pts',(3.3805676852555,1.,-1.93165739093276));
#60638=CARTESIAN_POINT('Ctrl Pts',(3.37336807068043,-1.,-1.92975993109877));
#60639=CARTESIAN_POINT('Ctrl Pts',(3.37336807068043,1.,-1.92975993109877));
#60640=CARTESIAN_POINT('Ctrl Pts',(3.36615168657567,-1.,-1.92778626543786));
#60641=CARTESIAN_POINT('Ctrl Pts',(3.36615168657567,1.,-1.92778626543786));
#60642=CARTESIAN_POINT('Ctrl Pts',(3.35890824422965,-1.,-1.92572846125756));
#60643=CARTESIAN_POINT('Ctrl Pts',(3.35890824422965,1.,-1.92572846125756));
#60644=CARTESIAN_POINT('Ctrl Pts',(3.35164424847223,-1.,-1.92358838440528));
#60645=CARTESIAN_POINT('Ctrl Pts',(3.35164424847223,1.,-1.92358838440528));
#60646=CARTESIAN_POINT('Ctrl Pts',(3.34439448941961,-1.,-1.92138450828404));
#60647=CARTESIAN_POINT('Ctrl Pts',(3.34439448941961,1.,-1.92138450828404));
#60648=CARTESIAN_POINT('Ctrl Pts',(3.33721230710012,-1.,-1.9191460961021));
#60649=CARTESIAN_POINT('Ctrl Pts',(3.33721230710012,1.,-1.9191460961021));
#60650=CARTESIAN_POINT('Ctrl Pts',(3.33014884257873,-1.,-1.91690081930332));
#60651=CARTESIAN_POINT('Ctrl Pts',(3.33014884257873,1.,-1.91690081930332));
#60652=CARTESIAN_POINT('Ctrl Pts',(3.32323403454535,-1.,-1.91466343916628));
#60653=CARTESIAN_POINT('Ctrl Pts',(3.32323403454535,1.,-1.91466343916628));
#60654=CARTESIAN_POINT('Ctrl Pts',(3.31646052426364,-1.,-1.91242616234442));
#60655=CARTESIAN_POINT('Ctrl Pts',(3.31646052426364,1.,-1.91242616234442));
#60656=CARTESIAN_POINT('Ctrl Pts',(3.30975721158596,-1.,-1.91014297830446));
#60657=CARTESIAN_POINT('Ctrl Pts',(3.30975721158596,1.,-1.91014297830446));
#60658=CARTESIAN_POINT('Ctrl Pts',(3.30300595568195,-1.,-1.90773912171341));
#60659=CARTESIAN_POINT('Ctrl Pts',(3.30300595568195,1.,-1.90773912171341));
#60660=CARTESIAN_POINT('Ctrl Pts',(3.29608978722113,-1.,-1.90513891864087));
#60661=CARTESIAN_POINT('Ctrl Pts',(3.29608978722113,1.,-1.90513891864087));
#60662=CARTESIAN_POINT('Ctrl Pts',(3.2889344860029,-1.,-1.90228971247527));
#60663=CARTESIAN_POINT('Ctrl Pts',(3.2889344860029,1.,-1.90228971247527));
#60664=CARTESIAN_POINT('Ctrl Pts',(3.28154737912352,-1.,-1.89918429230462));
#60665=CARTESIAN_POINT('Ctrl Pts',(3.28154737912352,1.,-1.89918429230462));
#60666=CARTESIAN_POINT('Ctrl Pts',(3.27407108933139,-1.,-1.89589172903793));
#60667=CARTESIAN_POINT('Ctrl Pts',(3.27407108933139,1.,-1.89589172903793));
#60668=CARTESIAN_POINT('Ctrl Pts',(3.26677653888676,-1.,-1.89255393500965));
#60669=CARTESIAN_POINT('Ctrl Pts',(3.26677653888676,1.,-1.89255393500965));
#60670=CARTESIAN_POINT('Ctrl Pts',(3.25999885193947,-1.,-1.88934996203698));
#60671=CARTESIAN_POINT('Ctrl Pts',(3.25999885193947,1.,-1.88934996203698));
#60672=CARTESIAN_POINT('Ctrl Pts',(3.25408686339463,-1.,-1.88646802523466));
#60673=CARTESIAN_POINT('Ctrl Pts',(3.25408686339463,1.,-1.88646802523466));
#60674=CARTESIAN_POINT('Ctrl Pts',(3.24935200511918,-1.,-1.88407708646357));
#60675=CARTESIAN_POINT('Ctrl Pts',(3.24935200511918,1.,-1.88407708646357));
#60676=CARTESIAN_POINT('Ctrl Pts',(3.24600543790443,-1.,-1.88229202582941));
#60677=CARTESIAN_POINT('Ctrl Pts',(3.24600543790443,1.,-1.88229202582941));
#60678=CARTESIAN_POINT('Ctrl Pts',(3.24451807186481,-1.,-1.88139187908074));
#60679=CARTESIAN_POINT('Ctrl Pts',(3.24451807186481,1.,-1.88139187908074));
#60680=CARTESIAN_POINT('Ctrl Pts',(3.24408699284121,-1.,-1.88102201872555));
#60681=CARTESIAN_POINT('Ctrl Pts',(3.24408699284121,1.,-1.88102201872555));
#60682=CARTESIAN_POINT('Ctrl Pts',(3.24410359189609,-1.,-1.88091100680349));
#60683=CARTESIAN_POINT('Ctrl Pts',(3.24410359189609,1.,-1.88091100680349));
#60684=CARTESIAN_POINT('Ctrl Pts',(3.24418789321065,-1.,-1.8808893942881));
#60685=CARTESIAN_POINT('Ctrl Pts',(3.24418789321065,1.,-1.8808893942881));
#60686=CARTESIAN_POINT('',(3.70708211654725,1.,-1.97421938526992));
#60687=CARTESIAN_POINT('Ctrl Pts',(3.70708211654725,1.,-1.97421938526992));
#60688=CARTESIAN_POINT('Ctrl Pts',(3.70551008132332,1.,-1.97417727645308));
#60689=CARTESIAN_POINT('Ctrl Pts',(3.70236698912904,1.,-1.97408973726715));
#60690=CARTESIAN_POINT('Ctrl Pts',(3.6976552856004,1.,-1.97394846383216));
#60691=CARTESIAN_POINT('Ctrl Pts',(3.69137888599902,1.,-1.97374016225483));
#60692=CARTESIAN_POINT('Ctrl Pts',(3.68354319915092,1.,-1.97344650304519));
#60693=CARTESIAN_POINT('Ctrl Pts',(3.67571738107084,1.,-1.97311947678517));
#60694=CARTESIAN_POINT('Ctrl Pts',(3.66790152752075,1.,-1.97275897198678));
#60695=CARTESIAN_POINT('Ctrl Pts',(3.6600957816636,1.,-1.9723648543905));
#60696=CARTESIAN_POINT('Ctrl Pts',(3.652300347166,1.,-1.9719369724024));
#60697=CARTESIAN_POINT('Ctrl Pts',(3.64451546723514,1.,-1.97147515441164));
#60698=CARTESIAN_POINT('Ctrl Pts',(3.63674139590412,1.,-1.97097920454464));
#60699=CARTESIAN_POINT('Ctrl Pts',(3.62897836973293,1.,-1.97044889850463));
#60700=CARTESIAN_POINT('Ctrl Pts',(3.62122658401893,1.,-1.96988398129978));
#60701=CARTESIAN_POINT('Ctrl Pts',(3.61348615496704,1.,-1.96928416040877));
#60702=CARTESIAN_POINT('Ctrl Pts',(3.60575714017989,1.,-1.9686491188594));
#60703=CARTESIAN_POINT('Ctrl Pts',(3.59803959819938,1.,-1.96797854118369));
#60704=CARTESIAN_POINT('Ctrl Pts',(3.59033364022801,1.,-1.96727213799544));
#60705=CARTESIAN_POINT('Ctrl Pts',(3.58263947663829,1.,-1.96652966688911));
#60706=CARTESIAN_POINT('Ctrl Pts',(3.57495748600959,1.,-1.96575096652789));
#60707=CARTESIAN_POINT('Ctrl Pts',(3.56728820357791,1.,-1.96493594634567));
#60708=CARTESIAN_POINT('Ctrl Pts',(3.55963218706096,1.,-1.96408450906812));
#60709=CARTESIAN_POINT('Ctrl Pts',(3.55198990600886,1.,-1.96319648628644));
#60710=CARTESIAN_POINT('Ctrl Pts',(3.54436163300443,1.,-1.96227157573067));
#60711=CARTESIAN_POINT('Ctrl Pts',(3.53674730625813,1.,-1.96130926212689));
#60712=CARTESIAN_POINT('Ctrl Pts',(3.52914648844351,1.,-1.96030879411566));
#60713=CARTESIAN_POINT('Ctrl Pts',(3.52155867431486,1.,-1.95926936324461));
#60714=CARTESIAN_POINT('Ctrl Pts',(3.51398354617794,1.,-1.95819025316779));
#60715=CARTESIAN_POINT('Ctrl Pts',(3.50642124159909,1.,-1.95707099606511));
#60716=CARTESIAN_POINT('Ctrl Pts',(3.49887263575583,1.,-1.95591153823661));
#60717=CARTESIAN_POINT('Ctrl Pts',(3.49133956289133,1.,-1.95471236969643));
#60718=CARTESIAN_POINT('Ctrl Pts',(3.48382414832634,1.,-1.95347412486309));
#60719=CARTESIAN_POINT('Ctrl Pts',(3.47632820495921,1.,-1.95219722189876));
#60720=CARTESIAN_POINT('Ctrl Pts',(3.46885258974191,1.,-1.95088147859877));
#60721=CARTESIAN_POINT('Ctrl Pts',(3.46139661060962,1.,-1.94952575850197));
#60722=CARTESIAN_POINT('Ctrl Pts',(3.45395731584051,1.,-1.94812754766524));
#60723=CARTESIAN_POINT('Ctrl Pts',(3.44653088665681,1.,-1.94668377715329));
#60724=CARTESIAN_POINT('Ctrl Pts',(3.43911410197687,1.,-1.94519168842879));
#60725=CARTESIAN_POINT('Ctrl Pts',(3.43170586602434,1.,-1.94364973660284));
#60726=CARTESIAN_POINT('Ctrl Pts',(3.42430850941503,1.,-1.94205835913696));
#60727=CARTESIAN_POINT('Ctrl Pts',(3.41692971994096,1.,-1.94042111965246));
#60728=CARTESIAN_POINT('Ctrl Pts',(3.40957978266642,1.,-1.93874306008143));
#60729=CARTESIAN_POINT('Ctrl Pts',(3.40226802104109,1.,-1.93702857723098));
#60730=CARTESIAN_POINT('Ctrl Pts',(3.39499923640795,1.,-1.93527929945985));
#60731=CARTESIAN_POINT('Ctrl Pts',(3.38777076883256,1.,-1.93349233176788));
#60732=CARTESIAN_POINT('Ctrl Pts',(3.3805676852555,1.,-1.93165739093276));
#60733=CARTESIAN_POINT('Ctrl Pts',(3.37336807068043,1.,-1.92975993109877));
#60734=CARTESIAN_POINT('Ctrl Pts',(3.36615168657567,1.,-1.92778626543786));
#60735=CARTESIAN_POINT('Ctrl Pts',(3.35890824422965,1.,-1.92572846125756));
#60736=CARTESIAN_POINT('Ctrl Pts',(3.35164424847223,1.,-1.92358838440528));
#60737=CARTESIAN_POINT('Ctrl Pts',(3.34439448941961,1.,-1.92138450828404));
#60738=CARTESIAN_POINT('Ctrl Pts',(3.33721230710012,1.,-1.9191460961021));
#60739=CARTESIAN_POINT('Ctrl Pts',(3.33014884257873,1.,-1.91690081930332));
#60740=CARTESIAN_POINT('Ctrl Pts',(3.32323403454535,1.,-1.91466343916628));
#60741=CARTESIAN_POINT('Ctrl Pts',(3.31646052426364,1.,-1.91242616234442));
#60742=CARTESIAN_POINT('Ctrl Pts',(3.30975721158596,1.,-1.91014297830446));
#60743=CARTESIAN_POINT('Ctrl Pts',(3.30300595568195,1.,-1.90773912171341));
#60744=CARTESIAN_POINT('Ctrl Pts',(3.29608978722113,1.,-1.90513891864087));
#60745=CARTESIAN_POINT('Ctrl Pts',(3.2889344860029,1.,-1.90228971247527));
#60746=CARTESIAN_POINT('Ctrl Pts',(3.28154737912352,1.,-1.89918429230462));
#60747=CARTESIAN_POINT('Ctrl Pts',(3.27407108933139,1.,-1.89589172903793));
#60748=CARTESIAN_POINT('Ctrl Pts',(3.26677653888676,1.,-1.89255393500965));
#60749=CARTESIAN_POINT('Ctrl Pts',(3.25999885193947,1.,-1.88934996203698));
#60750=CARTESIAN_POINT('Ctrl Pts',(3.25408686339463,1.,-1.88646802523466));
#60751=CARTESIAN_POINT('Ctrl Pts',(3.24935200511918,1.,-1.88407708646357));
#60752=CARTESIAN_POINT('Ctrl Pts',(3.2462565441079,1.,-1.88242596600454));
#60753=CARTESIAN_POINT('Ctrl Pts',(3.24480754676064,1.,-1.88156537699203));
#60754=CARTESIAN_POINT('Ctrl Pts',(3.24428080353022,1.,-1.88117508446775));
#60755=CARTESIAN_POINT('Ctrl Pts',(3.24415531671284,1.,-1.8810229239812));
#60756=CARTESIAN_POINT('Ctrl Pts',(3.24413672884812,1.,-1.88097764062697));
#60757=CARTESIAN_POINT('',(3.70708211654725,0.,-1.97421938526992));
#60758=CARTESIAN_POINT('Ctrl Pts',(3.42855728381368,-1.,-1.519044091397));
#60759=CARTESIAN_POINT('Ctrl Pts',(3.42855728381368,1.,-1.519044091397));
#60760=CARTESIAN_POINT('Ctrl Pts',(3.42852521763778,-1.,-1.51896318668366));
#60761=CARTESIAN_POINT('Ctrl Pts',(3.42852521763778,1.,-1.51896318668366));
#60762=CARTESIAN_POINT('Ctrl Pts',(3.42860527149177,-1.,-1.51888450659652));
#60763=CARTESIAN_POINT('Ctrl Pts',(3.42860527149177,1.,-1.51888450659652));
#60764=CARTESIAN_POINT('Ctrl Pts',(3.42915787669893,-1.,-1.51901585839109));
#60765=CARTESIAN_POINT('Ctrl Pts',(3.42915787669893,1.,-1.51901585839109));
#60766=CARTESIAN_POINT('Ctrl Pts',(3.43076036253837,-1.,-1.51969006980999));
#60767=CARTESIAN_POINT('Ctrl Pts',(3.43076036253837,1.,-1.51969006980999));
#60768=CARTESIAN_POINT('Ctrl Pts',(3.43417156977893,-1.,-1.52134826724293));
#60769=CARTESIAN_POINT('Ctrl Pts',(3.43417156977893,1.,-1.52134826724293));
#60770=CARTESIAN_POINT('Ctrl Pts',(3.4388889597401,-1.,-1.5237734895035));
#60771=CARTESIAN_POINT('Ctrl Pts',(3.4388889597401,1.,-1.5237734895035));
#60772=CARTESIAN_POINT('Ctrl Pts',(3.44469547526647,-1.,-1.52686242875556));
#60773=CARTESIAN_POINT('Ctrl Pts',(3.44469547526647,1.,-1.52686242875556));
#60774=CARTESIAN_POINT('Ctrl Pts',(3.45127136828305,-1.,-1.53046244461635));
#60775=CARTESIAN_POINT('Ctrl Pts',(3.45127136828305,1.,-1.53046244461635));
#60776=CARTESIAN_POINT('Ctrl Pts',(3.45825932955032,-1.,-1.53440195378792));
#60777=CARTESIAN_POINT('Ctrl Pts',(3.45825932955032,1.,-1.53440195378792));
#60778=CARTESIAN_POINT('Ctrl Pts',(3.46531752207153,-1.,-1.53851507915502));
#60779=CARTESIAN_POINT('Ctrl Pts',(3.46531752207153,1.,-1.53851507915502));
#60780=CARTESIAN_POINT('Ctrl Pts',(3.47217189224653,-1.,-1.54266605398188));
#60781=CARTESIAN_POINT('Ctrl Pts',(3.47217189224653,1.,-1.54266605398188));
#60782=CARTESIAN_POINT('Ctrl Pts',(3.47868272898751,-1.,-1.54678009290276));
#60783=CARTESIAN_POINT('Ctrl Pts',(3.47868272898751,1.,-1.54678009290276));
#60784=CARTESIAN_POINT('Ctrl Pts',(3.48485155928567,-1.,-1.55084702970452));
#60785=CARTESIAN_POINT('Ctrl Pts',(3.48485155928567,1.,-1.55084702970452));
#60786=CARTESIAN_POINT('Ctrl Pts',(3.4907646087742,-1.,-1.55489595901116));
#60787=CARTESIAN_POINT('Ctrl Pts',(3.4907646087742,1.,-1.55489595901116));
#60788=CARTESIAN_POINT('Ctrl Pts',(3.49655185179655,-1.,-1.55897703097874));
#60789=CARTESIAN_POINT('Ctrl Pts',(3.49655185179655,1.,-1.55897703097874));
#60790=CARTESIAN_POINT('Ctrl Pts',(3.50234321621578,-1.,-1.56314187758675));
#60791=CARTESIAN_POINT('Ctrl Pts',(3.50234321621578,1.,-1.56314187758675));
#60792=CARTESIAN_POINT('Ctrl Pts',(3.50821771695363,-1.,-1.56742097575012));
#60793=CARTESIAN_POINT('Ctrl Pts',(3.50821771695363,1.,-1.56742097575012));
#60794=CARTESIAN_POINT('Ctrl Pts',(3.51418598431665,-1.,-1.57181569799743));
#60795=CARTESIAN_POINT('Ctrl Pts',(3.51418598431665,1.,-1.57181569799743));
#60796=CARTESIAN_POINT('Ctrl Pts',(3.52021847865912,-1.,-1.57631049988158));
#60797=CARTESIAN_POINT('Ctrl Pts',(3.52021847865912,1.,-1.57631049988158));
#60798=CARTESIAN_POINT('Ctrl Pts',(3.52626275334881,-1.,-1.58088027227848));
#60799=CARTESIAN_POINT('Ctrl Pts',(3.52626275334881,1.,-1.58088027227848));
#60800=CARTESIAN_POINT('Ctrl Pts',(3.5322637814708,-1.,-1.58549906268088));
#60801=CARTESIAN_POINT('Ctrl Pts',(3.5322637814708,1.,-1.58549906268088));
#60802=CARTESIAN_POINT('Ctrl Pts',(3.53818616861077,-1.,-1.59014958368739));
#60803=CARTESIAN_POINT('Ctrl Pts',(3.53818616861077,1.,-1.59014958368739));
#60804=CARTESIAN_POINT('Ctrl Pts',(3.54402458182337,-1.,-1.59482766949766));
#60805=CARTESIAN_POINT('Ctrl Pts',(3.54402458182337,1.,-1.59482766949766));
#60806=CARTESIAN_POINT('Ctrl Pts',(3.54979148634454,-1.,-1.59953698113457));
#60807=CARTESIAN_POINT('Ctrl Pts',(3.54979148634454,1.,-1.59953698113457));
#60808=CARTESIAN_POINT('Ctrl Pts',(3.55550985096129,-1.,-1.60428584699853));
#60809=CARTESIAN_POINT('Ctrl Pts',(3.55550985096129,1.,-1.60428584699853));
#60810=CARTESIAN_POINT('Ctrl Pts',(3.5612043248298,-1.,-1.60908344685457));
#60811=CARTESIAN_POINT('Ctrl Pts',(3.5612043248298,1.,-1.60908344685457));
#60812=CARTESIAN_POINT('Ctrl Pts',(3.56689200468387,-1.,-1.61393581747514));
#60813=CARTESIAN_POINT('Ctrl Pts',(3.56689200468387,1.,-1.61393581747514));
#60814=CARTESIAN_POINT('Ctrl Pts',(3.57257679609806,-1.,-1.61884340915404));
#60815=CARTESIAN_POINT('Ctrl Pts',(3.57257679609806,1.,-1.61884340915404));
#60816=CARTESIAN_POINT('Ctrl Pts',(3.5782545595439,-1.,-1.62380329464844));
#60817=CARTESIAN_POINT('Ctrl Pts',(3.5782545595439,1.,-1.62380329464844));
#60818=CARTESIAN_POINT('Ctrl Pts',(3.58391625774343,-1.,-1.62881051550745));
#60819=CARTESIAN_POINT('Ctrl Pts',(3.58391625774343,1.,-1.62881051550745));
#60820=CARTESIAN_POINT('Ctrl Pts',(3.58955176627879,-1.,-1.6338597145126));
#60821=CARTESIAN_POINT('Ctrl Pts',(3.58955176627879,1.,-1.6338597145126));
#60822=CARTESIAN_POINT('Ctrl Pts',(3.59515368334893,-1.,-1.63894676675352));
#60823=CARTESIAN_POINT('Ctrl Pts',(3.59515368334893,1.,-1.63894676675352));
#60824=CARTESIAN_POINT('Ctrl Pts',(3.60072028513845,-1.,-1.64407004385582));
#60825=CARTESIAN_POINT('Ctrl Pts',(3.60072028513845,1.,-1.64407004385582));
#60826=CARTESIAN_POINT('Ctrl Pts',(3.60625346556992,-1.,-1.64922952425832));
#60827=CARTESIAN_POINT('Ctrl Pts',(3.60625346556992,1.,-1.64922952425832));
#60828=CARTESIAN_POINT('Ctrl Pts',(3.61175734965127,-1.,-1.65442619244325));
#60829=CARTESIAN_POINT('Ctrl Pts',(3.61175734965127,1.,-1.65442619244325));
#60830=CARTESIAN_POINT('Ctrl Pts',(3.61723666482456,-1.,-1.65966133399186));
#60831=CARTESIAN_POINT('Ctrl Pts',(3.61723666482456,1.,-1.65966133399186));
#60832=CARTESIAN_POINT('Ctrl Pts',(3.62269517989109,-1.,-1.66493585923855));
#60833=CARTESIAN_POINT('Ctrl Pts',(3.62269517989109,1.,-1.66493585923855));
#60834=CARTESIAN_POINT('Ctrl Pts',(3.62813422105271,-1.,-1.67024966008045));
#60835=CARTESIAN_POINT('Ctrl Pts',(3.62813422105271,1.,-1.67024966008045));
#60836=CARTESIAN_POINT('Ctrl Pts',(3.63355343201232,-1.,-1.67560193613156));
#60837=CARTESIAN_POINT('Ctrl Pts',(3.63355343201232,1.,-1.67560193613156));
#60838=CARTESIAN_POINT('Ctrl Pts',(3.63895140887462,-1.,-1.68099146651586));
#60839=CARTESIAN_POINT('Ctrl Pts',(3.63895140887462,1.,-1.68099146651586));
#60840=CARTESIAN_POINT('Ctrl Pts',(3.64432638915203,-1.,-1.68641690471457));
#60841=CARTESIAN_POINT('Ctrl Pts',(3.64432638915203,1.,-1.68641690471457));
#60842=CARTESIAN_POINT('Ctrl Pts',(3.64967689827371,-1.,-1.69187705481689));
#60843=CARTESIAN_POINT('Ctrl Pts',(3.64967689827371,1.,-1.69187705481689));
#60844=CARTESIAN_POINT('Ctrl Pts',(3.65500246526749,-1.,-1.69737117722534));
#60845=CARTESIAN_POINT('Ctrl Pts',(3.65500246526749,1.,-1.69737117722534));
#60846=CARTESIAN_POINT('Ctrl Pts',(3.66030338774847,-1.,-1.70289888566873));
#60847=CARTESIAN_POINT('Ctrl Pts',(3.66030338774847,1.,-1.70289888566873));
#60848=CARTESIAN_POINT('Ctrl Pts',(3.66558043198876,-1.,-1.70846001610956));
#60849=CARTESIAN_POINT('Ctrl Pts',(3.66558043198876,1.,-1.70846001610956));
#60850=CARTESIAN_POINT('Ctrl Pts',(3.67083454901611,-1.,-1.71405450210384));
#60851=CARTESIAN_POINT('Ctrl Pts',(3.67083454901611,1.,-1.71405450210384));
#60852=CARTESIAN_POINT('Ctrl Pts',(3.67606660374709,-1.,-1.71968225581808));
#60853=CARTESIAN_POINT('Ctrl Pts',(3.67606660374709,1.,-1.71968225581808));
#60854=CARTESIAN_POINT('Ctrl Pts',(3.68127704936579,-1.,-1.72534302437056));
#60855=CARTESIAN_POINT('Ctrl Pts',(3.68127704936579,1.,-1.72534302437056));
#60856=CARTESIAN_POINT('Ctrl Pts',(3.68646597019332,-1.,-1.73103640956717));
#60857=CARTESIAN_POINT('Ctrl Pts',(3.68646597019332,1.,-1.73103640956717));
#60858=CARTESIAN_POINT('Ctrl Pts',(3.69163322648036,-1.,-1.73676193254557));
#60859=CARTESIAN_POINT('Ctrl Pts',(3.69163322648036,1.,-1.73676193254557));
#60860=CARTESIAN_POINT('Ctrl Pts',(3.69677856910517,-1.,-1.74251908492617));
#60861=CARTESIAN_POINT('Ctrl Pts',(3.69677856910517,1.,-1.74251908492617));
#60862=CARTESIAN_POINT('Ctrl Pts',(3.7019017567335,-1.,-1.74830738046057));
#60863=CARTESIAN_POINT('Ctrl Pts',(3.7019017567335,1.,-1.74830738046057));
#60864=CARTESIAN_POINT('Ctrl Pts',(3.70700269736659,-1.,-1.75412641804042));
#60865=CARTESIAN_POINT('Ctrl Pts',(3.70700269736659,1.,-1.75412641804042));
#60866=CARTESIAN_POINT('Ctrl Pts',(3.71208146346136,-1.,-1.75997588498865));
#60867=CARTESIAN_POINT('Ctrl Pts',(3.71208146346136,1.,-1.75997588498865));
#60868=CARTESIAN_POINT('Ctrl Pts',(3.71713822377359,-1.,-1.76585552124394));
#60869=CARTESIAN_POINT('Ctrl Pts',(3.71713822377359,1.,-1.76585552124394));
#60870=CARTESIAN_POINT('Ctrl Pts',(3.72217319911254,-1.,-1.77176509401761));
#60871=CARTESIAN_POINT('Ctrl Pts',(3.72217319911254,1.,-1.77176509401761));
#60872=CARTESIAN_POINT('Ctrl Pts',(3.72718661205609,-1.,-1.77770437039658));
#60873=CARTESIAN_POINT('Ctrl Pts',(3.72718661205609,1.,-1.77770437039658));
#60874=CARTESIAN_POINT('Ctrl Pts',(3.7321786309547,-1.,-1.78367308442901));
#60875=CARTESIAN_POINT('Ctrl Pts',(3.7321786309547,1.,-1.78367308442901));
#60876=CARTESIAN_POINT('Ctrl Pts',(3.73714934730681,-1.,-1.78967092823491));
#60877=CARTESIAN_POINT('Ctrl Pts',(3.73714934730681,1.,-1.78967092823491));
#60878=CARTESIAN_POINT('Ctrl Pts',(3.74209880352445,-1.,-1.79569757859422));
#60879=CARTESIAN_POINT('Ctrl Pts',(3.74209880352445,1.,-1.79569757859422));
#60880=CARTESIAN_POINT('Ctrl Pts',(3.74702700875467,-1.,-1.8017527148577));
#60881=CARTESIAN_POINT('Ctrl Pts',(3.74702700875467,1.,-1.8017527148577));
#60882=CARTESIAN_POINT('Ctrl Pts',(3.75193395887977,-1.,-1.80783603939617));
#60883=CARTESIAN_POINT('Ctrl Pts',(3.75193395887977,1.,-1.80783603939617));
#60884=CARTESIAN_POINT('Ctrl Pts',(3.75681965683071,-1.,-1.8139472983358));
#60885=CARTESIAN_POINT('Ctrl Pts',(3.75681965683071,1.,-1.8139472983358));
#60886=CARTESIAN_POINT('Ctrl Pts',(3.76168412707948,-1.,-1.82008629694091));
#60887=CARTESIAN_POINT('Ctrl Pts',(3.76168412707948,1.,-1.82008629694091));
#60888=CARTESIAN_POINT('Ctrl Pts',(3.76652740353775,-1.,-1.82625289220915));
#60889=CARTESIAN_POINT('Ctrl Pts',(3.76652740353775,1.,-1.82625289220915));
#60890=CARTESIAN_POINT('Ctrl Pts',(3.77038509817999,-1.,-1.83120816955646));
#60891=CARTESIAN_POINT('Ctrl Pts',(3.77038509817999,1.,-1.83120816955646));
#60892=CARTESIAN_POINT('Ctrl Pts',(3.77326886064398,-1.,-1.83493697934534));
#60893=CARTESIAN_POINT('Ctrl Pts',(3.77326886064398,1.,-1.83493697934534));
#60894=CARTESIAN_POINT('Ctrl Pts',(3.77518714457833,-1.,-1.83742834010626));
#60895=CARTESIAN_POINT('Ctrl Pts',(3.77518714457833,1.,-1.83742834010626));
#60896=CARTESIAN_POINT('Ctrl Pts',(3.77614523045147,-1.,-1.83867539237861));
#60897=CARTESIAN_POINT('Ctrl Pts',(3.77614523045147,1.,-1.83867539237861));
#60898=CARTESIAN_POINT('',(3.42859860294306,1.,-1.5189508286633));
#60899=CARTESIAN_POINT('Ctrl Pts',(3.42859860294306,-1.,-1.5189508286633));
#60900=CARTESIAN_POINT('Ctrl Pts',(3.42859860294306,-0.666666666666667,
-1.5189508286633));
#60901=CARTESIAN_POINT('Ctrl Pts',(3.42859860294306,-0.333333333333333,
-1.5189508286633));
#60902=CARTESIAN_POINT('Ctrl Pts',(3.42859860294306,0.333333333333333,-1.5189508286633));
#60903=CARTESIAN_POINT('Ctrl Pts',(3.42859860294306,0.666666666666667,-1.5189508286633));
#60904=CARTESIAN_POINT('Ctrl Pts',(3.42859860294306,1.,-1.5189508286633));
#60905=CARTESIAN_POINT('',(3.77614523045147,1.,-1.83867539237861));
#60906=CARTESIAN_POINT('',(3.77614523045147,0.,-1.83867539237861));
#60907=CARTESIAN_POINT('Ctrl Pts',(3.42859860294306,1.,-1.5189508286633));
#60908=CARTESIAN_POINT('Ctrl Pts',(3.42864616361875,1.,-1.51893924967331));
#60909=CARTESIAN_POINT('Ctrl Pts',(3.42884302333841,1.,-1.5189513329503));
#60910=CARTESIAN_POINT('Ctrl Pts',(3.42946838852588,1.,-1.51914806898491));
#60911=CARTESIAN_POINT('Ctrl Pts',(3.43101631893414,1.,-1.5198144909338));
#60912=CARTESIAN_POINT('Ctrl Pts',(3.43417156977893,1.,-1.52134826724293));
#60913=CARTESIAN_POINT('Ctrl Pts',(3.4388889597401,1.,-1.5237734895035));
#60914=CARTESIAN_POINT('Ctrl Pts',(3.44469547526647,1.,-1.52686242875556));
#60915=CARTESIAN_POINT('Ctrl Pts',(3.45127136828305,1.,-1.53046244461635));
#60916=CARTESIAN_POINT('Ctrl Pts',(3.45825932955032,1.,-1.53440195378792));
#60917=CARTESIAN_POINT('Ctrl Pts',(3.46531752207153,1.,-1.53851507915502));
#60918=CARTESIAN_POINT('Ctrl Pts',(3.47217189224653,1.,-1.54266605398188));
#60919=CARTESIAN_POINT('Ctrl Pts',(3.47868272898751,1.,-1.54678009290276));
#60920=CARTESIAN_POINT('Ctrl Pts',(3.48485155928567,1.,-1.55084702970452));
#60921=CARTESIAN_POINT('Ctrl Pts',(3.4907646087742,1.,-1.55489595901116));
#60922=CARTESIAN_POINT('Ctrl Pts',(3.49655185179655,1.,-1.55897703097874));
#60923=CARTESIAN_POINT('Ctrl Pts',(3.50234321621578,1.,-1.56314187758675));
#60924=CARTESIAN_POINT('Ctrl Pts',(3.50821771695363,1.,-1.56742097575012));
#60925=CARTESIAN_POINT('Ctrl Pts',(3.51418598431665,1.,-1.57181569799743));
#60926=CARTESIAN_POINT('Ctrl Pts',(3.52021847865912,1.,-1.57631049988158));
#60927=CARTESIAN_POINT('Ctrl Pts',(3.52626275334881,1.,-1.58088027227848));
#60928=CARTESIAN_POINT('Ctrl Pts',(3.5322637814708,1.,-1.58549906268088));
#60929=CARTESIAN_POINT('Ctrl Pts',(3.53818616861077,1.,-1.59014958368739));
#60930=CARTESIAN_POINT('Ctrl Pts',(3.54402458182337,1.,-1.59482766949766));
#60931=CARTESIAN_POINT('Ctrl Pts',(3.54979148634454,1.,-1.59953698113457));
#60932=CARTESIAN_POINT('Ctrl Pts',(3.55550985096129,1.,-1.60428584699853));
#60933=CARTESIAN_POINT('Ctrl Pts',(3.5612043248298,1.,-1.60908344685457));
#60934=CARTESIAN_POINT('Ctrl Pts',(3.56689200468387,1.,-1.61393581747514));
#60935=CARTESIAN_POINT('Ctrl Pts',(3.57257679609806,1.,-1.61884340915404));
#60936=CARTESIAN_POINT('Ctrl Pts',(3.5782545595439,1.,-1.62380329464844));
#60937=CARTESIAN_POINT('Ctrl Pts',(3.58391625774343,1.,-1.62881051550745));
#60938=CARTESIAN_POINT('Ctrl Pts',(3.58955176627879,1.,-1.6338597145126));
#60939=CARTESIAN_POINT('Ctrl Pts',(3.59515368334893,1.,-1.63894676675352));
#60940=CARTESIAN_POINT('Ctrl Pts',(3.60072028513845,1.,-1.64407004385582));
#60941=CARTESIAN_POINT('Ctrl Pts',(3.60625346556992,1.,-1.64922952425832));
#60942=CARTESIAN_POINT('Ctrl Pts',(3.61175734965127,1.,-1.65442619244325));
#60943=CARTESIAN_POINT('Ctrl Pts',(3.61723666482456,1.,-1.65966133399186));
#60944=CARTESIAN_POINT('Ctrl Pts',(3.62269517989109,1.,-1.66493585923855));
#60945=CARTESIAN_POINT('Ctrl Pts',(3.62813422105271,1.,-1.67024966008045));
#60946=CARTESIAN_POINT('Ctrl Pts',(3.63355343201232,1.,-1.67560193613156));
#60947=CARTESIAN_POINT('Ctrl Pts',(3.63895140887462,1.,-1.68099146651586));
#60948=CARTESIAN_POINT('Ctrl Pts',(3.64432638915203,1.,-1.68641690471457));
#60949=CARTESIAN_POINT('Ctrl Pts',(3.64967689827371,1.,-1.69187705481689));
#60950=CARTESIAN_POINT('Ctrl Pts',(3.65500246526749,1.,-1.69737117722534));
#60951=CARTESIAN_POINT('Ctrl Pts',(3.66030338774847,1.,-1.70289888566873));
#60952=CARTESIAN_POINT('Ctrl Pts',(3.66558043198876,1.,-1.70846001610956));
#60953=CARTESIAN_POINT('Ctrl Pts',(3.67083454901611,1.,-1.71405450210384));
#60954=CARTESIAN_POINT('Ctrl Pts',(3.67606660374709,1.,-1.71968225581808));
#60955=CARTESIAN_POINT('Ctrl Pts',(3.68127704936579,1.,-1.72534302437056));
#60956=CARTESIAN_POINT('Ctrl Pts',(3.68646597019332,1.,-1.73103640956717));
#60957=CARTESIAN_POINT('Ctrl Pts',(3.69163322648036,1.,-1.73676193254557));
#60958=CARTESIAN_POINT('Ctrl Pts',(3.69677856910517,1.,-1.74251908492617));
#60959=CARTESIAN_POINT('Ctrl Pts',(3.7019017567335,1.,-1.74830738046057));
#60960=CARTESIAN_POINT('Ctrl Pts',(3.70700269736659,1.,-1.75412641804042));
#60961=CARTESIAN_POINT('Ctrl Pts',(3.71208146346136,1.,-1.75997588498865));
#60962=CARTESIAN_POINT('Ctrl Pts',(3.71713822377359,1.,-1.76585552124394));
#60963=CARTESIAN_POINT('Ctrl Pts',(3.72217319911254,1.,-1.77176509401761));
#60964=CARTESIAN_POINT('Ctrl Pts',(3.72718661205609,1.,-1.77770437039658));
#60965=CARTESIAN_POINT('Ctrl Pts',(3.7321786309547,1.,-1.78367308442901));
#60966=CARTESIAN_POINT('Ctrl Pts',(3.73714934730681,1.,-1.78967092823491));
#60967=CARTESIAN_POINT('Ctrl Pts',(3.74209880352445,1.,-1.79569757859422));
#60968=CARTESIAN_POINT('Ctrl Pts',(3.74702700875467,1.,-1.8017527148577));
#60969=CARTESIAN_POINT('Ctrl Pts',(3.75193395887977,1.,-1.80783603939617));
#60970=CARTESIAN_POINT('Ctrl Pts',(3.75681965683071,1.,-1.8139472983358));
#60971=CARTESIAN_POINT('Ctrl Pts',(3.76168412707948,1.,-1.82008629694091));
#60972=CARTESIAN_POINT('Ctrl Pts',(3.76652740353775,1.,-1.82625289220915));
#60973=CARTESIAN_POINT('Ctrl Pts',(3.77038509817999,1.,-1.83120816955646));
#60974=CARTESIAN_POINT('Ctrl Pts',(3.77326886064398,1.,-1.83493697934534));
#60975=CARTESIAN_POINT('Ctrl Pts',(3.77518714457833,1.,-1.83742834010626));
#60976=CARTESIAN_POINT('Ctrl Pts',(3.77614523045147,1.,-1.83867539237861));
#60977=CARTESIAN_POINT('Origin',(3.77614523045147,0.,-1.83867539237861));
#60978=CARTESIAN_POINT('',(3.70708211654725,1.,-1.97421938526992));
#60979=CARTESIAN_POINT('Origin',(0.,0.,0.));
#60980=CARTESIAN_POINT('',(3.49844575334386,1.,-1.35032489087269));
#60981=CARTESIAN_POINT('Origin',(0.,1.,0.));
#60982=CARTESIAN_POINT('Ctrl Pts',(3.49844575334386,1.,-1.35032489087269));
#60983=CARTESIAN_POINT('Ctrl Pts',(3.49844575334386,0.666666666666667,-1.35032489087269));
#60984=CARTESIAN_POINT('Ctrl Pts',(3.49844575334386,0.333333333333333,-1.35032489087269));
#60985=CARTESIAN_POINT('Ctrl Pts',(3.49844575334386,-0.333333333333333,
-1.35032489087269));
#60986=CARTESIAN_POINT('Ctrl Pts',(3.49844575334386,-0.666666666666667,
-1.35032489087269));
#60987=CARTESIAN_POINT('Ctrl Pts',(3.49844575334386,-1.,-1.35032489087269));
#60988=CARTESIAN_POINT('Ctrl Pts',(3.97027773754922,-1.,-1.36999806084572));
#60989=CARTESIAN_POINT('Ctrl Pts',(3.97027773754922,1.,-1.36999806084572));
#60990=CARTESIAN_POINT('Ctrl Pts',(3.9687184694173,-1.,-1.37020239094758));
#60991=CARTESIAN_POINT('Ctrl Pts',(3.9687184694173,1.,-1.37020239094758));
#60992=CARTESIAN_POINT('Ctrl Pts',(3.96560037975788,-1.,-1.37060761746027));
#60993=CARTESIAN_POINT('Ctrl Pts',(3.96560037975788,1.,-1.37060761746027));
#60994=CARTESIAN_POINT('Ctrl Pts',(3.96092458508407,-1.,-1.37120515615663));
#60995=CARTESIAN_POINT('Ctrl Pts',(3.96092458508407,1.,-1.37120515615663));
#60996=CARTESIAN_POINT('Ctrl Pts',(3.95469287283105,-1.,-1.37198126433139));
#60997=CARTESIAN_POINT('Ctrl Pts',(3.95469287283105,1.,-1.37198126433139));
#60998=CARTESIAN_POINT('Ctrl Pts',(3.94690771786926,-1.,-1.37291699203423));
#60999=CARTESIAN_POINT('Ctrl Pts',(3.94690771786926,1.,-1.37291699203423));
#61000=CARTESIAN_POINT('Ctrl Pts',(3.93912709041791,-1.,-1.37381821967499));
#61001=CARTESIAN_POINT('Ctrl Pts',(3.93912709041791,1.,-1.37381821967499));
#61002=CARTESIAN_POINT('Ctrl Pts',(3.93135106761941,-1.,-1.37468482215784));
#61003=CARTESIAN_POINT('Ctrl Pts',(3.93135106761941,1.,-1.37468482215784));
#61004=CARTESIAN_POINT('Ctrl Pts',(3.92357976987132,-1.,-1.37551664448057));
#61005=CARTESIAN_POINT('Ctrl Pts',(3.92357976987132,1.,-1.37551664448057));
#61006=CARTESIAN_POINT('Ctrl Pts',(3.91581337461825,-1.,-1.37631350505516));
#61007=CARTESIAN_POINT('Ctrl Pts',(3.91581337461825,1.,-1.37631350505516));
#61008=CARTESIAN_POINT('Ctrl Pts',(3.90805209522729,-1.,-1.3770751963376));
#61009=CARTESIAN_POINT('Ctrl Pts',(3.90805209522729,1.,-1.3770751963376));
#61010=CARTESIAN_POINT('Ctrl Pts',(3.90029615196255,-1.,-1.3778014851263));
#61011=CARTESIAN_POINT('Ctrl Pts',(3.90029615196255,1.,-1.3778014851263));
#61012=CARTESIAN_POINT('Ctrl Pts',(3.89254574338385,-1.,-1.37849211287981));
#61013=CARTESIAN_POINT('Ctrl Pts',(3.89254574338385,1.,-1.37849211287981));
#61014=CARTESIAN_POINT('Ctrl Pts',(3.88480102249461,-1.,-1.37914679719446));
#61015=CARTESIAN_POINT('Ctrl Pts',(3.88480102249461,1.,-1.37914679719446));
#61016=CARTESIAN_POINT('Ctrl Pts',(3.87706205830865,-1.,-1.37976523097187));
#61017=CARTESIAN_POINT('Ctrl Pts',(3.87706205830865,1.,-1.37976523097187));
#61018=CARTESIAN_POINT('Ctrl Pts',(3.86932885813403,-1.,-1.38034709213129));
#61019=CARTESIAN_POINT('Ctrl Pts',(3.86932885813403,1.,-1.38034709213129));
#61020=CARTESIAN_POINT('Ctrl Pts',(3.86160143044187,-1.,-1.38089205993068));
#61021=CARTESIAN_POINT('Ctrl Pts',(3.86160143044187,1.,-1.38089205993068));
#61022=CARTESIAN_POINT('Ctrl Pts',(3.85387983979557,-1.,-1.38139983115075));
#61023=CARTESIAN_POINT('Ctrl Pts',(3.85387983979557,1.,-1.38139983115075));
#61024=CARTESIAN_POINT('Ctrl Pts',(3.84616425605705,-1.,-1.38187013346089));
#61025=CARTESIAN_POINT('Ctrl Pts',(3.84616425605705,1.,-1.38187013346089));
#61026=CARTESIAN_POINT('Ctrl Pts',(3.83845502790609,-1.,-1.38230274828774));
#61027=CARTESIAN_POINT('Ctrl Pts',(3.83845502790609,1.,-1.38230274828774));
#61028=CARTESIAN_POINT('Ctrl Pts',(3.83075266982138,-1.,-1.38269750245086));
#61029=CARTESIAN_POINT('Ctrl Pts',(3.83075266982138,1.,-1.38269750245086));
#61030=CARTESIAN_POINT('Ctrl Pts',(3.82305771743715,-1.,-1.38305421262724));
#61031=CARTESIAN_POINT('Ctrl Pts',(3.82305771743715,1.,-1.38305421262724));
#61032=CARTESIAN_POINT('Ctrl Pts',(3.81537060817765,-1.,-1.38337263902766));
#61033=CARTESIAN_POINT('Ctrl Pts',(3.81537060817765,1.,-1.38337263902766));
#61034=CARTESIAN_POINT('Ctrl Pts',(3.80769156398429,-1.,-1.38365244046226));
#61035=CARTESIAN_POINT('Ctrl Pts',(3.80769156398429,1.,-1.38365244046226));
#61036=CARTESIAN_POINT('Ctrl Pts',(3.80002044322169,-1.,-1.38389311766701));
#61037=CARTESIAN_POINT('Ctrl Pts',(3.80002044322169,1.,-1.38389311766701));
#61038=CARTESIAN_POINT('Ctrl Pts',(3.79235669640907,-1.,-1.38409399694589));
#61039=CARTESIAN_POINT('Ctrl Pts',(3.79235669640907,1.,-1.38409399694589));
#61040=CARTESIAN_POINT('Ctrl Pts',(3.78469969805134,-1.,-1.38425435883773));
#61041=CARTESIAN_POINT('Ctrl Pts',(3.78469969805134,1.,-1.38425435883773));
#61042=CARTESIAN_POINT('Ctrl Pts',(3.77704902230441,-1.,-1.38437354551435));
#61043=CARTESIAN_POINT('Ctrl Pts',(3.77704902230441,1.,-1.38437354551435));
#61044=CARTESIAN_POINT('Ctrl Pts',(3.76940473185775,-1.,-1.38445107339517));
#61045=CARTESIAN_POINT('Ctrl Pts',(3.76940473185775,1.,-1.38445107339517));
#61046=CARTESIAN_POINT('Ctrl Pts',(3.76176768271347,-1.,-1.38448675253343));
#61047=CARTESIAN_POINT('Ctrl Pts',(3.76176768271347,1.,-1.38448675253343));
#61048=CARTESIAN_POINT('Ctrl Pts',(3.75413976318727,-1.,-1.38448077997155));
#61049=CARTESIAN_POINT('Ctrl Pts',(3.75413976318727,1.,-1.38448077997155));
#61050=CARTESIAN_POINT('Ctrl Pts',(3.7465231716786,-1.,-1.38443344984389));
#61051=CARTESIAN_POINT('Ctrl Pts',(3.7465231716786,1.,-1.38443344984389));
#61052=CARTESIAN_POINT('Ctrl Pts',(3.73891976418099,-1.,-1.38434489156456));
#61053=CARTESIAN_POINT('Ctrl Pts',(3.73891976418099,1.,-1.38434489156456));
#61054=CARTESIAN_POINT('Ctrl Pts',(3.73133035859283,-1.,-1.38421479111531));
#61055=CARTESIAN_POINT('Ctrl Pts',(3.73133035859283,1.,-1.38421479111531));
#61056=CARTESIAN_POINT('Ctrl Pts',(3.72375409358805,-1.,-1.3840421342895));
#61057=CARTESIAN_POINT('Ctrl Pts',(3.72375409358805,1.,-1.3840421342895));
#61058=CARTESIAN_POINT('Ctrl Pts',(3.7161876605181,-1.,-1.38382489984585));
#61059=CARTESIAN_POINT('Ctrl Pts',(3.7161876605181,1.,-1.38382489984585));
#61060=CARTESIAN_POINT('Ctrl Pts',(3.70862680753343,-1.,-1.38356065402122));
#61061=CARTESIAN_POINT('Ctrl Pts',(3.70862680753343,1.,-1.38356065402122));
#61062=CARTESIAN_POINT('Ctrl Pts',(3.70106792167894,-1.,-1.38324717612862));
#61063=CARTESIAN_POINT('Ctrl Pts',(3.70106792167894,1.,-1.38324717612862));
#61064=CARTESIAN_POINT('Ctrl Pts',(3.69350967899523,-1.,-1.38288311171649));
#61065=CARTESIAN_POINT('Ctrl Pts',(3.69350967899523,1.,-1.38288311171649));
#61066=CARTESIAN_POINT('Ctrl Pts',(3.68595444983844,-1.,-1.38246852827185));
#61067=CARTESIAN_POINT('Ctrl Pts',(3.68595444983844,1.,-1.38246852827185));
#61068=CARTESIAN_POINT('Ctrl Pts',(3.6784103848243,-1.,-1.38200574290626));
#61069=CARTESIAN_POINT('Ctrl Pts',(3.6784103848243,1.,-1.38200574290626));
#61070=CARTESIAN_POINT('Ctrl Pts',(3.67088843112282,-1.,-1.38149812653876));
#61071=CARTESIAN_POINT('Ctrl Pts',(3.67088843112282,1.,-1.38149812653876));
#61072=CARTESIAN_POINT('Ctrl Pts',(3.66339848520874,-1.,-1.38094856333558));
#61073=CARTESIAN_POINT('Ctrl Pts',(3.66339848520874,1.,-1.38094856333558));
#61074=CARTESIAN_POINT('Ctrl Pts',(3.65594554404396,-1.,-1.38035791051215));
#61075=CARTESIAN_POINT('Ctrl Pts',(3.65594554404396,1.,-1.38035791051215));
#61076=CARTESIAN_POINT('Ctrl Pts',(3.64852652756444,-1.,-1.37972372481598));
#61077=CARTESIAN_POINT('Ctrl Pts',(3.64852652756444,1.,-1.37972372481598));
#61078=CARTESIAN_POINT('Ctrl Pts',(3.64112507791112,-1.,-1.37903818567347));
#61079=CARTESIAN_POINT('Ctrl Pts',(3.64112507791112,1.,-1.37903818567347));
#61080=CARTESIAN_POINT('Ctrl Pts',(3.63371727442448,-1.,-1.37829035457325));
#61081=CARTESIAN_POINT('Ctrl Pts',(3.63371727442448,1.,-1.37829035457325));
#61082=CARTESIAN_POINT('Ctrl Pts',(3.62628098665112,-1.,-1.37746987919868));
#61083=CARTESIAN_POINT('Ctrl Pts',(3.62628098665112,1.,-1.37746987919868));
#61084=CARTESIAN_POINT('Ctrl Pts',(3.61880481160408,-1.,-1.37657053403102));
#61085=CARTESIAN_POINT('Ctrl Pts',(3.61880481160408,1.,-1.37657053403102));
#61086=CARTESIAN_POINT('Ctrl Pts',(3.61129546591082,-1.,-1.37559314436641));
#61087=CARTESIAN_POINT('Ctrl Pts',(3.61129546591082,1.,-1.37559314436641));
#61088=CARTESIAN_POINT('Ctrl Pts',(3.60379020124038,-1.,-1.37455051379642));
#61089=CARTESIAN_POINT('Ctrl Pts',(3.60379020124038,1.,-1.37455051379642));
#61090=CARTESIAN_POINT('Ctrl Pts',(3.59634627869117,-1.,-1.37346320103184));
#61091=CARTESIAN_POINT('Ctrl Pts',(3.59634627869117,1.,-1.37346320103184));
#61092=CARTESIAN_POINT('Ctrl Pts',(3.5890185384643,-1.,-1.37235053661));
#61093=CARTESIAN_POINT('Ctrl Pts',(3.5890185384643,1.,-1.37235053661));
#61094=CARTESIAN_POINT('Ctrl Pts',(3.58183885982745,-1.,-1.37122241663073));
#61095=CARTESIAN_POINT('Ctrl Pts',(3.58183885982745,1.,-1.37122241663073));
#61096=CARTESIAN_POINT('Ctrl Pts',(3.57479875549453,-1.,-1.37007229485646));
#61097=CARTESIAN_POINT('Ctrl Pts',(3.57479875549453,1.,-1.37007229485646));
#61098=CARTESIAN_POINT('Ctrl Pts',(3.56782080304554,-1.,-1.36886584973349));
#61099=CARTESIAN_POINT('Ctrl Pts',(3.56782080304554,1.,-1.36886584973349));
#61100=CARTESIAN_POINT('Ctrl Pts',(3.56077662028492,-1.,-1.36754771771174));
#61101=CARTESIAN_POINT('Ctrl Pts',(3.56077662028492,1.,-1.36754771771174));
#61102=CARTESIAN_POINT('Ctrl Pts',(3.55353883995793,-1.,-1.36606145456711));
#61103=CARTESIAN_POINT('Ctrl Pts',(3.55353883995793,1.,-1.36606145456711));
#61104=CARTESIAN_POINT('Ctrl Pts',(3.54602591832893,-1.,-1.36436666257568));
#61105=CARTESIAN_POINT('Ctrl Pts',(3.54602591832893,1.,-1.36436666257568));
#61106=CARTESIAN_POINT('Ctrl Pts',(3.53824396425032,-1.,-1.36245507339334));
#61107=CARTESIAN_POINT('Ctrl Pts',(3.53824396425032,1.,-1.36245507339334));
#61108=CARTESIAN_POINT('Ctrl Pts',(3.53034464961849,-1.,-1.36037259643827));
#61109=CARTESIAN_POINT('Ctrl Pts',(3.53034464961849,1.,-1.36037259643827));
#61110=CARTESIAN_POINT('Ctrl Pts',(3.52261776117121,-1.,-1.35821701528975));
#61111=CARTESIAN_POINT('Ctrl Pts',(3.52261776117121,1.,-1.35821701528975));
#61112=CARTESIAN_POINT('Ctrl Pts',(3.51542230699919,-1.,-1.35611275237288));
#61113=CARTESIAN_POINT('Ctrl Pts',(3.51542230699919,1.,-1.35611275237288));
#61114=CARTESIAN_POINT('Ctrl Pts',(3.50913227060177,-1.,-1.35419113576022));
#61115=CARTESIAN_POINT('Ctrl Pts',(3.50913227060177,1.,-1.35419113576022));
#61116=CARTESIAN_POINT('Ctrl Pts',(3.50408168106113,-1.,-1.3525703284343));
#61117=CARTESIAN_POINT('Ctrl Pts',(3.50408168106113,1.,-1.3525703284343));
#61118=CARTESIAN_POINT('Ctrl Pts',(3.50049707063673,-1.,-1.35133076331065));
#61119=CARTESIAN_POINT('Ctrl Pts',(3.50049707063673,1.,-1.35133076331065));
#61120=CARTESIAN_POINT('Ctrl Pts',(3.49888720256612,-1.,-1.35067437417289));
#61121=CARTESIAN_POINT('Ctrl Pts',(3.49888720256612,1.,-1.35067437417289));
#61122=CARTESIAN_POINT('Ctrl Pts',(3.49840357193384,-1.,-1.35037650302887));
#61123=CARTESIAN_POINT('Ctrl Pts',(3.49840357193384,1.,-1.35037650302887));
#61124=CARTESIAN_POINT('Ctrl Pts',(3.49840260053616,-1.,-1.35026426118352));
#61125=CARTESIAN_POINT('Ctrl Pts',(3.49840260053616,1.,-1.35026426118352));
#61126=CARTESIAN_POINT('Ctrl Pts',(3.49848248301936,-1.,-1.35022972712301));
#61127=CARTESIAN_POINT('Ctrl Pts',(3.49848248301936,1.,-1.35022972712301));
#61128=CARTESIAN_POINT('',(3.97027773754922,1.,-1.36999806084572));
#61129=CARTESIAN_POINT('Ctrl Pts',(3.97027773754922,1.,-1.36999806084572));
#61130=CARTESIAN_POINT('Ctrl Pts',(3.9687184694173,1.,-1.37020239094758));
#61131=CARTESIAN_POINT('Ctrl Pts',(3.96560037975788,1.,-1.37060761746027));
#61132=CARTESIAN_POINT('Ctrl Pts',(3.96092458508407,1.,-1.37120515615663));
#61133=CARTESIAN_POINT('Ctrl Pts',(3.95469287283105,1.,-1.37198126433139));
#61134=CARTESIAN_POINT('Ctrl Pts',(3.94690771786926,1.,-1.37291699203423));
#61135=CARTESIAN_POINT('Ctrl Pts',(3.93912709041791,1.,-1.37381821967499));
#61136=CARTESIAN_POINT('Ctrl Pts',(3.93135106761941,1.,-1.37468482215784));
#61137=CARTESIAN_POINT('Ctrl Pts',(3.92357976987132,1.,-1.37551664448057));
#61138=CARTESIAN_POINT('Ctrl Pts',(3.91581337461825,1.,-1.37631350505516));
#61139=CARTESIAN_POINT('Ctrl Pts',(3.90805209522729,1.,-1.3770751963376));
#61140=CARTESIAN_POINT('Ctrl Pts',(3.90029615196255,1.,-1.3778014851263));
#61141=CARTESIAN_POINT('Ctrl Pts',(3.89254574338385,1.,-1.37849211287981));
#61142=CARTESIAN_POINT('Ctrl Pts',(3.88480102249461,1.,-1.37914679719446));
#61143=CARTESIAN_POINT('Ctrl Pts',(3.87706205830865,1.,-1.37976523097187));
#61144=CARTESIAN_POINT('Ctrl Pts',(3.86932885813403,1.,-1.38034709213129));
#61145=CARTESIAN_POINT('Ctrl Pts',(3.86160143044187,1.,-1.38089205993068));
#61146=CARTESIAN_POINT('Ctrl Pts',(3.85387983979557,1.,-1.38139983115075));
#61147=CARTESIAN_POINT('Ctrl Pts',(3.84616425605705,1.,-1.38187013346089));
#61148=CARTESIAN_POINT('Ctrl Pts',(3.83845502790609,1.,-1.38230274828774));
#61149=CARTESIAN_POINT('Ctrl Pts',(3.83075266982138,1.,-1.38269750245086));
#61150=CARTESIAN_POINT('Ctrl Pts',(3.82305771743715,1.,-1.38305421262724));
#61151=CARTESIAN_POINT('Ctrl Pts',(3.81537060817765,1.,-1.38337263902766));
#61152=CARTESIAN_POINT('Ctrl Pts',(3.80769156398429,1.,-1.38365244046226));
#61153=CARTESIAN_POINT('Ctrl Pts',(3.80002044322169,1.,-1.38389311766701));
#61154=CARTESIAN_POINT('Ctrl Pts',(3.79235669640907,1.,-1.38409399694589));
#61155=CARTESIAN_POINT('Ctrl Pts',(3.78469969805134,1.,-1.38425435883773));
#61156=CARTESIAN_POINT('Ctrl Pts',(3.77704902230441,1.,-1.38437354551435));
#61157=CARTESIAN_POINT('Ctrl Pts',(3.76940473185775,1.,-1.38445107339517));
#61158=CARTESIAN_POINT('Ctrl Pts',(3.76176768271347,1.,-1.38448675253343));
#61159=CARTESIAN_POINT('Ctrl Pts',(3.75413976318727,1.,-1.38448077997155));
#61160=CARTESIAN_POINT('Ctrl Pts',(3.7465231716786,1.,-1.38443344984389));
#61161=CARTESIAN_POINT('Ctrl Pts',(3.73891976418099,1.,-1.38434489156456));
#61162=CARTESIAN_POINT('Ctrl Pts',(3.73133035859283,1.,-1.38421479111531));
#61163=CARTESIAN_POINT('Ctrl Pts',(3.72375409358805,1.,-1.3840421342895));
#61164=CARTESIAN_POINT('Ctrl Pts',(3.7161876605181,1.,-1.38382489984585));
#61165=CARTESIAN_POINT('Ctrl Pts',(3.70862680753343,1.,-1.38356065402122));
#61166=CARTESIAN_POINT('Ctrl Pts',(3.70106792167894,1.,-1.38324717612862));
#61167=CARTESIAN_POINT('Ctrl Pts',(3.69350967899523,1.,-1.38288311171649));
#61168=CARTESIAN_POINT('Ctrl Pts',(3.68595444983844,1.,-1.38246852827185));
#61169=CARTESIAN_POINT('Ctrl Pts',(3.6784103848243,1.,-1.38200574290626));
#61170=CARTESIAN_POINT('Ctrl Pts',(3.67088843112282,1.,-1.38149812653876));
#61171=CARTESIAN_POINT('Ctrl Pts',(3.66339848520874,1.,-1.38094856333558));
#61172=CARTESIAN_POINT('Ctrl Pts',(3.65594554404396,1.,-1.38035791051215));
#61173=CARTESIAN_POINT('Ctrl Pts',(3.64852652756444,1.,-1.37972372481598));
#61174=CARTESIAN_POINT('Ctrl Pts',(3.64112507791112,1.,-1.37903818567347));
#61175=CARTESIAN_POINT('Ctrl Pts',(3.63371727442448,1.,-1.37829035457325));
#61176=CARTESIAN_POINT('Ctrl Pts',(3.62628098665112,1.,-1.37746987919868));
#61177=CARTESIAN_POINT('Ctrl Pts',(3.61880481160408,1.,-1.37657053403102));
#61178=CARTESIAN_POINT('Ctrl Pts',(3.61129546591082,1.,-1.37559314436641));
#61179=CARTESIAN_POINT('Ctrl Pts',(3.60379020124038,1.,-1.37455051379642));
#61180=CARTESIAN_POINT('Ctrl Pts',(3.59634627869117,1.,-1.37346320103184));
#61181=CARTESIAN_POINT('Ctrl Pts',(3.5890185384643,1.,-1.37235053661));
#61182=CARTESIAN_POINT('Ctrl Pts',(3.58183885982745,1.,-1.37122241663073));
#61183=CARTESIAN_POINT('Ctrl Pts',(3.57479875549453,1.,-1.37007229485646));
#61184=CARTESIAN_POINT('Ctrl Pts',(3.56782080304554,1.,-1.36886584973349));
#61185=CARTESIAN_POINT('Ctrl Pts',(3.56077662028492,1.,-1.36754771771174));
#61186=CARTESIAN_POINT('Ctrl Pts',(3.55353883995793,1.,-1.36606145456711));
#61187=CARTESIAN_POINT('Ctrl Pts',(3.54602591832893,1.,-1.36436666257568));
#61188=CARTESIAN_POINT('Ctrl Pts',(3.53824396425032,1.,-1.36245507339334));
#61189=CARTESIAN_POINT('Ctrl Pts',(3.53034464961849,1.,-1.36037259643827));
#61190=CARTESIAN_POINT('Ctrl Pts',(3.52261776117121,1.,-1.35821701528975));
#61191=CARTESIAN_POINT('Ctrl Pts',(3.51542230699919,1.,-1.35611275237288));
#61192=CARTESIAN_POINT('Ctrl Pts',(3.50913227060177,1.,-1.35419113576022));
#61193=CARTESIAN_POINT('Ctrl Pts',(3.50408168106113,1.,-1.3525703284343));
#61194=CARTESIAN_POINT('Ctrl Pts',(3.5007660381658,1.,-1.35142377279535));
#61195=CARTESIAN_POINT('Ctrl Pts',(3.49920025459856,1.,-1.35080045218652));
#61196=CARTESIAN_POINT('Ctrl Pts',(3.49861894124915,1.,-1.35049736560633));
#61197=CARTESIAN_POINT('Ctrl Pts',(3.49847119623841,1.,-1.35036670893102));
#61198=CARTESIAN_POINT('Ctrl Pts',(3.49844575334386,1.,-1.35032489087269));
#61199=CARTESIAN_POINT('',(3.97027773754922,0.,-1.36999806084572));
#61200=CARTESIAN_POINT('Ctrl Pts',(3.62397690409552,-1.,-0.963997613369571));
#61201=CARTESIAN_POINT('Ctrl Pts',(3.62397690409552,1.,-0.963997613369571));
#61202=CARTESIAN_POINT('Ctrl Pts',(3.62393257642191,-1.,-0.963922720982576));
#61203=CARTESIAN_POINT('Ctrl Pts',(3.62393257642191,1.,-0.963922720982576));
#61204=CARTESIAN_POINT('Ctrl Pts',(3.62399933640277,-1.,-0.963832486396056));
#61205=CARTESIAN_POINT('Ctrl Pts',(3.62399933640277,1.,-0.963832486396056));
#61206=CARTESIAN_POINT('Ctrl Pts',(3.62456568607055,-1.,-0.963875774532103));
#61207=CARTESIAN_POINT('Ctrl Pts',(3.62456568607055,1.,-0.963875774532103));
#61208=CARTESIAN_POINT('Ctrl Pts',(3.62625391255277,-1.,-0.964291001274619));
#61209=CARTESIAN_POINT('Ctrl Pts',(3.62625391255277,1.,-0.964291001274619));
#61210=CARTESIAN_POINT('Ctrl Pts',(3.62988252139998,-1.,-0.965395153165716));
#61211=CARTESIAN_POINT('Ctrl Pts',(3.62988252139998,1.,-0.965395153165716));
#61212=CARTESIAN_POINT('Ctrl Pts',(3.6349212208096,-1.,-0.967052554540878));
#61213=CARTESIAN_POINT('Ctrl Pts',(3.6349212208096,1.,-0.967052554540878));
#61214=CARTESIAN_POINT('Ctrl Pts',(3.64113946505393,-1.,-0.969195124674829));
#61215=CARTESIAN_POINT('Ctrl Pts',(3.64113946505393,1.,-0.969195124674829));
#61216=CARTESIAN_POINT('Ctrl Pts',(3.64819756447072,-1.,-0.971722122060278));
#61217=CARTESIAN_POINT('Ctrl Pts',(3.64819756447072,1.,-0.971722122060278));
#61218=CARTESIAN_POINT('Ctrl Pts',(3.6557157673487,-1.,-0.974519971354139));
#61219=CARTESIAN_POINT('Ctrl Pts',(3.6557157673487,1.,-0.974519971354139));
#61220=CARTESIAN_POINT('Ctrl Pts',(3.66333049637403,-1.,-0.977478312751416));
#61221=CARTESIAN_POINT('Ctrl Pts',(3.66333049637403,1.,-0.977478312751416));
#61222=CARTESIAN_POINT('Ctrl Pts',(3.67074983340444,-1.,-0.980505922458495));
#61223=CARTESIAN_POINT('Ctrl Pts',(3.67074983340444,1.,-0.980505922458495));
#61224=CARTESIAN_POINT('Ctrl Pts',(3.67782408841876,-1.,-0.983550791470865));
#61225=CARTESIAN_POINT('Ctrl Pts',(3.67782408841876,1.,-0.983550791470865));
#61226=CARTESIAN_POINT('Ctrl Pts',(3.6845531792623,-1.,-0.986602639864286));
#61227=CARTESIAN_POINT('Ctrl Pts',(3.6845531792623,1.,-0.986602639864286));
#61228=CARTESIAN_POINT('Ctrl Pts',(3.69102682138955,-1.,-0.989676715398859));
#61229=CARTESIAN_POINT('Ctrl Pts',(3.69102682138955,1.,-0.989676715398859));
#61230=CARTESIAN_POINT('Ctrl Pts',(3.69738123415696,-1.,-0.992802218332104));
#61231=CARTESIAN_POINT('Ctrl Pts',(3.69738123415696,1.,-0.992802218332104));
#61232=CARTESIAN_POINT('Ctrl Pts',(3.70375282282107,-1.,-0.996009819772432));
#61233=CARTESIAN_POINT('Ctrl Pts',(3.70375282282107,1.,-0.996009819772432));
#61234=CARTESIAN_POINT('Ctrl Pts',(3.7102243971387,-1.,-0.999317260756345));
#61235=CARTESIAN_POINT('Ctrl Pts',(3.7102243971387,1.,-0.999317260756345));
#61236=CARTESIAN_POINT('Ctrl Pts',(3.71680667125047,-1.,-1.00272423396802));
#61237=CARTESIAN_POINT('Ctrl Pts',(3.71680667125047,1.,-1.00272423396802));
#61238=CARTESIAN_POINT('Ctrl Pts',(3.72346803750544,-1.,-1.00622000735696));
#61239=CARTESIAN_POINT('Ctrl Pts',(3.72346803750544,1.,-1.00622000735696));
#61240=CARTESIAN_POINT('Ctrl Pts',(3.73015276704407,-1.,-1.00978798539491));
#61241=CARTESIAN_POINT('Ctrl Pts',(3.73015276704407,1.,-1.00978798539491));
#61242=CARTESIAN_POINT('Ctrl Pts',(3.73680245055747,-1.,-1.01341114319906));
#61243=CARTESIAN_POINT('Ctrl Pts',(3.73680245055747,1.,-1.01341114319906));
#61244=CARTESIAN_POINT('Ctrl Pts',(3.74337942504993,-1.,-1.01707794311088));
#61245=CARTESIAN_POINT('Ctrl Pts',(3.74337942504993,1.,-1.01707794311088));
#61246=CARTESIAN_POINT('Ctrl Pts',(3.74987777155873,-1.,-1.02078510487439));
#61247=CARTESIAN_POINT('Ctrl Pts',(3.74987777155873,1.,-1.02078510487439));
#61248=CARTESIAN_POINT('Ctrl Pts',(3.75631037456224,-1.,-1.02453429444668));
#61249=CARTESIAN_POINT('Ctrl Pts',(3.75631037456224,1.,-1.02453429444668));
#61250=CARTESIAN_POINT('Ctrl Pts',(3.76270122291245,-1.,-1.02833014458184));
#61251=CARTESIAN_POINT('Ctrl Pts',(3.76270122291245,1.,-1.02833014458184));
#61252=CARTESIAN_POINT('Ctrl Pts',(3.76907609832516,-1.,-1.03217786604919));
#61253=CARTESIAN_POINT('Ctrl Pts',(3.76907609832516,1.,-1.03217786604919));
#61254=CARTESIAN_POINT('Ctrl Pts',(3.77545283140427,-1.,-1.03608074678008));
#61255=CARTESIAN_POINT('Ctrl Pts',(3.77545283140427,1.,-1.03608074678008));
#61256=CARTESIAN_POINT('Ctrl Pts',(3.7818353500817,-1.,-1.04003862055798));
#61257=CARTESIAN_POINT('Ctrl Pts',(3.7818353500817,1.,-1.04003862055798));
#61258=CARTESIAN_POINT('Ctrl Pts',(3.78821910787179,-1.,-1.04404924374422));
#61259=CARTESIAN_POINT('Ctrl Pts',(3.78821910787179,1.,-1.04404924374422));
#61260=CARTESIAN_POINT('Ctrl Pts',(3.79459440308786,-1.,-1.04810913267639));
#61261=CARTESIAN_POINT('Ctrl Pts',(3.79459440308786,1.,-1.04810913267639));
#61262=CARTESIAN_POINT('Ctrl Pts',(3.80095039790681,-1.,-1.05221457990016));
#61263=CARTESIAN_POINT('Ctrl Pts',(3.80095039790681,1.,-1.05221457990016));
#61264=CARTESIAN_POINT('Ctrl Pts',(3.80727913637791,-1.,-1.05636266918644));
#61265=CARTESIAN_POINT('Ctrl Pts',(3.80727913637791,1.,-1.05636266918644));
#61266=CARTESIAN_POINT('Ctrl Pts',(3.8135786611749,-1.,-1.06055206187299));
#61267=CARTESIAN_POINT('Ctrl Pts',(3.8135786611749,1.,-1.06055206187299));
#61268=CARTESIAN_POINT('Ctrl Pts',(3.81985083953012,-1.,-1.0647824403893));
#61269=CARTESIAN_POINT('Ctrl Pts',(3.81985083953012,1.,-1.0647824403893));
#61270=CARTESIAN_POINT('Ctrl Pts',(3.82609989967276,-1.,-1.06905413180359));
#61271=CARTESIAN_POINT('Ctrl Pts',(3.82609989967276,1.,-1.06905413180359));
#61272=CARTESIAN_POINT('Ctrl Pts',(3.83233071195144,-1.,-1.07336766633459));
#61273=CARTESIAN_POINT('Ctrl Pts',(3.83233071195144,1.,-1.07336766633459));
#61274=CARTESIAN_POINT('Ctrl Pts',(3.83854714117491,-1.,-1.07772335353858));
#61275=CARTESIAN_POINT('Ctrl Pts',(3.83854714117491,1.,-1.07772335353858));
#61276=CARTESIAN_POINT('Ctrl Pts',(3.8447504803063,-1.,-1.08212087917991));
#61277=CARTESIAN_POINT('Ctrl Pts',(3.8447504803063,1.,-1.08212087917991));
#61278=CARTESIAN_POINT('Ctrl Pts',(3.85094025222713,-1.,-1.08655950846384));
#61279=CARTESIAN_POINT('Ctrl Pts',(3.85094025222713,1.,-1.08655950846384));
#61280=CARTESIAN_POINT('Ctrl Pts',(3.85711487933931,-1.,-1.09103825516294));
#61281=CARTESIAN_POINT('Ctrl Pts',(3.85711487933931,1.,-1.09103825516294));
#61282=CARTESIAN_POINT('Ctrl Pts',(3.86327241021247,-1.,-1.09555606505013));
#61283=CARTESIAN_POINT('Ctrl Pts',(3.86327241021247,1.,-1.09555606505013));
#61284=CARTESIAN_POINT('Ctrl Pts',(3.86941120134849,-1.,-1.10011198761195));
#61285=CARTESIAN_POINT('Ctrl Pts',(3.86941120134849,1.,-1.10011198761195));
#61286=CARTESIAN_POINT('Ctrl Pts',(3.87553067187514,-1.,-1.10470536603287));
#61287=CARTESIAN_POINT('Ctrl Pts',(3.87553067187514,1.,-1.10470536603287));
#61288=CARTESIAN_POINT('Ctrl Pts',(3.88163105531724,-1.,-1.10933577224008));
#61289=CARTESIAN_POINT('Ctrl Pts',(3.88163105531724,1.,-1.10933577224008));
#61290=CARTESIAN_POINT('Ctrl Pts',(3.88771308285171,-1.,-1.11400292434429));
#61291=CARTESIAN_POINT('Ctrl Pts',(3.88771308285171,1.,-1.11400292434429));
#61292=CARTESIAN_POINT('Ctrl Pts',(3.89377768340344,-1.,-1.11870660794603));
#61293=CARTESIAN_POINT('Ctrl Pts',(3.89377768340344,1.,-1.11870660794603));
#61294=CARTESIAN_POINT('Ctrl Pts',(3.89982569750025,-1.,-1.12344660099043));
#61295=CARTESIAN_POINT('Ctrl Pts',(3.89982569750025,1.,-1.12344660099043));
#61296=CARTESIAN_POINT('Ctrl Pts',(3.90585753318737,-1.,-1.12822258281553));
#61297=CARTESIAN_POINT('Ctrl Pts',(3.90585753318737,1.,-1.12822258281553));
#61298=CARTESIAN_POINT('Ctrl Pts',(3.91187321145649,-1.,-1.13303414693896));
#61299=CARTESIAN_POINT('Ctrl Pts',(3.91187321145649,1.,-1.13303414693896));
#61300=CARTESIAN_POINT('Ctrl Pts',(3.91787251936827,-1.,-1.13788084225554));
#61301=CARTESIAN_POINT('Ctrl Pts',(3.91787251936827,1.,-1.13788084225554));
#61302=CARTESIAN_POINT('Ctrl Pts',(3.92385513133997,-1.,-1.14276220561593));
#61303=CARTESIAN_POINT('Ctrl Pts',(3.92385513133997,1.,-1.14276220561593));
#61304=CARTESIAN_POINT('Ctrl Pts',(3.92982073294257,-1.,-1.14767779451124));
#61305=CARTESIAN_POINT('Ctrl Pts',(3.92982073294257,1.,-1.14767779451124));
#61306=CARTESIAN_POINT('Ctrl Pts',(3.9357691705628,-1.,-1.1526272271632));
#61307=CARTESIAN_POINT('Ctrl Pts',(3.9357691705628,1.,-1.1526272271632));
#61308=CARTESIAN_POINT('Ctrl Pts',(3.94170046685203,-1.,-1.15761018340956));
#61309=CARTESIAN_POINT('Ctrl Pts',(3.94170046685203,1.,-1.15761018340956));
#61310=CARTESIAN_POINT('Ctrl Pts',(3.94761474780583,-1.,-1.16262637999157));
#61311=CARTESIAN_POINT('Ctrl Pts',(3.94761474780583,1.,-1.16262637999157));
#61312=CARTESIAN_POINT('Ctrl Pts',(3.95351219509876,-1.,-1.16767555244438));
#61313=CARTESIAN_POINT('Ctrl Pts',(3.95351219509876,1.,-1.16767555244438));
#61314=CARTESIAN_POINT('Ctrl Pts',(3.95939299213276,-1.,-1.17275743590361));
#61315=CARTESIAN_POINT('Ctrl Pts',(3.95939299213276,1.,-1.17275743590361));
#61316=CARTESIAN_POINT('Ctrl Pts',(3.96525726358159,-1.,-1.17787174135592));
#61317=CARTESIAN_POINT('Ctrl Pts',(3.96525726358159,1.,-1.17787174135592));
#61318=CARTESIAN_POINT('Ctrl Pts',(3.97110505165415,-1.,-1.18301815039831));
#61319=CARTESIAN_POINT('Ctrl Pts',(3.97110505165415,1.,-1.18301815039831));
#61320=CARTESIAN_POINT('Ctrl Pts',(3.97693634767754,-1.,-1.18819633715539));
#61321=CARTESIAN_POINT('Ctrl Pts',(3.97693634767754,1.,-1.18819633715539));
#61322=CARTESIAN_POINT('Ctrl Pts',(3.98275111052561,-1.,-1.19340598349475));
#61323=CARTESIAN_POINT('Ctrl Pts',(3.98275111052561,1.,-1.19340598349475));
#61324=CARTESIAN_POINT('Ctrl Pts',(3.98854928957189,-1.,-1.19864679609566));
#61325=CARTESIAN_POINT('Ctrl Pts',(3.98854928957189,1.,-1.19864679609566));
#61326=CARTESIAN_POINT('Ctrl Pts',(3.99433084799666,-1.,-1.20391852375139));
#61327=CARTESIAN_POINT('Ctrl Pts',(3.99433084799666,1.,-1.20391852375139));
#61328=CARTESIAN_POINT('Ctrl Pts',(4.00009577950721,-1.,-1.20922097029551));
#61329=CARTESIAN_POINT('Ctrl Pts',(4.00009577950721,1.,-1.20922097029551));
#61330=CARTESIAN_POINT('Ctrl Pts',(4.00584409522722,-1.,-1.21455398918133));
#61331=CARTESIAN_POINT('Ctrl Pts',(4.00584409522722,1.,-1.21455398918133));
#61332=CARTESIAN_POINT('Ctrl Pts',(4.01042947140789,-1.,-1.21884478244403));
#61333=CARTESIAN_POINT('Ctrl Pts',(4.01042947140789,1.,-1.21884478244403));
#61334=CARTESIAN_POINT('Ctrl Pts',(4.01386104433519,-1.,-1.22207656455845));
#61335=CARTESIAN_POINT('Ctrl Pts',(4.01386104433519,1.,-1.22207656455845));
#61336=CARTESIAN_POINT('Ctrl Pts',(4.01614544569895,-1.,-1.22423716681317));
#61337=CARTESIAN_POINT('Ctrl Pts',(4.01614544569895,1.,-1.22423716681317));
#61338=CARTESIAN_POINT('Ctrl Pts',(4.01728681790024,-1.,-1.22531898815164));
#61339=CARTESIAN_POINT('Ctrl Pts',(4.01728681790024,1.,-1.22531898815164));
#61340=CARTESIAN_POINT('',(3.62400312501199,1.,-0.963899035118984));
#61341=CARTESIAN_POINT('Ctrl Pts',(3.62400312501199,-1.,-0.963899035118986));
#61342=CARTESIAN_POINT('Ctrl Pts',(3.62400312501199,-0.666666666666667,
-0.963899035118986));
#61343=CARTESIAN_POINT('Ctrl Pts',(3.62400312501199,-0.333333333333333,
-0.963899035118986));
#61344=CARTESIAN_POINT('Ctrl Pts',(3.62400312501199,0.333333333333333,-0.963899035118986));
#61345=CARTESIAN_POINT('Ctrl Pts',(3.62400312501199,0.666666666666667,-0.963899035118986));
#61346=CARTESIAN_POINT('Ctrl Pts',(3.62400312501199,1.,-0.963899035118986));
#61347=CARTESIAN_POINT('',(4.01728681790024,1.,-1.22531898815164));
#61348=CARTESIAN_POINT('',(4.01728681790024,0.,-1.22531898815164));
#61349=CARTESIAN_POINT('Ctrl Pts',(3.62400312501199,1.,-0.963899035118985));
#61350=CARTESIAN_POINT('Ctrl Pts',(3.62404828878374,1.,-0.963880158556713));
#61351=CARTESIAN_POINT('Ctrl Pts',(3.62424461507455,1.,-0.963861297423579));
#61352=CARTESIAN_POINT('Ctrl Pts',(3.62489305727516,1.,-0.96395778264259));
#61353=CARTESIAN_POINT('Ctrl Pts',(3.62652618145252,1.,-0.964373850166082));
#61354=CARTESIAN_POINT('Ctrl Pts',(3.62988252139998,1.,-0.965395153165716));
#61355=CARTESIAN_POINT('Ctrl Pts',(3.6349212208096,1.,-0.967052554540878));
#61356=CARTESIAN_POINT('Ctrl Pts',(3.64113946505393,1.,-0.969195124674829));
#61357=CARTESIAN_POINT('Ctrl Pts',(3.64819756447072,1.,-0.971722122060278));
#61358=CARTESIAN_POINT('Ctrl Pts',(3.6557157673487,1.,-0.974519971354139));
#61359=CARTESIAN_POINT('Ctrl Pts',(3.66333049637403,1.,-0.977478312751416));
#61360=CARTESIAN_POINT('Ctrl Pts',(3.67074983340444,1.,-0.980505922458495));
#61361=CARTESIAN_POINT('Ctrl Pts',(3.67782408841876,1.,-0.983550791470865));
#61362=CARTESIAN_POINT('Ctrl Pts',(3.6845531792623,1.,-0.986602639864286));
#61363=CARTESIAN_POINT('Ctrl Pts',(3.69102682138955,1.,-0.989676715398859));
#61364=CARTESIAN_POINT('Ctrl Pts',(3.69738123415696,1.,-0.992802218332104));
#61365=CARTESIAN_POINT('Ctrl Pts',(3.70375282282107,1.,-0.996009819772432));
#61366=CARTESIAN_POINT('Ctrl Pts',(3.7102243971387,1.,-0.999317260756345));
#61367=CARTESIAN_POINT('Ctrl Pts',(3.71680667125047,1.,-1.00272423396802));
#61368=CARTESIAN_POINT('Ctrl Pts',(3.72346803750544,1.,-1.00622000735696));
#61369=CARTESIAN_POINT('Ctrl Pts',(3.73015276704407,1.,-1.00978798539491));
#61370=CARTESIAN_POINT('Ctrl Pts',(3.73680245055747,1.,-1.01341114319906));
#61371=CARTESIAN_POINT('Ctrl Pts',(3.74337942504993,1.,-1.01707794311088));
#61372=CARTESIAN_POINT('Ctrl Pts',(3.74987777155873,1.,-1.02078510487439));
#61373=CARTESIAN_POINT('Ctrl Pts',(3.75631037456224,1.,-1.02453429444668));
#61374=CARTESIAN_POINT('Ctrl Pts',(3.76270122291245,1.,-1.02833014458184));
#61375=CARTESIAN_POINT('Ctrl Pts',(3.76907609832516,1.,-1.03217786604919));
#61376=CARTESIAN_POINT('Ctrl Pts',(3.77545283140427,1.,-1.03608074678008));
#61377=CARTESIAN_POINT('Ctrl Pts',(3.7818353500817,1.,-1.04003862055798));
#61378=CARTESIAN_POINT('Ctrl Pts',(3.78821910787179,1.,-1.04404924374422));
#61379=CARTESIAN_POINT('Ctrl Pts',(3.79459440308786,1.,-1.04810913267639));
#61380=CARTESIAN_POINT('Ctrl Pts',(3.80095039790681,1.,-1.05221457990016));
#61381=CARTESIAN_POINT('Ctrl Pts',(3.80727913637791,1.,-1.05636266918644));
#61382=CARTESIAN_POINT('Ctrl Pts',(3.8135786611749,1.,-1.06055206187299));
#61383=CARTESIAN_POINT('Ctrl Pts',(3.81985083953012,1.,-1.0647824403893));
#61384=CARTESIAN_POINT('Ctrl Pts',(3.82609989967276,1.,-1.06905413180359));
#61385=CARTESIAN_POINT('Ctrl Pts',(3.83233071195144,1.,-1.07336766633459));
#61386=CARTESIAN_POINT('Ctrl Pts',(3.83854714117491,1.,-1.07772335353858));
#61387=CARTESIAN_POINT('Ctrl Pts',(3.8447504803063,1.,-1.08212087917991));
#61388=CARTESIAN_POINT('Ctrl Pts',(3.85094025222713,1.,-1.08655950846384));
#61389=CARTESIAN_POINT('Ctrl Pts',(3.85711487933931,1.,-1.09103825516294));
#61390=CARTESIAN_POINT('Ctrl Pts',(3.86327241021247,1.,-1.09555606505013));
#61391=CARTESIAN_POINT('Ctrl Pts',(3.86941120134849,1.,-1.10011198761195));
#61392=CARTESIAN_POINT('Ctrl Pts',(3.87553067187514,1.,-1.10470536603287));
#61393=CARTESIAN_POINT('Ctrl Pts',(3.88163105531724,1.,-1.10933577224008));
#61394=CARTESIAN_POINT('Ctrl Pts',(3.88771308285171,1.,-1.11400292434429));
#61395=CARTESIAN_POINT('Ctrl Pts',(3.89377768340344,1.,-1.11870660794603));
#61396=CARTESIAN_POINT('Ctrl Pts',(3.89982569750025,1.,-1.12344660099043));
#61397=CARTESIAN_POINT('Ctrl Pts',(3.90585753318737,1.,-1.12822258281553));
#61398=CARTESIAN_POINT('Ctrl Pts',(3.91187321145649,1.,-1.13303414693896));
#61399=CARTESIAN_POINT('Ctrl Pts',(3.91787251936827,1.,-1.13788084225554));
#61400=CARTESIAN_POINT('Ctrl Pts',(3.92385513133997,1.,-1.14276220561593));
#61401=CARTESIAN_POINT('Ctrl Pts',(3.92982073294257,1.,-1.14767779451124));
#61402=CARTESIAN_POINT('Ctrl Pts',(3.9357691705628,1.,-1.1526272271632));
#61403=CARTESIAN_POINT('Ctrl Pts',(3.94170046685203,1.,-1.15761018340956));
#61404=CARTESIAN_POINT('Ctrl Pts',(3.94761474780583,1.,-1.16262637999157));
#61405=CARTESIAN_POINT('Ctrl Pts',(3.95351219509876,1.,-1.16767555244438));
#61406=CARTESIAN_POINT('Ctrl Pts',(3.95939299213276,1.,-1.17275743590361));
#61407=CARTESIAN_POINT('Ctrl Pts',(3.96525726358159,1.,-1.17787174135592));
#61408=CARTESIAN_POINT('Ctrl Pts',(3.97110505165415,1.,-1.18301815039831));
#61409=CARTESIAN_POINT('Ctrl Pts',(3.97693634767754,1.,-1.18819633715539));
#61410=CARTESIAN_POINT('Ctrl Pts',(3.98275111052561,1.,-1.19340598349475));
#61411=CARTESIAN_POINT('Ctrl Pts',(3.98854928957189,1.,-1.19864679609566));
#61412=CARTESIAN_POINT('Ctrl Pts',(3.99433084799666,1.,-1.20391852375139));
#61413=CARTESIAN_POINT('Ctrl Pts',(4.00009577950721,1.,-1.20922097029551));
#61414=CARTESIAN_POINT('Ctrl Pts',(4.00584409522722,1.,-1.21455398918133));
#61415=CARTESIAN_POINT('Ctrl Pts',(4.01042947140789,1.,-1.21884478244403));
#61416=CARTESIAN_POINT('Ctrl Pts',(4.01386104433519,1.,-1.22207656455845));
#61417=CARTESIAN_POINT('Ctrl Pts',(4.01614544569895,1.,-1.22423716681317));
#61418=CARTESIAN_POINT('Ctrl Pts',(4.01728681790024,1.,-1.22531898815164));
#61419=CARTESIAN_POINT('Origin',(4.01728681790024,0.,-1.22531898815164));
#61420=CARTESIAN_POINT('',(3.97027773754922,1.,-1.36999806084572));
#61421=CARTESIAN_POINT('Origin',(0.,0.,0.));
#61422=CARTESIAN_POINT('',(3.66661143271648,1.,-0.786422660833743));
#61423=CARTESIAN_POINT('Origin',(0.,1.,0.));
#61424=CARTESIAN_POINT('Ctrl Pts',(3.66661143271648,1.,-0.786422660833743));
#61425=CARTESIAN_POINT('Ctrl Pts',(3.66661143271648,0.666666666666667,-0.786422660833743));
#61426=CARTESIAN_POINT('Ctrl Pts',(3.66661143271648,0.333333333333333,-0.786422660833743));
#61427=CARTESIAN_POINT('Ctrl Pts',(3.66661143271648,-0.333333333333333,
-0.786422660833743));
#61428=CARTESIAN_POINT('Ctrl Pts',(3.66661143271648,-0.666666666666667,
-0.786422660833742));
#61429=CARTESIAN_POINT('Ctrl Pts',(3.66661143271648,-1.,-0.786422660833742));
#61430=CARTESIAN_POINT('Ctrl Pts',(4.13571194405636,-1.,-0.73204283740062));
#61431=CARTESIAN_POINT('Ctrl Pts',(4.13571194405636,1.,-0.73204283740062));
#61432=CARTESIAN_POINT('Ctrl Pts',(4.13420383737278,-1.,-0.732488575135926));
#61433=CARTESIAN_POINT('Ctrl Pts',(4.13420383737278,1.,-0.732488575135926));
#61434=CARTESIAN_POINT('Ctrl Pts',(4.13118752796397,-1.,-0.733376589325634));
#61435=CARTESIAN_POINT('Ctrl Pts',(4.13118752796397,1.,-0.733376589325634));
#61436=CARTESIAN_POINT('Ctrl Pts',(4.12666277572794,-1.,-0.734698226767513));
#61437=CARTESIAN_POINT('Ctrl Pts',(4.12666277572794,1.,-0.734698226767513));
#61438=CARTESIAN_POINT('Ctrl Pts',(4.12062919626082,-1.,-0.736439634335347));
#61439=CARTESIAN_POINT('Ctrl Pts',(4.12062919626082,1.,-0.736439634335347));
#61440=CARTESIAN_POINT('Ctrl Pts',(4.11308626953795,-1.,-0.738581708229119));
#61441=CARTESIAN_POINT('Ctrl Pts',(4.11308626953795,1.,-0.738581708229119));
#61442=CARTESIAN_POINT('Ctrl Pts',(4.1055424175856,-1.,-0.740688998555152));
#61443=CARTESIAN_POINT('Ctrl Pts',(4.1055424175856,1.,-0.740688998555152));
#61444=CARTESIAN_POINT('Ctrl Pts',(4.09799769702712,-1.,-0.742761369690018));
#61445=CARTESIAN_POINT('Ctrl Pts',(4.09799769702712,1.,-0.742761369690018));
#61446=CARTESIAN_POINT('Ctrl Pts',(4.09045220253011,-1.,-0.744798649705514));
#61447=CARTESIAN_POINT('Ctrl Pts',(4.09045220253011,1.,-0.744798649705514));
#61448=CARTESIAN_POINT('Ctrl Pts',(4.08290608094789,-1.,-0.746800631490822));
#61449=CARTESIAN_POINT('Ctrl Pts',(4.08290608094789,1.,-0.746800631490822));
#61450=CARTESIAN_POINT('Ctrl Pts',(4.07535951055363,-1.,-0.748767076679177));
#61451=CARTESIAN_POINT('Ctrl Pts',(4.07535951055363,1.,-0.748767076679177));
#61452=CARTESIAN_POINT('Ctrl Pts',(4.06781267241886,-1.,-0.750697720483176));
#61453=CARTESIAN_POINT('Ctrl Pts',(4.06781267241886,1.,-0.750697720483176));
#61454=CARTESIAN_POINT('Ctrl Pts',(4.06026572221399,-1.,-0.752592276482869));
#61455=CARTESIAN_POINT('Ctrl Pts',(4.06026572221399,1.,-0.752592276482869));
#61456=CARTESIAN_POINT('Ctrl Pts',(4.05271876688106,-1.,-0.754450441816412));
#61457=CARTESIAN_POINT('Ctrl Pts',(4.05271876688106,1.,-0.754450441816412));
#61458=CARTESIAN_POINT('Ctrl Pts',(4.04517182654344,-1.,-0.756271902370187));
#61459=CARTESIAN_POINT('Ctrl Pts',(4.04517182654344,1.,-0.756271902370187));
#61460=CARTESIAN_POINT('Ctrl Pts',(4.03762485803468,-1.,-0.758056338885554));
#61461=CARTESIAN_POINT('Ctrl Pts',(4.03762485803468,1.,-0.758056338885554));
#61462=CARTESIAN_POINT('Ctrl Pts',(4.0300778195465,-1.,-0.759803433244166));
#61463=CARTESIAN_POINT('Ctrl Pts',(4.0300778195465,1.,-0.759803433244166));
#61464=CARTESIAN_POINT('Ctrl Pts',(4.02253072741347,-1.,-0.761512875859942));
#61465=CARTESIAN_POINT('Ctrl Pts',(4.02253072741347,1.,-0.761512875859942));
#61466=CARTESIAN_POINT('Ctrl Pts',(4.01498370680434,-1.,-0.763184371182827));
#61467=CARTESIAN_POINT('Ctrl Pts',(4.01498370680434,1.,-0.763184371182827));
#61468=CARTESIAN_POINT('Ctrl Pts',(4.00743706791366,-1.,-0.764817648784947));
#61469=CARTESIAN_POINT('Ctrl Pts',(4.00743706791366,1.,-0.764817648784947));
#61470=CARTESIAN_POINT('Ctrl Pts',(3.99989129179464,-1.,-0.766412457135786));
#61471=CARTESIAN_POINT('Ctrl Pts',(3.99989129179464,1.,-0.766412457135786));
#61472=CARTESIAN_POINT('Ctrl Pts',(3.99234687880892,-1.,-0.767968531377708));
#61473=CARTESIAN_POINT('Ctrl Pts',(3.99234687880892,1.,-0.767968531377708));
#61474=CARTESIAN_POINT('Ctrl Pts',(3.98480422348403,-1.,-0.76948556624546));
#61475=CARTESIAN_POINT('Ctrl Pts',(3.98480422348403,1.,-0.76948556624546));
#61476=CARTESIAN_POINT('Ctrl Pts',(3.97726349165507,-1.,-0.770963190030504));
#61477=CARTESIAN_POINT('Ctrl Pts',(3.97726349165507,1.,-0.770963190030504));
#61478=CARTESIAN_POINT('Ctrl Pts',(3.96972446532832,-1.,-0.772400931772239));
#61479=CARTESIAN_POINT('Ctrl Pts',(3.96972446532832,1.,-0.772400931772239));
#61480=CARTESIAN_POINT('Ctrl Pts',(3.96218649639876,-1.,-0.773798212026683));
#61481=CARTESIAN_POINT('Ctrl Pts',(3.96218649639876,1.,-0.773798212026683));
#61482=CARTESIAN_POINT('Ctrl Pts',(3.95464885452364,-1.,-0.775154418039442));
#61483=CARTESIAN_POINT('Ctrl Pts',(3.95464885452364,1.,-0.775154418039442));
#61484=CARTESIAN_POINT('Ctrl Pts',(3.94711101619471,-1.,-0.77646896669796));
#61485=CARTESIAN_POINT('Ctrl Pts',(3.94711101619471,1.,-0.77646896669796));
#61486=CARTESIAN_POINT('Ctrl Pts',(3.93957296768098,-1.,-0.77774137056855));
#61487=CARTESIAN_POINT('Ctrl Pts',(3.93957296768098,1.,-0.77774137056855));
#61488=CARTESIAN_POINT('Ctrl Pts',(3.93203552473153,-1.,-0.778971308134786));
#61489=CARTESIAN_POINT('Ctrl Pts',(3.93203552473153,1.,-0.778971308134786));
#61490=CARTESIAN_POINT('Ctrl Pts',(3.92450058323799,-1.,-0.780158678615507));
#61491=CARTESIAN_POINT('Ctrl Pts',(3.92450058323799,1.,-0.780158678615507));
#61492=CARTESIAN_POINT('Ctrl Pts',(3.9169703605466,-1.,-0.781303428618344));
#61493=CARTESIAN_POINT('Ctrl Pts',(3.9169703605466,1.,-0.781303428618344));
#61494=CARTESIAN_POINT('Ctrl Pts',(3.90944671004536,-1.,-0.782405395622759));
#61495=CARTESIAN_POINT('Ctrl Pts',(3.90944671004536,1.,-0.782405395622759));
#61496=CARTESIAN_POINT('Ctrl Pts',(3.90193039043971,-1.,-0.783464141529083));
#61497=CARTESIAN_POINT('Ctrl Pts',(3.90193039043971,1.,-0.783464141529083));
#61498=CARTESIAN_POINT('Ctrl Pts',(3.89442039235105,-1.,-0.784478799358336));
#61499=CARTESIAN_POINT('Ctrl Pts',(3.89442039235105,1.,-0.784478799358336));
#61500=CARTESIAN_POINT('Ctrl Pts',(3.88691313167399,-1.,-0.785447890340723));
#61501=CARTESIAN_POINT('Ctrl Pts',(3.88691313167399,1.,-0.785447890340723));
#61502=CARTESIAN_POINT('Ctrl Pts',(3.87940402818186,-1.,-0.786369675812592));
#61503=CARTESIAN_POINT('Ctrl Pts',(3.87940402818186,1.,-0.786369675812592));
#61504=CARTESIAN_POINT('Ctrl Pts',(3.87188916600905,-1.,-0.787242527617981));
#61505=CARTESIAN_POINT('Ctrl Pts',(3.87188916600905,1.,-0.787242527617981));
#61506=CARTESIAN_POINT('Ctrl Pts',(3.86436702561342,-1.,-0.788065315093771));
#61507=CARTESIAN_POINT('Ctrl Pts',(3.86436702561342,1.,-0.788065315093771));
#61508=CARTESIAN_POINT('Ctrl Pts',(3.85683995872536,-1.,-0.788837734090688));
#61509=CARTESIAN_POINT('Ctrl Pts',(3.85683995872536,1.,-0.788837734090688));
#61510=CARTESIAN_POINT('Ctrl Pts',(3.8493163780891,-1.,-0.789560798155619));
#61511=CARTESIAN_POINT('Ctrl Pts',(3.8493163780891,1.,-0.789560798155619));
#61512=CARTESIAN_POINT('Ctrl Pts',(3.84180762342476,-1.,-0.790236124191289));
#61513=CARTESIAN_POINT('Ctrl Pts',(3.84180762342476,1.,-0.790236124191289));
#61514=CARTESIAN_POINT('Ctrl Pts',(3.83432392054804,-1.,-0.79086501270534));
#61515=CARTESIAN_POINT('Ctrl Pts',(3.83432392054804,1.,-0.79086501270534));
#61516=CARTESIAN_POINT('Ctrl Pts',(3.82687033899799,-1.,-0.791447528662381));
#61517=CARTESIAN_POINT('Ctrl Pts',(3.82687033899799,1.,-0.791447528662381));
#61518=CARTESIAN_POINT('Ctrl Pts',(3.81944345442237,-1.,-0.791981740718607));
#61519=CARTESIAN_POINT('Ctrl Pts',(3.81944345442237,1.,-0.791981740718607));
#61520=CARTESIAN_POINT('Ctrl Pts',(3.81202588694726,-1.,-0.792462483517568));
#61521=CARTESIAN_POINT('Ctrl Pts',(3.81202588694726,1.,-0.792462483517568));
#61522=CARTESIAN_POINT('Ctrl Pts',(3.80459229925598,-1.,-0.792882695234693));
#61523=CARTESIAN_POINT('Ctrl Pts',(3.80459229925598,1.,-0.792882695234693));
#61524=CARTESIAN_POINT('Ctrl Pts',(3.79711921389862,-1.,-0.793235612973201));
#61525=CARTESIAN_POINT('Ctrl Pts',(3.79711921389862,1.,-0.793235612973201));
#61526=CARTESIAN_POINT('Ctrl Pts',(3.78959439439222,-1.,-0.793516871680966));
#61527=CARTESIAN_POINT('Ctrl Pts',(3.78959439439222,1.,-0.793516871680966));
#61528=CARTESIAN_POINT('Ctrl Pts',(3.78202460377617,-1.,-0.79372623578134));
#61529=CARTESIAN_POINT('Ctrl Pts',(3.78202460377617,1.,-0.79372623578134));
#61530=CARTESIAN_POINT('Ctrl Pts',(3.77444863801264,-1.,-0.793870523787515));
#61531=CARTESIAN_POINT('Ctrl Pts',(3.77444863801264,1.,-0.793870523787515));
#61532=CARTESIAN_POINT('Ctrl Pts',(3.76692626931184,-1.,-0.793961083689141));
#61533=CARTESIAN_POINT('Ctrl Pts',(3.76692626931184,1.,-0.793961083689141));
#61534=CARTESIAN_POINT('Ctrl Pts',(3.75951468666325,-1.,-0.794008429135047));
#61535=CARTESIAN_POINT('Ctrl Pts',(3.75951468666325,1.,-0.794008429135047));
#61536=CARTESIAN_POINT('Ctrl Pts',(3.75224692493895,-1.,-0.794017347371441));
#61537=CARTESIAN_POINT('Ctrl Pts',(3.75224692493895,1.,-0.794017347371441));
#61538=CARTESIAN_POINT('Ctrl Pts',(3.74511357728827,-1.,-0.79398270045988));
#61539=CARTESIAN_POINT('Ctrl Pts',(3.74511357728827,1.,-0.79398270045988));
#61540=CARTESIAN_POINT('Ctrl Pts',(3.73803280541576,-1.,-0.793882700936791));
#61541=CARTESIAN_POINT('Ctrl Pts',(3.73803280541576,1.,-0.793882700936791));
#61542=CARTESIAN_POINT('Ctrl Pts',(3.7308691469564,-1.,-0.793682750269348));
#61543=CARTESIAN_POINT('Ctrl Pts',(3.7308691469564,1.,-0.793682750269348));
#61544=CARTESIAN_POINT('Ctrl Pts',(3.7234879729357,-1.,-0.793347023783871));
#61545=CARTESIAN_POINT('Ctrl Pts',(3.7234879729357,1.,-0.793347023783871));
#61546=CARTESIAN_POINT('Ctrl Pts',(3.7158024239604,-1.,-0.792848377370116));
#61547=CARTESIAN_POINT('Ctrl Pts',(3.7158024239604,1.,-0.792848377370116));
#61548=CARTESIAN_POINT('Ctrl Pts',(3.70781724021879,-1.,-0.792177688845968));
#61549=CARTESIAN_POINT('Ctrl Pts',(3.70781724021879,1.,-0.792177688845968));
#61550=CARTESIAN_POINT('Ctrl Pts',(3.69968940808982,-1.,-0.791356575696509));
#61551=CARTESIAN_POINT('Ctrl Pts',(3.69968940808982,1.,-0.791356575696509));
#61552=CARTESIAN_POINT('Ctrl Pts',(3.69172044327754,-1.,-0.79043628498958));
#61553=CARTESIAN_POINT('Ctrl Pts',(3.69172044327754,1.,-0.79043628498958));
#61554=CARTESIAN_POINT('Ctrl Pts',(3.68428439784285,-1.,-0.789483546065159));
#61555=CARTESIAN_POINT('Ctrl Pts',(3.68428439784285,1.,-0.789483546065159));
#61556=CARTESIAN_POINT('Ctrl Pts',(3.67777119516438,-1.,-0.788569566220663));
#61557=CARTESIAN_POINT('Ctrl Pts',(3.67777119516438,1.,-0.788569566220663));
#61558=CARTESIAN_POINT('Ctrl Pts',(3.672529236635,-1.,-0.787758799995427));
#61559=CARTESIAN_POINT('Ctrl Pts',(3.672529236635,1.,-0.787758799995427));
#61560=CARTESIAN_POINT('Ctrl Pts',(3.66879484800625,-1.,-0.787095252589508));
#61561=CARTESIAN_POINT('Ctrl Pts',(3.66879484800625,1.,-0.787095252589508));
#61562=CARTESIAN_POINT('Ctrl Pts',(3.66710211819938,-1.,-0.786698783541658));
#61563=CARTESIAN_POINT('Ctrl Pts',(3.66710211819938,1.,-0.786698783541658));
#61564=CARTESIAN_POINT('Ctrl Pts',(3.66657784454965,-1.,-0.786480236184947));
#61565=CARTESIAN_POINT('Ctrl Pts',(3.66657784454965,1.,-0.786480236184947));
#61566=CARTESIAN_POINT('Ctrl Pts',(3.66655932661846,-1.,-0.78636952818304));
#61567=CARTESIAN_POINT('Ctrl Pts',(3.66655932661846,1.,-0.78636952818304));
#61568=CARTESIAN_POINT('Ctrl Pts',(3.66663282329846,-1.,-0.786322922920599));
#61569=CARTESIAN_POINT('Ctrl Pts',(3.66663282329846,1.,-0.786322922920599));
#61570=CARTESIAN_POINT('',(4.13571194405636,1.,-0.73204283740062));
#61571=CARTESIAN_POINT('Ctrl Pts',(4.13571194405636,1.,-0.73204283740062));
#61572=CARTESIAN_POINT('Ctrl Pts',(4.13420383737278,1.,-0.732488575135926));
#61573=CARTESIAN_POINT('Ctrl Pts',(4.13118752796397,1.,-0.733376589325634));
#61574=CARTESIAN_POINT('Ctrl Pts',(4.12666277572794,1.,-0.734698226767513));
#61575=CARTESIAN_POINT('Ctrl Pts',(4.12062919626082,1.,-0.736439634335347));
#61576=CARTESIAN_POINT('Ctrl Pts',(4.11308626953795,1.,-0.738581708229119));
#61577=CARTESIAN_POINT('Ctrl Pts',(4.1055424175856,1.,-0.740688998555152));
#61578=CARTESIAN_POINT('Ctrl Pts',(4.09799769702712,1.,-0.742761369690018));
#61579=CARTESIAN_POINT('Ctrl Pts',(4.09045220253011,1.,-0.744798649705514));
#61580=CARTESIAN_POINT('Ctrl Pts',(4.08290608094789,1.,-0.746800631490822));
#61581=CARTESIAN_POINT('Ctrl Pts',(4.07535951055363,1.,-0.748767076679177));
#61582=CARTESIAN_POINT('Ctrl Pts',(4.06781267241886,1.,-0.750697720483176));
#61583=CARTESIAN_POINT('Ctrl Pts',(4.06026572221399,1.,-0.752592276482869));
#61584=CARTESIAN_POINT('Ctrl Pts',(4.05271876688106,1.,-0.754450441816412));
#61585=CARTESIAN_POINT('Ctrl Pts',(4.04517182654344,1.,-0.756271902370187));
#61586=CARTESIAN_POINT('Ctrl Pts',(4.03762485803468,1.,-0.758056338885554));
#61587=CARTESIAN_POINT('Ctrl Pts',(4.0300778195465,1.,-0.759803433244166));
#61588=CARTESIAN_POINT('Ctrl Pts',(4.02253072741347,1.,-0.761512875859942));
#61589=CARTESIAN_POINT('Ctrl Pts',(4.01498370680434,1.,-0.763184371182827));
#61590=CARTESIAN_POINT('Ctrl Pts',(4.00743706791366,1.,-0.764817648784947));
#61591=CARTESIAN_POINT('Ctrl Pts',(3.99989129179464,1.,-0.766412457135786));
#61592=CARTESIAN_POINT('Ctrl Pts',(3.99234687880892,1.,-0.767968531377708));
#61593=CARTESIAN_POINT('Ctrl Pts',(3.98480422348403,1.,-0.76948556624546));
#61594=CARTESIAN_POINT('Ctrl Pts',(3.97726349165507,1.,-0.770963190030504));
#61595=CARTESIAN_POINT('Ctrl Pts',(3.96972446532832,1.,-0.772400931772239));
#61596=CARTESIAN_POINT('Ctrl Pts',(3.96218649639876,1.,-0.773798212026683));
#61597=CARTESIAN_POINT('Ctrl Pts',(3.95464885452364,1.,-0.775154418039442));
#61598=CARTESIAN_POINT('Ctrl Pts',(3.94711101619471,1.,-0.77646896669796));
#61599=CARTESIAN_POINT('Ctrl Pts',(3.93957296768098,1.,-0.77774137056855));
#61600=CARTESIAN_POINT('Ctrl Pts',(3.93203552473153,1.,-0.778971308134786));
#61601=CARTESIAN_POINT('Ctrl Pts',(3.92450058323799,1.,-0.780158678615507));
#61602=CARTESIAN_POINT('Ctrl Pts',(3.9169703605466,1.,-0.781303428618344));
#61603=CARTESIAN_POINT('Ctrl Pts',(3.90944671004536,1.,-0.782405395622759));
#61604=CARTESIAN_POINT('Ctrl Pts',(3.90193039043971,1.,-0.783464141529083));
#61605=CARTESIAN_POINT('Ctrl Pts',(3.89442039235105,1.,-0.784478799358336));
#61606=CARTESIAN_POINT('Ctrl Pts',(3.88691313167399,1.,-0.785447890340723));
#61607=CARTESIAN_POINT('Ctrl Pts',(3.87940402818186,1.,-0.786369675812592));
#61608=CARTESIAN_POINT('Ctrl Pts',(3.87188916600905,1.,-0.787242527617981));
#61609=CARTESIAN_POINT('Ctrl Pts',(3.86436702561342,1.,-0.788065315093771));
#61610=CARTESIAN_POINT('Ctrl Pts',(3.85683995872536,1.,-0.788837734090688));
#61611=CARTESIAN_POINT('Ctrl Pts',(3.8493163780891,1.,-0.789560798155619));
#61612=CARTESIAN_POINT('Ctrl Pts',(3.84180762342476,1.,-0.790236124191289));
#61613=CARTESIAN_POINT('Ctrl Pts',(3.83432392054804,1.,-0.79086501270534));
#61614=CARTESIAN_POINT('Ctrl Pts',(3.82687033899799,1.,-0.791447528662381));
#61615=CARTESIAN_POINT('Ctrl Pts',(3.81944345442237,1.,-0.791981740718607));
#61616=CARTESIAN_POINT('Ctrl Pts',(3.81202588694726,1.,-0.792462483517568));
#61617=CARTESIAN_POINT('Ctrl Pts',(3.80459229925598,1.,-0.792882695234693));
#61618=CARTESIAN_POINT('Ctrl Pts',(3.79711921389862,1.,-0.793235612973201));
#61619=CARTESIAN_POINT('Ctrl Pts',(3.78959439439222,1.,-0.793516871680966));
#61620=CARTESIAN_POINT('Ctrl Pts',(3.78202460377617,1.,-0.79372623578134));
#61621=CARTESIAN_POINT('Ctrl Pts',(3.77444863801264,1.,-0.793870523787515));
#61622=CARTESIAN_POINT('Ctrl Pts',(3.76692626931184,1.,-0.793961083689141));
#61623=CARTESIAN_POINT('Ctrl Pts',(3.75951468666325,1.,-0.794008429135047));
#61624=CARTESIAN_POINT('Ctrl Pts',(3.75224692493895,1.,-0.794017347371441));
#61625=CARTESIAN_POINT('Ctrl Pts',(3.74511357728827,1.,-0.79398270045988));
#61626=CARTESIAN_POINT('Ctrl Pts',(3.73803280541576,1.,-0.793882700936791));
#61627=CARTESIAN_POINT('Ctrl Pts',(3.7308691469564,1.,-0.793682750269348));
#61628=CARTESIAN_POINT('Ctrl Pts',(3.7234879729357,1.,-0.793347023783871));
#61629=CARTESIAN_POINT('Ctrl Pts',(3.7158024239604,1.,-0.792848377370116));
#61630=CARTESIAN_POINT('Ctrl Pts',(3.70781724021879,1.,-0.792177688845968));
#61631=CARTESIAN_POINT('Ctrl Pts',(3.69968940808982,1.,-0.791356575696509));
#61632=CARTESIAN_POINT('Ctrl Pts',(3.69172044327754,1.,-0.79043628498958));
#61633=CARTESIAN_POINT('Ctrl Pts',(3.68428439784285,1.,-0.789483546065159));
#61634=CARTESIAN_POINT('Ctrl Pts',(3.67777119516438,1.,-0.788569566220663));
#61635=CARTESIAN_POINT('Ctrl Pts',(3.672529236635,1.,-0.787758799995427));
#61636=CARTESIAN_POINT('Ctrl Pts',(3.66907505398769,1.,-0.787145041181589));
#61637=CARTESIAN_POINT('Ctrl Pts',(3.66743103898844,1.,-0.7867743371985));
#61638=CARTESIAN_POINT('Ctrl Pts',(3.66680946938396,1.,-0.78656591955989));
#61639=CARTESIAN_POINT('Ctrl Pts',(3.66664310415236,1.,-0.786459983896781));
#61640=CARTESIAN_POINT('Ctrl Pts',(3.66661143271648,1.,-0.786422660833743));
#61641=CARTESIAN_POINT('',(4.13571194405636,0.,-0.73204283740062));
#61642=CARTESIAN_POINT('Origin',(4.15950947128175,0.,-0.581791163835815));
#61643=CARTESIAN_POINT('',(4.15950947128175,1.,-0.581791163835815));
#61644=CARTESIAN_POINT('',(4.13571194405636,1.,-0.73204283740062));
#61645=CARTESIAN_POINT('',(4.15950947128175,0.,-0.581791163835815));
#61646=CARTESIAN_POINT('Ctrl Pts',(3.73016218570874,-1.,-0.385214314776329));
#61647=CARTESIAN_POINT('Ctrl Pts',(3.73016218570874,1.,-0.385214314776329));
#61648=CARTESIAN_POINT('Ctrl Pts',(3.73010668803185,-1.,-0.385147278814804));
#61649=CARTESIAN_POINT('Ctrl Pts',(3.73010668803185,1.,-0.385147278814804));
#61650=CARTESIAN_POINT('Ctrl Pts',(3.73015851028729,-1.,-0.385047711603887));
#61651=CARTESIAN_POINT('Ctrl Pts',(3.73015851028729,1.,-0.385047711603887));
#61652=CARTESIAN_POINT('Ctrl Pts',(3.73072465900727,-1.,-0.385001870183842));
#61653=CARTESIAN_POINT('Ctrl Pts',(3.73072465900727,1.,-0.385001870183842));
#61654=CARTESIAN_POINT('Ctrl Pts',(3.73245705639337,-1.,-0.385147887989515));
#61655=CARTESIAN_POINT('Ctrl Pts',(3.73245705639337,1.,-0.385147887989515));
#61656=CARTESIAN_POINT('Ctrl Pts',(3.73621371845475,-1.,-0.385670806454744));
#61657=CARTESIAN_POINT('Ctrl Pts',(3.73621371845475,1.,-0.385670806454744));
#61658=CARTESIAN_POINT('Ctrl Pts',(3.74144965781088,-1.,-0.386519576222036));
#61659=CARTESIAN_POINT('Ctrl Pts',(3.74144965781088,1.,-0.386519576222036));
#61660=CARTESIAN_POINT('Ctrl Pts',(3.74792651696269,-1.,-0.387663020050396));
#61661=CARTESIAN_POINT('Ctrl Pts',(3.74792651696269,1.,-0.387663020050396));
#61662=CARTESIAN_POINT('Ctrl Pts',(3.75529302894757,-1.,-0.389054775898251));
#61663=CARTESIAN_POINT('Ctrl Pts',(3.75529302894757,1.,-0.389054775898251));
#61664=CARTESIAN_POINT('Ctrl Pts',(3.76315635032993,-1.,-0.390642072979259));
#61665=CARTESIAN_POINT('Ctrl Pts',(3.76315635032993,1.,-0.390642072979259));
#61666=CARTESIAN_POINT('Ctrl Pts',(3.77114011595892,-1.,-0.392372786223347));
#61667=CARTESIAN_POINT('Ctrl Pts',(3.77114011595892,1.,-0.392372786223347));
#61668=CARTESIAN_POINT('Ctrl Pts',(3.77894173114368,-1.,-0.394202481011595));
#61669=CARTESIAN_POINT('Ctrl Pts',(3.77894173114368,1.,-0.394202481011595));
#61670=CARTESIAN_POINT('Ctrl Pts',(3.78640521279479,-1.,-0.396103205335029));
#61671=CARTESIAN_POINT('Ctrl Pts',(3.78640521279479,1.,-0.396103205335029));
#61672=CARTESIAN_POINT('Ctrl Pts',(3.79352887163457,-1.,-0.398064818684159));
#61673=CARTESIAN_POINT('Ctrl Pts',(3.79352887163457,1.,-0.398064818684159));
#61674=CARTESIAN_POINT('Ctrl Pts',(3.80040370384659,-1.,-0.400088346504727));
#61675=CARTESIAN_POINT('Ctrl Pts',(3.80040370384659,1.,-0.400088346504727));
#61676=CARTESIAN_POINT('Ctrl Pts',(3.80716881962763,-1.,-0.402181320148475));
#61677=CARTESIAN_POINT('Ctrl Pts',(3.80716881962763,1.,-0.402181320148475));
#61678=CARTESIAN_POINT('Ctrl Pts',(3.81396374287762,-1.,-0.404352694628237));
#61679=CARTESIAN_POINT('Ctrl Pts',(3.81396374287762,1.,-0.404352694628237));
#61680=CARTESIAN_POINT('Ctrl Pts',(3.82087303913741,-1.,-0.406607038258907));
#61681=CARTESIAN_POINT('Ctrl Pts',(3.82087303913741,1.,-0.406607038258907));
#61682=CARTESIAN_POINT('Ctrl Pts',(3.82790724256397,-1.,-0.408942371447377));
#61683=CARTESIAN_POINT('Ctrl Pts',(3.82790724256397,1.,-0.408942371447377));
#61684=CARTESIAN_POINT('Ctrl Pts',(3.83503345578645,-1.,-0.41135303879846));
#61685=CARTESIAN_POINT('Ctrl Pts',(3.83503345578645,1.,-0.41135303879846));
#61686=CARTESIAN_POINT('Ctrl Pts',(3.84219403994742,-1.,-0.413831367016727));
#61687=CARTESIAN_POINT('Ctrl Pts',(3.84219403994742,1.,-0.413831367016727));
#61688=CARTESIAN_POINT('Ctrl Pts',(3.8493286415751,-1.,-0.41636967805292));
#61689=CARTESIAN_POINT('Ctrl Pts',(3.8493286415751,1.,-0.41636967805292));
#61690=CARTESIAN_POINT('Ctrl Pts',(3.85639825648031,-1.,-0.41896246808681));
#61691=CARTESIAN_POINT('Ctrl Pts',(3.85639825648031,1.,-0.41896246808681));
#61692=CARTESIAN_POINT('Ctrl Pts',(3.86339652542749,-1.,-0.421607423177576));
#61693=CARTESIAN_POINT('Ctrl Pts',(3.86339652542749,1.,-0.421607423177576));
#61694=CARTESIAN_POINT('Ctrl Pts',(3.87033643487882,-1.,-0.424304173195143));
#61695=CARTESIAN_POINT('Ctrl Pts',(3.87033643487882,1.,-0.424304173195143));
#61696=CARTESIAN_POINT('Ctrl Pts',(3.87724240306609,-1.,-0.427053541173469));
#61697=CARTESIAN_POINT('Ctrl Pts',(3.87724240306609,1.,-0.427053541173469));
#61698=CARTESIAN_POINT('Ctrl Pts',(3.88414070943334,-1.,-0.429856640579734));
#61699=CARTESIAN_POINT('Ctrl Pts',(3.88414070943334,1.,-0.429856640579734));
#61700=CARTESIAN_POINT('Ctrl Pts',(3.89104947940592,-1.,-0.43271392954444));
#61701=CARTESIAN_POINT('Ctrl Pts',(3.89104947940592,1.,-0.43271392954444));
#61702=CARTESIAN_POINT('Ctrl Pts',(3.8979725665544,-1.,-0.435624629433506));
#61703=CARTESIAN_POINT('Ctrl Pts',(3.8979725665544,1.,-0.435624629433506));
#61704=CARTESIAN_POINT('Ctrl Pts',(3.90490512938546,-1.,-0.438587235458234));
#61705=CARTESIAN_POINT('Ctrl Pts',(3.90490512938546,1.,-0.438587235458234));
#61706=CARTESIAN_POINT('Ctrl Pts',(3.91183704069146,-1.,-0.441599824524048));
#61707=CARTESIAN_POINT('Ctrl Pts',(3.91183704069146,1.,-0.441599824524048));
#61708=CARTESIAN_POINT('Ctrl Pts',(3.91875701610721,-1.,-0.444660430230593));
#61709=CARTESIAN_POINT('Ctrl Pts',(3.91875701610721,1.,-0.444660430230593));
#61710=CARTESIAN_POINT('Ctrl Pts',(3.92565674143424,-1.,-0.447767416837297));
#61711=CARTESIAN_POINT('Ctrl Pts',(3.92565674143424,1.,-0.447767416837297));
#61712=CARTESIAN_POINT('Ctrl Pts',(3.93253407403128,-1.,-0.450919768356347));
#61713=CARTESIAN_POINT('Ctrl Pts',(3.93253407403128,1.,-0.450919768356347));
#61714=CARTESIAN_POINT('Ctrl Pts',(3.93939080846298,-1.,-0.454116879027576));
#61715=CARTESIAN_POINT('Ctrl Pts',(3.93939080846298,1.,-0.454116879027576));
#61716=CARTESIAN_POINT('Ctrl Pts',(3.94623117206675,-1.,-0.457358410451674));
#61717=CARTESIAN_POINT('Ctrl Pts',(3.94623117206675,1.,-0.457358410451674));
#61718=CARTESIAN_POINT('Ctrl Pts',(3.95306005817363,-1.,-0.460644124429119));
#61719=CARTESIAN_POINT('Ctrl Pts',(3.95306005817363,1.,-0.460644124429119));
#61720=CARTESIAN_POINT('Ctrl Pts',(3.95988133243543,-1.,-0.463973722115745));
#61721=CARTESIAN_POINT('Ctrl Pts',(3.95988133243543,1.,-0.463973722115745));
#61722=CARTESIAN_POINT('Ctrl Pts',(3.96669622273946,-1.,-0.467346690880672));
#61723=CARTESIAN_POINT('Ctrl Pts',(3.96669622273946,1.,-0.467346690880672));
#61724=CARTESIAN_POINT('Ctrl Pts',(3.97350414289415,-1.,-0.470762379613478));
#61725=CARTESIAN_POINT('Ctrl Pts',(3.97350414289415,1.,-0.470762379613478));
#61726=CARTESIAN_POINT('Ctrl Pts',(3.9803033804443,-1.,-0.474220061019542));
#61727=CARTESIAN_POINT('Ctrl Pts',(3.9803033804443,1.,-0.474220061019542));
#61728=CARTESIAN_POINT('Ctrl Pts',(3.98709184306743,-1.,-0.477718999122033));
#61729=CARTESIAN_POINT('Ctrl Pts',(3.98709184306743,1.,-0.477718999122033));
#61730=CARTESIAN_POINT('Ctrl Pts',(3.99386775880655,-1.,-0.481258512209638));
#61731=CARTESIAN_POINT('Ctrl Pts',(3.99386775880655,1.,-0.481258512209638));
#61732=CARTESIAN_POINT('Ctrl Pts',(4.00063045119234,-1.,-0.484838042421754));
#61733=CARTESIAN_POINT('Ctrl Pts',(4.00063045119234,1.,-0.484838042421754));
#61734=CARTESIAN_POINT('Ctrl Pts',(4.0073800839092,-1.,-0.488457130424531));
#61735=CARTESIAN_POINT('Ctrl Pts',(4.0073800839092,1.,-0.488457130424531));
#61736=CARTESIAN_POINT('Ctrl Pts',(4.01411733503486,-1.,-0.492115383417931));
#61737=CARTESIAN_POINT('Ctrl Pts',(4.01411733503486,1.,-0.492115383417931));
#61738=CARTESIAN_POINT('Ctrl Pts',(4.02084308851813,-1.,-0.495812444326223));
#61739=CARTESIAN_POINT('Ctrl Pts',(4.02084308851813,1.,-0.495812444326223));
#61740=CARTESIAN_POINT('Ctrl Pts',(4.0275581398015,-1.,-0.49954796234089));
#61741=CARTESIAN_POINT('Ctrl Pts',(4.0275581398015,1.,-0.49954796234089));
#61742=CARTESIAN_POINT('Ctrl Pts',(4.0342628417439,-1.,-0.503321556915514));
#61743=CARTESIAN_POINT('Ctrl Pts',(4.0342628417439,1.,-0.503321556915514));
#61744=CARTESIAN_POINT('Ctrl Pts',(4.04095715149074,-1.,-0.507132823288362));
#61745=CARTESIAN_POINT('Ctrl Pts',(4.04095715149074,1.,-0.507132823288362));
#61746=CARTESIAN_POINT('Ctrl Pts',(4.04764078815591,-1.,-0.510981349219174));
#61747=CARTESIAN_POINT('Ctrl Pts',(4.04764078815591,1.,-0.510981349219174));
#61748=CARTESIAN_POINT('Ctrl Pts',(4.05431335771261,-1.,-0.514866728193104));
#61749=CARTESIAN_POINT('Ctrl Pts',(4.05431335771261,1.,-0.514866728193104));
#61750=CARTESIAN_POINT('Ctrl Pts',(4.06097448037934,-1.,-0.51878857233681));
#61751=CARTESIAN_POINT('Ctrl Pts',(4.06097448037934,1.,-0.51878857233681));
#61752=CARTESIAN_POINT('Ctrl Pts',(4.06762394471075,-1.,-0.522746528602768));
#61753=CARTESIAN_POINT('Ctrl Pts',(4.06762394471075,1.,-0.522746528602768));
#61754=CARTESIAN_POINT('Ctrl Pts',(4.07426172299496,-1.,-0.526740277227));
#61755=CARTESIAN_POINT('Ctrl Pts',(4.07426172299496,1.,-0.526740277227));
#61756=CARTESIAN_POINT('Ctrl Pts',(4.08088789536488,-1.,-0.530769518728076));
#61757=CARTESIAN_POINT('Ctrl Pts',(4.08088789536488,1.,-0.530769518728076));
#61758=CARTESIAN_POINT('Ctrl Pts',(4.08750259988693,-1.,-0.534833963477));
#61759=CARTESIAN_POINT('Ctrl Pts',(4.08750259988693,1.,-0.534833963477));
#61760=CARTESIAN_POINT('Ctrl Pts',(4.09410597627116,-1.,-0.538933321179921));
#61761=CARTESIAN_POINT('Ctrl Pts',(4.09410597627116,1.,-0.538933321179921));
#61762=CARTESIAN_POINT('Ctrl Pts',(4.10069810244473,-1.,-0.543067286878457));
#61763=CARTESIAN_POINT('Ctrl Pts',(4.10069810244473,1.,-0.543067286878457));
#61764=CARTESIAN_POINT('Ctrl Pts',(4.1072789702877,-1.,-0.54723553948676));
#61765=CARTESIAN_POINT('Ctrl Pts',(4.1072789702877,1.,-0.54723553948676));
#61766=CARTESIAN_POINT('Ctrl Pts',(4.11384852025578,-1.,-0.551437758498247));
#61767=CARTESIAN_POINT('Ctrl Pts',(4.11384852025578,1.,-0.551437758498247));
#61768=CARTESIAN_POINT('Ctrl Pts',(4.1204066619623,-1.,-0.555673636130778));
#61769=CARTESIAN_POINT('Ctrl Pts',(4.1204066619623,1.,-0.555673636130778));
#61770=CARTESIAN_POINT('Ctrl Pts',(4.12695329951859,-1.,-0.559942890594628));
#61771=CARTESIAN_POINT('Ctrl Pts',(4.12695329951859,1.,-0.559942890594628));
#61772=CARTESIAN_POINT('Ctrl Pts',(4.13348835726086,-1.,-0.564245279535706));
#61773=CARTESIAN_POINT('Ctrl Pts',(4.13348835726086,1.,-0.564245279535706));
#61774=CARTESIAN_POINT('Ctrl Pts',(4.14001179828669,-1.,-0.568580610187116));
#61775=CARTESIAN_POINT('Ctrl Pts',(4.14001179828669,1.,-0.568580610187116));
#61776=CARTESIAN_POINT('Ctrl Pts',(4.14652361065787,-1.,-0.572948736066277));
#61777=CARTESIAN_POINT('Ctrl Pts',(4.14652361065787,1.,-0.572948736066277));
#61778=CARTESIAN_POINT('Ctrl Pts',(4.1517237611974,-1.,-0.576469391673917));
#61779=CARTESIAN_POINT('Ctrl Pts',(4.1517237611974,1.,-0.576469391673917));
#61780=CARTESIAN_POINT('Ctrl Pts',(4.15561864787379,-1.,-0.579124568912544));
#61781=CARTESIAN_POINT('Ctrl Pts',(4.15561864787379,1.,-0.579124568912544));
#61782=CARTESIAN_POINT('Ctrl Pts',(4.15821291712391,-1.,-0.580901211462913));
#61783=CARTESIAN_POINT('Ctrl Pts',(4.15821291712391,1.,-0.580901211462913));
#61784=CARTESIAN_POINT('Ctrl Pts',(4.15950947128175,-1.,-0.581791163835815));
#61785=CARTESIAN_POINT('Ctrl Pts',(4.15950947128175,1.,-0.581791163835815));
#61786=CARTESIAN_POINT('',(3.73017266276632,1.,-0.385112848332548));
#61787=CARTESIAN_POINT('Ctrl Pts',(3.73017266276632,-1.,-0.385112848332549));
#61788=CARTESIAN_POINT('Ctrl Pts',(3.73017266276632,-0.666666666666667,
-0.385112848332549));
#61789=CARTESIAN_POINT('Ctrl Pts',(3.73017266276632,-0.333333333333333,
-0.385112848332549));
#61790=CARTESIAN_POINT('Ctrl Pts',(3.73017266276632,0.333333333333333,-0.385112848332549));
#61791=CARTESIAN_POINT('Ctrl Pts',(3.73017266276632,0.666666666666667,-0.38511284833255));
#61792=CARTESIAN_POINT('Ctrl Pts',(3.73017266276632,1.,-0.38511284833255));
#61793=CARTESIAN_POINT('Ctrl Pts',(3.73017266276632,1.,-0.385112848332549));
#61794=CARTESIAN_POINT('Ctrl Pts',(3.73021431755218,1.,-0.385087139001609));
#61795=CARTESIAN_POINT('Ctrl Pts',(3.73040527620929,1.,-0.385037797882046));
#61796=CARTESIAN_POINT('Ctrl Pts',(3.731060828624,1.,-0.385031656499142));
#61797=CARTESIAN_POINT('Ctrl Pts',(3.73273893363318,1.,-0.385187124633965));
#61798=CARTESIAN_POINT('Ctrl Pts',(3.73621371845475,1.,-0.385670806454744));
#61799=CARTESIAN_POINT('Ctrl Pts',(3.74144965781088,1.,-0.386519576222036));
#61800=CARTESIAN_POINT('Ctrl Pts',(3.74792651696269,1.,-0.387663020050396));
#61801=CARTESIAN_POINT('Ctrl Pts',(3.75529302894757,1.,-0.389054775898251));
#61802=CARTESIAN_POINT('Ctrl Pts',(3.76315635032993,1.,-0.390642072979259));
#61803=CARTESIAN_POINT('Ctrl Pts',(3.77114011595892,1.,-0.392372786223347));
#61804=CARTESIAN_POINT('Ctrl Pts',(3.77894173114368,1.,-0.394202481011595));
#61805=CARTESIAN_POINT('Ctrl Pts',(3.78640521279479,1.,-0.396103205335029));
#61806=CARTESIAN_POINT('Ctrl Pts',(3.79352887163457,1.,-0.398064818684159));
#61807=CARTESIAN_POINT('Ctrl Pts',(3.80040370384659,1.,-0.400088346504727));
#61808=CARTESIAN_POINT('Ctrl Pts',(3.80716881962763,1.,-0.402181320148475));
#61809=CARTESIAN_POINT('Ctrl Pts',(3.81396374287762,1.,-0.404352694628237));
#61810=CARTESIAN_POINT('Ctrl Pts',(3.82087303913741,1.,-0.406607038258907));
#61811=CARTESIAN_POINT('Ctrl Pts',(3.82790724256397,1.,-0.408942371447377));
#61812=CARTESIAN_POINT('Ctrl Pts',(3.83503345578645,1.,-0.41135303879846));
#61813=CARTESIAN_POINT('Ctrl Pts',(3.84219403994742,1.,-0.413831367016727));
#61814=CARTESIAN_POINT('Ctrl Pts',(3.8493286415751,1.,-0.41636967805292));
#61815=CARTESIAN_POINT('Ctrl Pts',(3.85639825648031,1.,-0.41896246808681));
#61816=CARTESIAN_POINT('Ctrl Pts',(3.86339652542749,1.,-0.421607423177576));
#61817=CARTESIAN_POINT('Ctrl Pts',(3.87033643487882,1.,-0.424304173195143));
#61818=CARTESIAN_POINT('Ctrl Pts',(3.87724240306609,1.,-0.427053541173469));
#61819=CARTESIAN_POINT('Ctrl Pts',(3.88414070943334,1.,-0.429856640579734));
#61820=CARTESIAN_POINT('Ctrl Pts',(3.89104947940592,1.,-0.43271392954444));
#61821=CARTESIAN_POINT('Ctrl Pts',(3.8979725665544,1.,-0.435624629433506));
#61822=CARTESIAN_POINT('Ctrl Pts',(3.90490512938546,1.,-0.438587235458234));
#61823=CARTESIAN_POINT('Ctrl Pts',(3.91183704069146,1.,-0.441599824524048));
#61824=CARTESIAN_POINT('Ctrl Pts',(3.91875701610721,1.,-0.444660430230593));
#61825=CARTESIAN_POINT('Ctrl Pts',(3.92565674143424,1.,-0.447767416837297));
#61826=CARTESIAN_POINT('Ctrl Pts',(3.93253407403128,1.,-0.450919768356347));
#61827=CARTESIAN_POINT('Ctrl Pts',(3.93939080846298,1.,-0.454116879027576));
#61828=CARTESIAN_POINT('Ctrl Pts',(3.94623117206675,1.,-0.457358410451674));
#61829=CARTESIAN_POINT('Ctrl Pts',(3.95306005817363,1.,-0.460644124429119));
#61830=CARTESIAN_POINT('Ctrl Pts',(3.95988133243543,1.,-0.463973722115745));
#61831=CARTESIAN_POINT('Ctrl Pts',(3.96669622273946,1.,-0.467346690880672));
#61832=CARTESIAN_POINT('Ctrl Pts',(3.97350414289415,1.,-0.470762379613478));
#61833=CARTESIAN_POINT('Ctrl Pts',(3.9803033804443,1.,-0.474220061019542));
#61834=CARTESIAN_POINT('Ctrl Pts',(3.98709184306743,1.,-0.477718999122033));
#61835=CARTESIAN_POINT('Ctrl Pts',(3.99386775880655,1.,-0.481258512209638));
#61836=CARTESIAN_POINT('Ctrl Pts',(4.00063045119234,1.,-0.484838042421754));
#61837=CARTESIAN_POINT('Ctrl Pts',(4.0073800839092,1.,-0.488457130424531));
#61838=CARTESIAN_POINT('Ctrl Pts',(4.01411733503486,1.,-0.492115383417931));
#61839=CARTESIAN_POINT('Ctrl Pts',(4.02084308851813,1.,-0.495812444326223));
#61840=CARTESIAN_POINT('Ctrl Pts',(4.0275581398015,1.,-0.49954796234089));
#61841=CARTESIAN_POINT('Ctrl Pts',(4.0342628417439,1.,-0.503321556915514));
#61842=CARTESIAN_POINT('Ctrl Pts',(4.04095715149074,1.,-0.507132823288362));
#61843=CARTESIAN_POINT('Ctrl Pts',(4.04764078815591,1.,-0.510981349219174));
#61844=CARTESIAN_POINT('Ctrl Pts',(4.05431335771261,1.,-0.514866728193104));
#61845=CARTESIAN_POINT('Ctrl Pts',(4.06097448037934,1.,-0.51878857233681));
#61846=CARTESIAN_POINT('Ctrl Pts',(4.06762394471075,1.,-0.522746528602768));
#61847=CARTESIAN_POINT('Ctrl Pts',(4.07426172299496,1.,-0.526740277227));
#61848=CARTESIAN_POINT('Ctrl Pts',(4.08088789536488,1.,-0.530769518728076));
#61849=CARTESIAN_POINT('Ctrl Pts',(4.08750259988693,1.,-0.534833963477));
#61850=CARTESIAN_POINT('Ctrl Pts',(4.09410597627116,1.,-0.538933321179921));
#61851=CARTESIAN_POINT('Ctrl Pts',(4.10069810244473,1.,-0.543067286878457));
#61852=CARTESIAN_POINT('Ctrl Pts',(4.1072789702877,1.,-0.54723553948676));
#61853=CARTESIAN_POINT('Ctrl Pts',(4.11384852025578,1.,-0.551437758498247));
#61854=CARTESIAN_POINT('Ctrl Pts',(4.1204066619623,1.,-0.555673636130778));
#61855=CARTESIAN_POINT('Ctrl Pts',(4.12695329951859,1.,-0.559942890594628));
#61856=CARTESIAN_POINT('Ctrl Pts',(4.13348835726086,1.,-0.564245279535706));
#61857=CARTESIAN_POINT('Ctrl Pts',(4.14001179828669,1.,-0.568580610187116));
#61858=CARTESIAN_POINT('Ctrl Pts',(4.14652361065787,1.,-0.572948736066277));
#61859=CARTESIAN_POINT('Ctrl Pts',(4.1517237611974,1.,-0.576469391673917));
#61860=CARTESIAN_POINT('Ctrl Pts',(4.15561864787379,1.,-0.579124568912544));
#61861=CARTESIAN_POINT('Ctrl Pts',(4.15821291712391,1.,-0.580901211462913));
#61862=CARTESIAN_POINT('Ctrl Pts',(4.15950947128175,1.,-0.581791163835815));
#61863=CARTESIAN_POINT('Origin',(0.,0.,0.));
#61864=CARTESIAN_POINT('',(3.74449296982994,1.,-0.203156094897896));
#61865=CARTESIAN_POINT('Origin',(0.,1.,0.));
#61866=CARTESIAN_POINT('Ctrl Pts',(3.74449296982994,1.,-0.203156094897896));
#61867=CARTESIAN_POINT('Ctrl Pts',(3.74449296982994,0.666666666666667,-0.203156094897896));
#61868=CARTESIAN_POINT('Ctrl Pts',(3.74449296982994,0.333333333333333,-0.203156094897896));
#61869=CARTESIAN_POINT('Ctrl Pts',(3.74449296982994,-0.333333333333333,
-0.203156094897896));
#61870=CARTESIAN_POINT('Ctrl Pts',(3.74449296982994,-0.666666666666667,
-0.203156094897895));
#61871=CARTESIAN_POINT('Ctrl Pts',(3.74449296982994,-1.,-0.203156094897895));
#61872=CARTESIAN_POINT('Ctrl Pts',(3.74449849461127,-1.,0.20305423869972));
#61873=CARTESIAN_POINT('Ctrl Pts',(3.74449849461127,1.,0.20305423869972));
#61874=CARTESIAN_POINT('Ctrl Pts',(3.7444331934681,-1.,0.203111767587923));
#61875=CARTESIAN_POINT('Ctrl Pts',(3.7444331934681,1.,0.203111767587923));
#61876=CARTESIAN_POINT('Ctrl Pts',(3.7444688019622,-1.,0.203218215748058));
#61877=CARTESIAN_POINT('Ctrl Pts',(3.7444688019622,1.,0.203218215748058));
#61878=CARTESIAN_POINT('Ctrl Pts',(3.74502080927395,-1.,0.203352057956297));
#61879=CARTESIAN_POINT('Ctrl Pts',(3.74502080927395,1.,0.203352057956297));
#61880=CARTESIAN_POINT('Ctrl Pts',(3.7467547201908,-1.,0.203478844530446));
#61881=CARTESIAN_POINT('Ctrl Pts',(3.7467547201908,1.,0.203478844530446));
#61882=CARTESIAN_POINT('Ctrl Pts',(3.75054693397875,-1.,0.203550035479166));
#61883=CARTESIAN_POINT('Ctrl Pts',(3.75054693397875,1.,0.203550035479166));
#61884=CARTESIAN_POINT('Ctrl Pts',(3.75585118707734,-1.,0.203530796848321));
#61885=CARTESIAN_POINT('Ctrl Pts',(3.75585118707734,1.,0.203530796848321));
#61886=CARTESIAN_POINT('Ctrl Pts',(3.76242717936885,-1.,0.203414634707478));
#61887=CARTESIAN_POINT('Ctrl Pts',(3.76242717936885,1.,0.203414634707478));
#61888=CARTESIAN_POINT('Ctrl Pts',(3.7699207159487,-1.,0.203192390045164));
#61889=CARTESIAN_POINT('Ctrl Pts',(3.7699207159487,1.,0.203192390045164));
#61890=CARTESIAN_POINT('Ctrl Pts',(3.77793553476614,-1.,0.20285472969908));
#61891=CARTESIAN_POINT('Ctrl Pts',(3.77793553476614,1.,0.20285472969908));
#61892=CARTESIAN_POINT('Ctrl Pts',(3.78609175019242,-1.,0.20239426051216));
#61893=CARTESIAN_POINT('Ctrl Pts',(3.78609175019242,1.,0.20239426051216));
#61894=CARTESIAN_POINT('Ctrl Pts',(3.7940835418736,-1.,0.201807533800837));
#61895=CARTESIAN_POINT('Ctrl Pts',(3.7940835418736,1.,0.201807533800837));
#61896=CARTESIAN_POINT('Ctrl Pts',(3.80175247447337,-1.,0.201097756307325));
#61897=CARTESIAN_POINT('Ctrl Pts',(3.80175247447337,1.,0.201097756307325));
#61898=CARTESIAN_POINT('Ctrl Pts',(3.80909529318669,-1.,0.200274679433364));
#61899=CARTESIAN_POINT('Ctrl Pts',(3.80909529318669,1.,0.200274679433364));
#61900=CARTESIAN_POINT('Ctrl Pts',(3.81620203429815,-1.,0.199351525297447));
#61901=CARTESIAN_POINT('Ctrl Pts',(3.81620203429815,1.,0.199351525297447));
#61902=CARTESIAN_POINT('Ctrl Pts',(3.82321127349016,-1.,0.198342616900486));
#61903=CARTESIAN_POINT('Ctrl Pts',(3.82321127349016,1.,0.198342616900486));
#61904=CARTESIAN_POINT('Ctrl Pts',(3.83026221776456,-1.,0.197260935827361));
#61905=CARTESIAN_POINT('Ctrl Pts',(3.83026221776456,1.,0.197260935827361));
#61906=CARTESIAN_POINT('Ctrl Pts',(3.83743910616195,-1.,0.196115198971858));
#61907=CARTESIAN_POINT('Ctrl Pts',(3.83743910616195,1.,0.196115198971858));
#61908=CARTESIAN_POINT('Ctrl Pts',(3.84475203346977,-1.,0.19490900946022));
#61909=CARTESIAN_POINT('Ctrl Pts',(3.84475203346977,1.,0.19490900946022));
#61910=CARTESIAN_POINT('Ctrl Pts',(3.85216762263966,-1.,0.193642806777722));
#61911=CARTESIAN_POINT('Ctrl Pts',(3.85216762263966,1.,0.193642806777722));
#61912=CARTESIAN_POINT('Ctrl Pts',(3.85962774407633,-1.,0.19231515304497));
#61913=CARTESIAN_POINT('Ctrl Pts',(3.85962774407633,1.,0.19231515304497));
#61914=CARTESIAN_POINT('Ctrl Pts',(3.86707158624783,-1.,0.190924190418619));
#61915=CARTESIAN_POINT('Ctrl Pts',(3.86707158624783,1.,0.190924190418619));
#61916=CARTESIAN_POINT('Ctrl Pts',(3.87445976418412,-1.,0.189469253358272));
#61917=CARTESIAN_POINT('Ctrl Pts',(3.87445976418412,1.,0.189469253358272));
#61918=CARTESIAN_POINT('Ctrl Pts',(3.88178563496228,-1.,0.187951632512684));
#61919=CARTESIAN_POINT('Ctrl Pts',(3.88178563496228,1.,0.187951632512684));
#61920=CARTESIAN_POINT('Ctrl Pts',(3.88906196725848,-1.,0.18637372498528));
#61921=CARTESIAN_POINT('Ctrl Pts',(3.88906196725848,1.,0.18637372498528));
#61922=CARTESIAN_POINT('Ctrl Pts',(3.89631300742646,-1.,0.184738537728042));
#61923=CARTESIAN_POINT('Ctrl Pts',(3.89631300742646,1.,0.184738537728042));
#61924=CARTESIAN_POINT('Ctrl Pts',(3.90356488555132,-1.,0.18304908199319));
#61925=CARTESIAN_POINT('Ctrl Pts',(3.90356488555132,1.,0.18304908199319));
#61926=CARTESIAN_POINT('Ctrl Pts',(3.91083557557175,-1.,0.181307740731785));
#61927=CARTESIAN_POINT('Ctrl Pts',(3.91083557557175,1.,0.181307740731785));
#61928=CARTESIAN_POINT('Ctrl Pts',(3.91812876180926,-1.,0.179515885822881));
#61929=CARTESIAN_POINT('Ctrl Pts',(3.91812876180926,1.,0.179515885822881));
#61930=CARTESIAN_POINT('Ctrl Pts',(3.92543942697655,-1.,0.177674246152317));
#61931=CARTESIAN_POINT('Ctrl Pts',(3.92543942697655,1.,0.177674246152317));
#61932=CARTESIAN_POINT('Ctrl Pts',(3.93275726771042,-1.,0.175783136893867));
#61933=CARTESIAN_POINT('Ctrl Pts',(3.93275726771042,1.,0.175783136893867));
#61934=CARTESIAN_POINT('Ctrl Pts',(3.94007083096217,-1.,0.173842734974609));
#61935=CARTESIAN_POINT('Ctrl Pts',(3.94007083096217,1.,0.173842734974609));
#61936=CARTESIAN_POINT('Ctrl Pts',(3.94737164900868,-1.,0.17185335536924));
#61937=CARTESIAN_POINT('Ctrl Pts',(3.94737164900868,1.,0.17185335536924));
#61938=CARTESIAN_POINT('Ctrl Pts',(3.95465744665268,-1.,0.169815666374138));
#61939=CARTESIAN_POINT('Ctrl Pts',(3.95465744665268,1.,0.169815666374138));
#61940=CARTESIAN_POINT('Ctrl Pts',(3.96192990160296,-1.,0.167730547023319));
#61941=CARTESIAN_POINT('Ctrl Pts',(3.96192990160296,1.,0.167730547023319));
#61942=CARTESIAN_POINT('Ctrl Pts',(3.96919313621407,-1.,0.165598992851102));
#61943=CARTESIAN_POINT('Ctrl Pts',(3.96919313621407,1.,0.165598992851102));
#61944=CARTESIAN_POINT('Ctrl Pts',(3.97645194630943,-1.,0.163422004609999));
#61945=CARTESIAN_POINT('Ctrl Pts',(3.97645194630943,1.,0.163422004609999));
#61946=CARTESIAN_POINT('Ctrl Pts',(3.98371010319872,-1.,0.161200482186084));
#61947=CARTESIAN_POINT('Ctrl Pts',(3.98371010319872,1.,0.161200482186084));
#61948=CARTESIAN_POINT('Ctrl Pts',(3.99096873945878,-1.,0.158935123982793));
#61949=CARTESIAN_POINT('Ctrl Pts',(3.99096873945878,1.,0.158935123982793));
#61950=CARTESIAN_POINT('Ctrl Pts',(3.99822717425893,-1.,0.156626481393734));
#61951=CARTESIAN_POINT('Ctrl Pts',(3.99822717425893,1.,0.156626481393734));
#61952=CARTESIAN_POINT('Ctrl Pts',(4.00548360245319,-1.,0.15427500487231));
#61953=CARTESIAN_POINT('Ctrl Pts',(4.00548360245319,1.,0.15427500487231));
#61954=CARTESIAN_POINT('Ctrl Pts',(4.01273584234689,-1.,0.15188109402291));
#61955=CARTESIAN_POINT('Ctrl Pts',(4.01273584234689,1.,0.15188109402291));
#61956=CARTESIAN_POINT('Ctrl Pts',(4.01998203715564,-1.,0.149445144968706));
#61957=CARTESIAN_POINT('Ctrl Pts',(4.01998203715564,1.,0.149445144968706));
#61958=CARTESIAN_POINT('Ctrl Pts',(4.02722143146994,-1.,0.146967602878994));
#61959=CARTESIAN_POINT('Ctrl Pts',(4.02722143146994,1.,0.146967602878994));
#61960=CARTESIAN_POINT('Ctrl Pts',(4.03445411510333,-1.,0.144448947038344));
#61961=CARTESIAN_POINT('Ctrl Pts',(4.03445411510333,1.,0.144448947038344));
#61962=CARTESIAN_POINT('Ctrl Pts',(4.04168069633781,-1.,0.1418896714855));
#61963=CARTESIAN_POINT('Ctrl Pts',(4.04168069633781,1.,0.1418896714855));
#61964=CARTESIAN_POINT('Ctrl Pts',(4.04890199238036,-1.,0.139290267180057));
#61965=CARTESIAN_POINT('Ctrl Pts',(4.04890199238036,1.,0.139290267180057));
#61966=CARTESIAN_POINT('Ctrl Pts',(4.05611873400172,-1.,0.136651205046119));
#61967=CARTESIAN_POINT('Ctrl Pts',(4.05611873400172,1.,0.136651205046119));
#61968=CARTESIAN_POINT('Ctrl Pts',(4.06333121018596,-1.,0.133972916144244));
#61969=CARTESIAN_POINT('Ctrl Pts',(4.06333121018596,1.,0.133972916144244));
#61970=CARTESIAN_POINT('Ctrl Pts',(4.0705393152874,-1.,0.13125579354894));
#61971=CARTESIAN_POINT('Ctrl Pts',(4.0705393152874,1.,0.13125579354894));
#61972=CARTESIAN_POINT('Ctrl Pts',(4.07774270738954,-1.,0.128500200484837));
#61973=CARTESIAN_POINT('Ctrl Pts',(4.07774270738954,1.,0.128500200484837));
#61974=CARTESIAN_POINT('Ctrl Pts',(4.08494093372377,-1.,0.125706476822539));
#61975=CARTESIAN_POINT('Ctrl Pts',(4.08494093372377,1.,0.125706476822539));
#61976=CARTESIAN_POINT('Ctrl Pts',(4.09213355850756,-1.,0.122874946249106));
#61977=CARTESIAN_POINT('Ctrl Pts',(4.09213355850756,1.,0.122874946249106));
#61978=CARTESIAN_POINT('Ctrl Pts',(4.09932031767002,-1.,0.120005924388124));
#61979=CARTESIAN_POINT('Ctrl Pts',(4.09932031767002,1.,0.120005924388124));
#61980=CARTESIAN_POINT('Ctrl Pts',(4.10650113381833,-1.,0.117099722731648));
#61981=CARTESIAN_POINT('Ctrl Pts',(4.10650113381833,1.,0.117099722731648));
#61982=CARTESIAN_POINT('Ctrl Pts',(4.11367603924961,-1.,0.114156649609545));
#61983=CARTESIAN_POINT('Ctrl Pts',(4.11367603924961,1.,0.114156649609545));
#61984=CARTESIAN_POINT('Ctrl Pts',(4.1208451250225,-1.,0.111177012683346));
#61985=CARTESIAN_POINT('Ctrl Pts',(4.1208451250225,1.,0.111177012683346));
#61986=CARTESIAN_POINT('Ctrl Pts',(4.12800848371504,-1.,0.108161120528369));
#61987=CARTESIAN_POINT('Ctrl Pts',(4.12800848371504,1.,0.108161120528369));
#61988=CARTESIAN_POINT('Ctrl Pts',(4.13516614458895,-1.,0.105109286538945));
#61989=CARTESIAN_POINT('Ctrl Pts',(4.13516614458895,1.,0.105109286538945));
#61990=CARTESIAN_POINT('Ctrl Pts',(4.14231804939538,-1.,0.102021826577583));
#61991=CARTESIAN_POINT('Ctrl Pts',(4.14231804939538,1.,0.102021826577583));
#61992=CARTESIAN_POINT('Ctrl Pts',(4.14946408918485,-1.,0.0988990478901221));
#61993=CARTESIAN_POINT('Ctrl Pts',(4.14946408918485,1.,0.0988990478901221));
#61994=CARTESIAN_POINT('Ctrl Pts',(4.15660412653577,-1.,0.0957412403298002));
#61995=CARTESIAN_POINT('Ctrl Pts',(4.15660412653577,1.,0.0957412403298002));
#61996=CARTESIAN_POINT('Ctrl Pts',(4.16373802265839,-1.,0.0925486672167526));
#61997=CARTESIAN_POINT('Ctrl Pts',(4.16373802265839,1.,0.0925486672167526));
#61998=CARTESIAN_POINT('Ctrl Pts',(4.17086566490794,-1.,0.0893215560848644));
#61999=CARTESIAN_POINT('Ctrl Pts',(4.17086566490794,1.,0.0893215560848644));
#62000=CARTESIAN_POINT('Ctrl Pts',(4.17798698668094,-1.,0.0860600915549391));
#62001=CARTESIAN_POINT('Ctrl Pts',(4.17798698668094,1.,0.0860600915549391));
#62002=CARTESIAN_POINT('Ctrl Pts',(4.18510195327123,-1.,0.0827644164385674));
#62003=CARTESIAN_POINT('Ctrl Pts',(4.18510195327123,1.,0.0827644164385674));
#62004=CARTESIAN_POINT('Ctrl Pts',(4.19078883320504,-1.,0.0801005887114315));
#62005=CARTESIAN_POINT('Ctrl Pts',(4.19078883320504,1.,0.0801005887114315));
#62006=CARTESIAN_POINT('Ctrl Pts',(4.19505112859416,-1.,0.0780873956242392));
#62007=CARTESIAN_POINT('Ctrl Pts',(4.19505112859416,1.,0.0780873956242392));
#62008=CARTESIAN_POINT('Ctrl Pts',(4.1978913862118,-1.,0.0767384596141459));
#62009=CARTESIAN_POINT('Ctrl Pts',(4.1978913862118,1.,0.0767384596141459));
#62010=CARTESIAN_POINT('Ctrl Pts',(4.19931119685982,-1.,0.0760622897878241));
#62011=CARTESIAN_POINT('Ctrl Pts',(4.19931119685982,1.,0.0760622897878241));
#62012=CARTESIAN_POINT('',(3.74449296983004,1.,0.2031560948961));
#62013=CARTESIAN_POINT('Ctrl Pts',(3.74449296983004,-1.,0.2031560948961));
#62014=CARTESIAN_POINT('Ctrl Pts',(3.74449296983004,-0.666666666666667,
0.2031560948961));
#62015=CARTESIAN_POINT('Ctrl Pts',(3.74449296983004,-0.333333333333333,
0.2031560948961));
#62016=CARTESIAN_POINT('Ctrl Pts',(3.74449296983004,0.333333333333333,0.2031560948961));
#62017=CARTESIAN_POINT('Ctrl Pts',(3.74449296983004,0.666666666666667,0.2031560948961));
#62018=CARTESIAN_POINT('Ctrl Pts',(3.74449296983004,1.,0.2031560948961));
#62019=CARTESIAN_POINT('',(4.19931119685982,1.,0.0760622897878241));
#62020=CARTESIAN_POINT('',(4.19931119685982,0.,0.0760622897878241));
#62021=CARTESIAN_POINT('Ctrl Pts',(3.74449296983004,1.,0.2031560948961));
#62022=CARTESIAN_POINT('Ctrl Pts',(3.74453008995092,1.,0.203188003946656));
#62023=CARTESIAN_POINT('Ctrl Pts',(3.74471097893845,1.,0.20326661011053));
#62024=CARTESIAN_POINT('Ctrl Pts',(3.74535749969115,1.,0.203375226874121));
#62025=CARTESIAN_POINT('Ctrl Pts',(3.74703926501752,1.,0.203484186269415));
#62026=CARTESIAN_POINT('Ctrl Pts',(3.75054693397875,1.,0.203550035479166));
#62027=CARTESIAN_POINT('Ctrl Pts',(3.75585118707734,1.,0.203530796848321));
#62028=CARTESIAN_POINT('Ctrl Pts',(3.76242717936885,1.,0.203414634707478));
#62029=CARTESIAN_POINT('Ctrl Pts',(3.7699207159487,1.,0.203192390045164));
#62030=CARTESIAN_POINT('Ctrl Pts',(3.77793553476614,1.,0.20285472969908));
#62031=CARTESIAN_POINT('Ctrl Pts',(3.78609175019242,1.,0.20239426051216));
#62032=CARTESIAN_POINT('Ctrl Pts',(3.7940835418736,1.,0.201807533800837));
#62033=CARTESIAN_POINT('Ctrl Pts',(3.80175247447337,1.,0.201097756307325));
#62034=CARTESIAN_POINT('Ctrl Pts',(3.80909529318669,1.,0.200274679433364));
#62035=CARTESIAN_POINT('Ctrl Pts',(3.81620203429815,1.,0.199351525297447));
#62036=CARTESIAN_POINT('Ctrl Pts',(3.82321127349016,1.,0.198342616900486));
#62037=CARTESIAN_POINT('Ctrl Pts',(3.83026221776456,1.,0.197260935827361));
#62038=CARTESIAN_POINT('Ctrl Pts',(3.83743910616195,1.,0.196115198971858));
#62039=CARTESIAN_POINT('Ctrl Pts',(3.84475203346977,1.,0.19490900946022));
#62040=CARTESIAN_POINT('Ctrl Pts',(3.85216762263966,1.,0.193642806777722));
#62041=CARTESIAN_POINT('Ctrl Pts',(3.85962774407633,1.,0.19231515304497));
#62042=CARTESIAN_POINT('Ctrl Pts',(3.86707158624783,1.,0.190924190418619));
#62043=CARTESIAN_POINT('Ctrl Pts',(3.87445976418412,1.,0.189469253358272));
#62044=CARTESIAN_POINT('Ctrl Pts',(3.88178563496228,1.,0.187951632512684));
#62045=CARTESIAN_POINT('Ctrl Pts',(3.88906196725848,1.,0.18637372498528));
#62046=CARTESIAN_POINT('Ctrl Pts',(3.89631300742646,1.,0.184738537728042));
#62047=CARTESIAN_POINT('Ctrl Pts',(3.90356488555132,1.,0.18304908199319));
#62048=CARTESIAN_POINT('Ctrl Pts',(3.91083557557175,1.,0.181307740731785));
#62049=CARTESIAN_POINT('Ctrl Pts',(3.91812876180926,1.,0.179515885822881));
#62050=CARTESIAN_POINT('Ctrl Pts',(3.92543942697655,1.,0.177674246152317));
#62051=CARTESIAN_POINT('Ctrl Pts',(3.93275726771042,1.,0.175783136893867));
#62052=CARTESIAN_POINT('Ctrl Pts',(3.94007083096217,1.,0.173842734974609));
#62053=CARTESIAN_POINT('Ctrl Pts',(3.94737164900868,1.,0.17185335536924));
#62054=CARTESIAN_POINT('Ctrl Pts',(3.95465744665268,1.,0.169815666374138));
#62055=CARTESIAN_POINT('Ctrl Pts',(3.96192990160296,1.,0.167730547023319));
#62056=CARTESIAN_POINT('Ctrl Pts',(3.96919313621407,1.,0.165598992851102));
#62057=CARTESIAN_POINT('Ctrl Pts',(3.97645194630943,1.,0.163422004609999));
#62058=CARTESIAN_POINT('Ctrl Pts',(3.98371010319872,1.,0.161200482186084));
#62059=CARTESIAN_POINT('Ctrl Pts',(3.99096873945878,1.,0.158935123982793));
#62060=CARTESIAN_POINT('Ctrl Pts',(3.99822717425893,1.,0.156626481393734));
#62061=CARTESIAN_POINT('Ctrl Pts',(4.00548360245319,1.,0.15427500487231));
#62062=CARTESIAN_POINT('Ctrl Pts',(4.01273584234689,1.,0.15188109402291));
#62063=CARTESIAN_POINT('Ctrl Pts',(4.01998203715564,1.,0.149445144968706));
#62064=CARTESIAN_POINT('Ctrl Pts',(4.02722143146994,1.,0.146967602878994));
#62065=CARTESIAN_POINT('Ctrl Pts',(4.03445411510333,1.,0.144448947038344));
#62066=CARTESIAN_POINT('Ctrl Pts',(4.04168069633781,1.,0.1418896714855));
#62067=CARTESIAN_POINT('Ctrl Pts',(4.04890199238036,1.,0.139290267180057));
#62068=CARTESIAN_POINT('Ctrl Pts',(4.05611873400172,1.,0.136651205046119));
#62069=CARTESIAN_POINT('Ctrl Pts',(4.06333121018596,1.,0.133972916144244));
#62070=CARTESIAN_POINT('Ctrl Pts',(4.0705393152874,1.,0.13125579354894));
#62071=CARTESIAN_POINT('Ctrl Pts',(4.07774270738954,1.,0.128500200484837));
#62072=CARTESIAN_POINT('Ctrl Pts',(4.08494093372377,1.,0.125706476822539));
#62073=CARTESIAN_POINT('Ctrl Pts',(4.09213355850756,1.,0.122874946249106));
#62074=CARTESIAN_POINT('Ctrl Pts',(4.09932031767002,1.,0.120005924388124));
#62075=CARTESIAN_POINT('Ctrl Pts',(4.10650113381833,1.,0.117099722731648));
#62076=CARTESIAN_POINT('Ctrl Pts',(4.11367603924961,1.,0.114156649609545));
#62077=CARTESIAN_POINT('Ctrl Pts',(4.1208451250225,1.,0.111177012683346));
#62078=CARTESIAN_POINT('Ctrl Pts',(4.12800848371504,1.,0.108161120528369));
#62079=CARTESIAN_POINT('Ctrl Pts',(4.13516614458895,1.,0.105109286538945));
#62080=CARTESIAN_POINT('Ctrl Pts',(4.14231804939538,1.,0.102021826577583));
#62081=CARTESIAN_POINT('Ctrl Pts',(4.14946408918485,1.,0.0988990478901221));
#62082=CARTESIAN_POINT('Ctrl Pts',(4.15660412653577,1.,0.0957412403298002));
#62083=CARTESIAN_POINT('Ctrl Pts',(4.16373802265839,1.,0.0925486672167526));
#62084=CARTESIAN_POINT('Ctrl Pts',(4.17086566490794,1.,0.0893215560848644));
#62085=CARTESIAN_POINT('Ctrl Pts',(4.17798698668094,1.,0.0860600915549391));
#62086=CARTESIAN_POINT('Ctrl Pts',(4.18510195327123,1.,0.0827644164385674));
#62087=CARTESIAN_POINT('Ctrl Pts',(4.19078883320504,1.,0.0801005887114315));
#62088=CARTESIAN_POINT('Ctrl Pts',(4.19505112859416,1.,0.0780873956242392));
#62089=CARTESIAN_POINT('Ctrl Pts',(4.1978913862118,1.,0.0767384596141459));
#62090=CARTESIAN_POINT('Ctrl Pts',(4.19931119685982,1.,0.0760622897878241));
#62091=CARTESIAN_POINT('Ctrl Pts',(4.19931119685982,-1.,-0.0760622897878241));
#62092=CARTESIAN_POINT('Ctrl Pts',(4.19931119685982,1.,-0.0760622897878241));
#62093=CARTESIAN_POINT('Ctrl Pts',(4.19789138621624,-1.,-0.07673845961422));
#62094=CARTESIAN_POINT('Ctrl Pts',(4.19789138621624,1.,-0.07673845961422));
#62095=CARTESIAN_POINT('Ctrl Pts',(4.19505112860624,-1.,-0.0780873956244407));
#62096=CARTESIAN_POINT('Ctrl Pts',(4.19505112860624,1.,-0.0780873956244407));
#62097=CARTESIAN_POINT('Ctrl Pts',(4.19078883322483,-1.,-0.0801005887117608));
#62098=CARTESIAN_POINT('Ctrl Pts',(4.19078883322483,1.,-0.0801005887117608));
#62099=CARTESIAN_POINT('Ctrl Pts',(4.1851019532944,-1.,-0.0827644164389515));
#62100=CARTESIAN_POINT('Ctrl Pts',(4.1851019532944,1.,-0.0827644164389515));
#62101=CARTESIAN_POINT('Ctrl Pts',(4.17798698669991,-1.,-0.086060091555252));
#62102=CARTESIAN_POINT('Ctrl Pts',(4.17798698669991,1.,-0.086060091555252));
#62103=CARTESIAN_POINT('Ctrl Pts',(4.17086566491823,-1.,-0.0893215560850332));
#62104=CARTESIAN_POINT('Ctrl Pts',(4.17086566491823,1.,-0.0893215560850332));
#62105=CARTESIAN_POINT('Ctrl Pts',(4.16373802265942,-1.,-0.0925486672167695));
#62106=CARTESIAN_POINT('Ctrl Pts',(4.16373802265942,1.,-0.0925486672167695));
#62107=CARTESIAN_POINT('Ctrl Pts',(4.15660412653006,-1.,-0.0957412403297072));
#62108=CARTESIAN_POINT('Ctrl Pts',(4.15660412653006,1.,-0.0957412403297072));
#62109=CARTESIAN_POINT('Ctrl Pts',(4.1494640891762,-1.,-0.0988990478899816));
#62110=CARTESIAN_POINT('Ctrl Pts',(4.1494640891762,1.,-0.0988990478899816));
#62111=CARTESIAN_POINT('Ctrl Pts',(4.14231804938737,-1.,-0.102021826577454));
#62112=CARTESIAN_POINT('Ctrl Pts',(4.14231804938737,1.,-0.102021826577454));
#62113=CARTESIAN_POINT('Ctrl Pts',(4.13516614458396,-1.,-0.105109286538864));
#62114=CARTESIAN_POINT('Ctrl Pts',(4.13516614458396,1.,-0.105109286538864));
#62115=CARTESIAN_POINT('Ctrl Pts',(4.12800848371386,-1.,-0.10816112052835));
#62116=CARTESIAN_POINT('Ctrl Pts',(4.12800848371386,1.,-0.10816112052835));
#62117=CARTESIAN_POINT('Ctrl Pts',(4.12084512502444,-1.,-0.111177012683378));
#62118=CARTESIAN_POINT('Ctrl Pts',(4.12084512502444,1.,-0.111177012683378));
#62119=CARTESIAN_POINT('Ctrl Pts',(4.11367603925313,-1.,-0.114156649609602));
#62120=CARTESIAN_POINT('Ctrl Pts',(4.11367603925313,1.,-0.114156649609602));
#62121=CARTESIAN_POINT('Ctrl Pts',(4.10650113382187,-1.,-0.117099722731705));
#62122=CARTESIAN_POINT('Ctrl Pts',(4.10650113382187,1.,-0.117099722731705));
#62123=CARTESIAN_POINT('Ctrl Pts',(4.09932031767243,-1.,-0.120005924388162));
#62124=CARTESIAN_POINT('Ctrl Pts',(4.09932031767243,1.,-0.120005924388162));
#62125=CARTESIAN_POINT('Ctrl Pts',(4.09213355850836,-1.,-0.122874946249119));
#62126=CARTESIAN_POINT('Ctrl Pts',(4.09213355850836,1.,-0.122874946249119));
#62127=CARTESIAN_POINT('Ctrl Pts',(4.08494093372315,-1.,-0.12570647682253));
#62128=CARTESIAN_POINT('Ctrl Pts',(4.08494093372315,1.,-0.12570647682253));
#62129=CARTESIAN_POINT('Ctrl Pts',(4.07774270738809,-1.,-0.128500200484814));
#62130=CARTESIAN_POINT('Ctrl Pts',(4.07774270738809,1.,-0.128500200484814));
#62131=CARTESIAN_POINT('Ctrl Pts',(4.07053931528579,-1.,-0.131255793548914));
#62132=CARTESIAN_POINT('Ctrl Pts',(4.07053931528579,1.,-0.131255793548914));
#62133=CARTESIAN_POINT('Ctrl Pts',(4.06333121018476,-1.,-0.133972916144225));
#62134=CARTESIAN_POINT('Ctrl Pts',(4.06333121018476,1.,-0.133972916144225));
#62135=CARTESIAN_POINT('Ctrl Pts',(4.05611873400122,-1.,-0.136651205046111));
#62136=CARTESIAN_POINT('Ctrl Pts',(4.05611873400122,1.,-0.136651205046111));
#62137=CARTESIAN_POINT('Ctrl Pts',(4.04890199238056,-1.,-0.13929026718006));
#62138=CARTESIAN_POINT('Ctrl Pts',(4.04890199238056,1.,-0.13929026718006));
#62139=CARTESIAN_POINT('Ctrl Pts',(4.04168069633842,-1.,-0.141889671485508));
#62140=CARTESIAN_POINT('Ctrl Pts',(4.04168069633842,1.,-0.141889671485508));
#62141=CARTESIAN_POINT('Ctrl Pts',(4.03445411510403,-1.,-0.144448947038352));
#62142=CARTESIAN_POINT('Ctrl Pts',(4.03445411510403,1.,-0.144448947038352));
#62143=CARTESIAN_POINT('Ctrl Pts',(4.02722143147048,-1.,-0.146967602878999));
#62144=CARTESIAN_POINT('Ctrl Pts',(4.02722143147048,1.,-0.146967602878999));
#62145=CARTESIAN_POINT('Ctrl Pts',(4.01998203715588,-1.,-0.149445144968708));
#62146=CARTESIAN_POINT('Ctrl Pts',(4.01998203715588,1.,-0.149445144968708));
#62147=CARTESIAN_POINT('Ctrl Pts',(4.01273584234684,-1.,-0.151881094022909));
#62148=CARTESIAN_POINT('Ctrl Pts',(4.01273584234684,1.,-0.151881094022909));
#62149=CARTESIAN_POINT('Ctrl Pts',(4.00548360245297,-1.,-0.15427500487231));
#62150=CARTESIAN_POINT('Ctrl Pts',(4.00548360245297,1.,-0.15427500487231));
#62151=CARTESIAN_POINT('Ctrl Pts',(3.99822717425869,-1.,-0.156626481393736));
#62152=CARTESIAN_POINT('Ctrl Pts',(3.99822717425869,1.,-0.156626481393736));
#62153=CARTESIAN_POINT('Ctrl Pts',(3.99096873945862,-1.,-0.158935123982796));
#62154=CARTESIAN_POINT('Ctrl Pts',(3.99096873945862,1.,-0.158935123982796));
#62155=CARTESIAN_POINT('Ctrl Pts',(3.98371010319866,-1.,-0.161200482186088));
#62156=CARTESIAN_POINT('Ctrl Pts',(3.98371010319866,1.,-0.161200482186088));
#62157=CARTESIAN_POINT('Ctrl Pts',(3.97645194630944,-1.,-0.163422004609999));
#62158=CARTESIAN_POINT('Ctrl Pts',(3.97645194630944,1.,-0.163422004609999));
#62159=CARTESIAN_POINT('Ctrl Pts',(3.9691931362141,-1.,-0.165598992851098));
#62160=CARTESIAN_POINT('Ctrl Pts',(3.9691931362141,1.,-0.165598992851098));
#62161=CARTESIAN_POINT('Ctrl Pts',(3.96192990160296,-1.,-0.167730547023312));
#62162=CARTESIAN_POINT('Ctrl Pts',(3.96192990160296,1.,-0.167730547023312));
#62163=CARTESIAN_POINT('Ctrl Pts',(3.95465744665263,-1.,-0.16981566637413));
#62164=CARTESIAN_POINT('Ctrl Pts',(3.95465744665263,1.,-0.16981566637413));
#62165=CARTESIAN_POINT('Ctrl Pts',(3.94737164900861,-1.,-0.171853355369233));
#62166=CARTESIAN_POINT('Ctrl Pts',(3.94737164900861,1.,-0.171853355369233));
#62167=CARTESIAN_POINT('Ctrl Pts',(3.94007083096214,-1.,-0.173842734974608));
#62168=CARTESIAN_POINT('Ctrl Pts',(3.94007083096214,1.,-0.173842734974608));
#62169=CARTESIAN_POINT('Ctrl Pts',(3.93275726771049,-1.,-0.175783136893873));
#62170=CARTESIAN_POINT('Ctrl Pts',(3.93275726771049,1.,-0.175783136893873));
#62171=CARTESIAN_POINT('Ctrl Pts',(3.92543942697672,-1.,-0.177674246152328));
#62172=CARTESIAN_POINT('Ctrl Pts',(3.92543942697672,1.,-0.177674246152328));
#62173=CARTESIAN_POINT('Ctrl Pts',(3.91812876180948,-1.,-0.179515885822895));
#62174=CARTESIAN_POINT('Ctrl Pts',(3.91812876180948,1.,-0.179515885822895));
#62175=CARTESIAN_POINT('Ctrl Pts',(3.91083557557193,-1.,-0.181307740731796));
#62176=CARTESIAN_POINT('Ctrl Pts',(3.91083557557193,1.,-0.181307740731796));
#62177=CARTESIAN_POINT('Ctrl Pts',(3.90356488555138,-1.,-0.183049081993193));
#62178=CARTESIAN_POINT('Ctrl Pts',(3.90356488555138,1.,-0.183049081993193));
#62179=CARTESIAN_POINT('Ctrl Pts',(3.89631300742633,-1.,-0.184738537728035));
#62180=CARTESIAN_POINT('Ctrl Pts',(3.89631300742633,1.,-0.184738537728035));
#62181=CARTESIAN_POINT('Ctrl Pts',(3.88906196725817,-1.,-0.186373724985263));
#62182=CARTESIAN_POINT('Ctrl Pts',(3.88906196725817,1.,-0.186373724985263));
#62183=CARTESIAN_POINT('Ctrl Pts',(3.88178563496187,-1.,-0.187951632512664));
#62184=CARTESIAN_POINT('Ctrl Pts',(3.88178563496187,1.,-0.187951632512664));
#62185=CARTESIAN_POINT('Ctrl Pts',(3.87445976418377,-1.,-0.189469253358255));
#62186=CARTESIAN_POINT('Ctrl Pts',(3.87445976418377,1.,-0.189469253358255));
#62187=CARTESIAN_POINT('Ctrl Pts',(3.8670715862477,-1.,-0.190924190418613));
#62188=CARTESIAN_POINT('Ctrl Pts',(3.8670715862477,1.,-0.190924190418613));
#62189=CARTESIAN_POINT('Ctrl Pts',(3.85962774407652,-1.,-0.19231515304498));
#62190=CARTESIAN_POINT('Ctrl Pts',(3.85962774407652,1.,-0.19231515304498));
#62191=CARTESIAN_POINT('Ctrl Pts',(3.85216762264019,-1.,-0.193642806777748));
#62192=CARTESIAN_POINT('Ctrl Pts',(3.85216762264019,1.,-0.193642806777748));
#62193=CARTESIAN_POINT('Ctrl Pts',(3.84475203347052,-1.,-0.194909009460255));
#62194=CARTESIAN_POINT('Ctrl Pts',(3.84475203347052,1.,-0.194909009460255));
#62195=CARTESIAN_POINT('Ctrl Pts',(3.83743910616265,-1.,-0.19611519897189));
#62196=CARTESIAN_POINT('Ctrl Pts',(3.83743910616265,1.,-0.19611519897189));
#62197=CARTESIAN_POINT('Ctrl Pts',(3.83026221776488,-1.,-0.197260935827375));
#62198=CARTESIAN_POINT('Ctrl Pts',(3.83026221776488,1.,-0.197260935827375));
#62199=CARTESIAN_POINT('Ctrl Pts',(3.82321127348981,-1.,-0.19834261690047));
#62200=CARTESIAN_POINT('Ctrl Pts',(3.82321127348981,1.,-0.19834261690047));
#62201=CARTESIAN_POINT('Ctrl Pts',(3.81620203429702,-1.,-0.199351525297397));
#62202=CARTESIAN_POINT('Ctrl Pts',(3.81620203429702,1.,-0.199351525297397));
#62203=CARTESIAN_POINT('Ctrl Pts',(3.80909529318501,-1.,-0.20027467943329));
#62204=CARTESIAN_POINT('Ctrl Pts',(3.80909529318501,1.,-0.20027467943329));
#62205=CARTESIAN_POINT('Ctrl Pts',(3.80175247447171,-1.,-0.201097756307252));
#62206=CARTESIAN_POINT('Ctrl Pts',(3.80175247447171,1.,-0.201097756307252));
#62207=CARTESIAN_POINT('Ctrl Pts',(3.79408354187274,-1.,-0.201807533800799));
#62208=CARTESIAN_POINT('Ctrl Pts',(3.79408354187274,1.,-0.201807533800799));
#62209=CARTESIAN_POINT('Ctrl Pts',(3.78609175019317,-1.,-0.202394260512193));
#62210=CARTESIAN_POINT('Ctrl Pts',(3.78609175019317,1.,-0.202394260512193));
#62211=CARTESIAN_POINT('Ctrl Pts',(3.77793553476879,-1.,-0.202854729699197));
#62212=CARTESIAN_POINT('Ctrl Pts',(3.77793553476879,1.,-0.202854729699197));
#62213=CARTESIAN_POINT('Ctrl Pts',(3.76992071595267,-1.,-0.203192390045338));
#62214=CARTESIAN_POINT('Ctrl Pts',(3.76992071595267,1.,-0.203192390045338));
#62215=CARTESIAN_POINT('Ctrl Pts',(3.76242717937273,-1.,-0.203414634707647));
#62216=CARTESIAN_POINT('Ctrl Pts',(3.76242717937273,1.,-0.203414634707647));
#62217=CARTESIAN_POINT('Ctrl Pts',(3.75585118707924,-1.,-0.203530796848404));
#62218=CARTESIAN_POINT('Ctrl Pts',(3.75585118707924,1.,-0.203530796848404));
#62219=CARTESIAN_POINT('Ctrl Pts',(3.75054693397716,-1.,-0.203550035479097));
#62220=CARTESIAN_POINT('Ctrl Pts',(3.75054693397716,1.,-0.203550035479097));
#62221=CARTESIAN_POINT('Ctrl Pts',(3.74675472018582,-1.,-0.20347884453023));
#62222=CARTESIAN_POINT('Ctrl Pts',(3.74675472018582,1.,-0.20347884453023));
#62223=CARTESIAN_POINT('Ctrl Pts',(3.7450208092684,-1.,-0.203352057956056));
#62224=CARTESIAN_POINT('Ctrl Pts',(3.7450208092684,1.,-0.203352057956056));
#62225=CARTESIAN_POINT('Ctrl Pts',(3.74446880195845,-1.,-0.203218215747895));
#62226=CARTESIAN_POINT('Ctrl Pts',(3.74446880195845,1.,-0.203218215747895));
#62227=CARTESIAN_POINT('Ctrl Pts',(3.74443319346666,-1.,-0.20311176758786));
#62228=CARTESIAN_POINT('Ctrl Pts',(3.74443319346666,1.,-0.20311176758786));
#62229=CARTESIAN_POINT('Ctrl Pts',(3.74449849461127,-1.,-0.20305423869972));
#62230=CARTESIAN_POINT('Ctrl Pts',(3.74449849461127,1.,-0.20305423869972));
#62231=CARTESIAN_POINT('',(4.19931119685982,1.,-0.0760622897878241));
#62232=CARTESIAN_POINT('Ctrl Pts',(4.19931119685982,1.,-0.0760622897878241));
#62233=CARTESIAN_POINT('Ctrl Pts',(4.19789138621624,1.,-0.07673845961422));
#62234=CARTESIAN_POINT('Ctrl Pts',(4.19505112860624,1.,-0.0780873956244407));
#62235=CARTESIAN_POINT('Ctrl Pts',(4.19078883322483,1.,-0.0801005887117608));
#62236=CARTESIAN_POINT('Ctrl Pts',(4.1851019532944,1.,-0.0827644164389515));
#62237=CARTESIAN_POINT('Ctrl Pts',(4.17798698669991,1.,-0.086060091555252));
#62238=CARTESIAN_POINT('Ctrl Pts',(4.17086566491823,1.,-0.0893215560850332));
#62239=CARTESIAN_POINT('Ctrl Pts',(4.16373802265942,1.,-0.0925486672167695));
#62240=CARTESIAN_POINT('Ctrl Pts',(4.15660412653006,1.,-0.0957412403297072));
#62241=CARTESIAN_POINT('Ctrl Pts',(4.1494640891762,1.,-0.0988990478899816));
#62242=CARTESIAN_POINT('Ctrl Pts',(4.14231804938737,1.,-0.102021826577454));
#62243=CARTESIAN_POINT('Ctrl Pts',(4.13516614458396,1.,-0.105109286538864));
#62244=CARTESIAN_POINT('Ctrl Pts',(4.12800848371386,1.,-0.10816112052835));
#62245=CARTESIAN_POINT('Ctrl Pts',(4.12084512502444,1.,-0.111177012683378));
#62246=CARTESIAN_POINT('Ctrl Pts',(4.11367603925313,1.,-0.114156649609602));
#62247=CARTESIAN_POINT('Ctrl Pts',(4.10650113382187,1.,-0.117099722731705));
#62248=CARTESIAN_POINT('Ctrl Pts',(4.09932031767243,1.,-0.120005924388162));
#62249=CARTESIAN_POINT('Ctrl Pts',(4.09213355850836,1.,-0.122874946249119));
#62250=CARTESIAN_POINT('Ctrl Pts',(4.08494093372315,1.,-0.12570647682253));
#62251=CARTESIAN_POINT('Ctrl Pts',(4.07774270738809,1.,-0.128500200484814));
#62252=CARTESIAN_POINT('Ctrl Pts',(4.07053931528579,1.,-0.131255793548914));
#62253=CARTESIAN_POINT('Ctrl Pts',(4.06333121018476,1.,-0.133972916144225));
#62254=CARTESIAN_POINT('Ctrl Pts',(4.05611873400122,1.,-0.136651205046111));
#62255=CARTESIAN_POINT('Ctrl Pts',(4.04890199238056,1.,-0.13929026718006));
#62256=CARTESIAN_POINT('Ctrl Pts',(4.04168069633842,1.,-0.141889671485508));
#62257=CARTESIAN_POINT('Ctrl Pts',(4.03445411510403,1.,-0.144448947038352));
#62258=CARTESIAN_POINT('Ctrl Pts',(4.02722143147048,1.,-0.146967602878999));
#62259=CARTESIAN_POINT('Ctrl Pts',(4.01998203715588,1.,-0.149445144968708));
#62260=CARTESIAN_POINT('Ctrl Pts',(4.01273584234684,1.,-0.151881094022909));
#62261=CARTESIAN_POINT('Ctrl Pts',(4.00548360245297,1.,-0.15427500487231));
#62262=CARTESIAN_POINT('Ctrl Pts',(3.99822717425869,1.,-0.156626481393736));
#62263=CARTESIAN_POINT('Ctrl Pts',(3.99096873945862,1.,-0.158935123982796));
#62264=CARTESIAN_POINT('Ctrl Pts',(3.98371010319866,1.,-0.161200482186088));
#62265=CARTESIAN_POINT('Ctrl Pts',(3.97645194630944,1.,-0.163422004609999));
#62266=CARTESIAN_POINT('Ctrl Pts',(3.9691931362141,1.,-0.165598992851098));
#62267=CARTESIAN_POINT('Ctrl Pts',(3.96192990160296,1.,-0.167730547023312));
#62268=CARTESIAN_POINT('Ctrl Pts',(3.95465744665263,1.,-0.16981566637413));
#62269=CARTESIAN_POINT('Ctrl Pts',(3.94737164900861,1.,-0.171853355369233));
#62270=CARTESIAN_POINT('Ctrl Pts',(3.94007083096214,1.,-0.173842734974608));
#62271=CARTESIAN_POINT('Ctrl Pts',(3.93275726771049,1.,-0.175783136893873));
#62272=CARTESIAN_POINT('Ctrl Pts',(3.92543942697672,1.,-0.177674246152328));
#62273=CARTESIAN_POINT('Ctrl Pts',(3.91812876180948,1.,-0.179515885822895));
#62274=CARTESIAN_POINT('Ctrl Pts',(3.91083557557193,1.,-0.181307740731796));
#62275=CARTESIAN_POINT('Ctrl Pts',(3.90356488555138,1.,-0.183049081993193));
#62276=CARTESIAN_POINT('Ctrl Pts',(3.89631300742633,1.,-0.184738537728035));
#62277=CARTESIAN_POINT('Ctrl Pts',(3.88906196725817,1.,-0.186373724985263));
#62278=CARTESIAN_POINT('Ctrl Pts',(3.88178563496187,1.,-0.187951632512664));
#62279=CARTESIAN_POINT('Ctrl Pts',(3.87445976418377,1.,-0.189469253358255));
#62280=CARTESIAN_POINT('Ctrl Pts',(3.8670715862477,1.,-0.190924190418613));
#62281=CARTESIAN_POINT('Ctrl Pts',(3.85962774407652,1.,-0.19231515304498));
#62282=CARTESIAN_POINT('Ctrl Pts',(3.85216762264019,1.,-0.193642806777748));
#62283=CARTESIAN_POINT('Ctrl Pts',(3.84475203347052,1.,-0.194909009460255));
#62284=CARTESIAN_POINT('Ctrl Pts',(3.83743910616265,1.,-0.19611519897189));
#62285=CARTESIAN_POINT('Ctrl Pts',(3.83026221776488,1.,-0.197260935827375));
#62286=CARTESIAN_POINT('Ctrl Pts',(3.82321127348981,1.,-0.19834261690047));
#62287=CARTESIAN_POINT('Ctrl Pts',(3.81620203429702,1.,-0.199351525297397));
#62288=CARTESIAN_POINT('Ctrl Pts',(3.80909529318501,1.,-0.20027467943329));
#62289=CARTESIAN_POINT('Ctrl Pts',(3.80175247447171,1.,-0.201097756307252));
#62290=CARTESIAN_POINT('Ctrl Pts',(3.79408354187274,1.,-0.201807533800799));
#62291=CARTESIAN_POINT('Ctrl Pts',(3.78609175019317,1.,-0.202394260512193));
#62292=CARTESIAN_POINT('Ctrl Pts',(3.77793553476879,1.,-0.202854729699197));
#62293=CARTESIAN_POINT('Ctrl Pts',(3.76992071595267,1.,-0.203192390045338));
#62294=CARTESIAN_POINT('Ctrl Pts',(3.76242717937273,1.,-0.203414634707647));
#62295=CARTESIAN_POINT('Ctrl Pts',(3.75585118707924,1.,-0.203530796848404));
#62296=CARTESIAN_POINT('Ctrl Pts',(3.75054693397716,1.,-0.203550035479097));
#62297=CARTESIAN_POINT('Ctrl Pts',(3.74703926501843,1.,-0.203484186269315));
#62298=CARTESIAN_POINT('Ctrl Pts',(3.74535749969262,1.,-0.203375226874332));
#62299=CARTESIAN_POINT('Ctrl Pts',(3.74471097893961,1.,-0.203266610111264));
#62300=CARTESIAN_POINT('Ctrl Pts',(3.74453008995129,1.,-0.203188003947965));
#62301=CARTESIAN_POINT('Ctrl Pts',(3.74449296982994,1.,-0.203156094897896));
#62302=CARTESIAN_POINT('',(4.19931119685982,0.,-0.0760622897878241));
#62303=CARTESIAN_POINT('Origin',(4.19931119685982,0.,0.0760622897878241));
#62304=CARTESIAN_POINT('',(4.19931119685982,1.,-0.0760622897878241));
#62305=CARTESIAN_POINT('Origin',(0.,1.,0.));
#62306=CARTESIAN_POINT('Origin',(0.,1.,0.));
#62307=CARTESIAN_POINT('Origin',(0.,0.,0.));
#62308=CARTESIAN_POINT('',(0.,0.,0.));
#62309=CARTESIAN_POINT('Origin',(-1.,0.,0.35));
#62310=CARTESIAN_POINT('',(-1.,-0.26,0.6));
#62311=CARTESIAN_POINT('',(-1.,-0.3,0.56));
#62312=CARTESIAN_POINT('',(-1.,-0.2675,0.5925));
#62313=CARTESIAN_POINT('',(-1.,0.26,0.6));
#62314=CARTESIAN_POINT('',(-1.,0.,0.6));
#62315=CARTESIAN_POINT('',(-1.,0.3,0.56));
#62316=CARTESIAN_POINT('',(-1.,0.2675,0.5925));
#62317=CARTESIAN_POINT('',(-1.,0.3,0.04));
#62318=CARTESIAN_POINT('',(-1.,0.3,0.175));
#62319=CARTESIAN_POINT('',(-1.,0.26,0.));
#62320=CARTESIAN_POINT('',(-1.,0.2925,0.0325));
#62321=CARTESIAN_POINT('',(-1.,-0.26,0.));
#62322=CARTESIAN_POINT('',(-1.,0.,0.));
#62323=CARTESIAN_POINT('',(-1.,-0.3,0.04));
#62324=CARTESIAN_POINT('',(-1.,-0.2925,0.0325));
#62325=CARTESIAN_POINT('',(-1.,-0.3,0.175));
#62326=CARTESIAN_POINT('Origin',(0.75,0.28,0.02));
#62327=CARTESIAN_POINT('',(1.,0.3,0.04));
#62328=CARTESIAN_POINT('',(0.75,0.3,0.04));
#62329=CARTESIAN_POINT('',(1.,0.26,0.));
#62330=CARTESIAN_POINT('',(1.,0.2925,0.0325));
#62331=CARTESIAN_POINT('',(0.75,0.26,0.));
#62332=CARTESIAN_POINT('Origin',(1.5,0.3,0.));
#62333=CARTESIAN_POINT('',(1.,0.3,0.56));
#62334=CARTESIAN_POINT('',(0.75,0.3,0.56));
#62335=CARTESIAN_POINT('',(1.,0.3,0.175));
#62336=CARTESIAN_POINT('Origin',(0.75,0.28,0.58));
#62337=CARTESIAN_POINT('',(1.,0.26,0.6));
#62338=CARTESIAN_POINT('',(0.75,0.26,0.6));
#62339=CARTESIAN_POINT('',(1.,0.2675,0.5925));
#62340=CARTESIAN_POINT('Origin',(0.,0.,0.6));
#62341=CARTESIAN_POINT('',(1.,-0.26,0.6));
#62342=CARTESIAN_POINT('',(-0.75,-0.26,0.6));
#62343=CARTESIAN_POINT('',(1.,0.,0.6));
#62344=CARTESIAN_POINT('Origin',(1.,0.,0.35));
#62345=CARTESIAN_POINT('',(1.,-0.26,0.));
#62346=CARTESIAN_POINT('',(1.,-0.3,0.04));
#62347=CARTESIAN_POINT('',(1.,-0.2925,0.0325));
#62348=CARTESIAN_POINT('',(1.,0.,0.));
#62349=CARTESIAN_POINT('',(1.,-0.3,0.56));
#62350=CARTESIAN_POINT('',(1.,-0.2675,0.5925));
#62351=CARTESIAN_POINT('',(1.,-0.3,0.175));
#62352=CARTESIAN_POINT('Origin',(0.,0.,0.));
#62353=CARTESIAN_POINT('',(-0.75,-0.26,0.));
#62354=CARTESIAN_POINT('Origin',(-0.75,-0.28,0.58));
#62355=CARTESIAN_POINT('',(-0.75,-0.3,0.56));
#62356=CARTESIAN_POINT('Origin',(-0.75,-0.28,0.02));
#62357=CARTESIAN_POINT('',(-0.75,-0.3,0.04));
#62358=CARTESIAN_POINT('Origin',(-1.5,-0.3,0.));
#62359=CARTESIAN_POINT('',(0.,0.,0.));
#62360=CARTESIAN_POINT('Origin',(0.0721687836487032,0.,-0.125));
#62361=CARTESIAN_POINT('',(0.0721687836487032,0.,-0.125));
#62362=CARTESIAN_POINT('',(0.144337567297406,0.,0.));
#62363=CARTESIAN_POINT('',(0.117710979560879,0.,-0.0461186027918559));
#62364=CARTESIAN_POINT('',(0.0721687836487032,-0.25,-0.125));
#62365=CARTESIAN_POINT('',(0.0721687836487032,0.,-0.125));
#62366=CARTESIAN_POINT('',(0.144337567297406,-0.25,0.));
#62367=CARTESIAN_POINT('',(0.144337567297406,-0.25,0.));
#62368=CARTESIAN_POINT('',(0.144337567297406,0.,0.));
#62369=CARTESIAN_POINT('Origin',(-0.0721687836487032,0.,-0.125));
#62370=CARTESIAN_POINT('',(-0.0721687836487032,0.,-0.125));
#62371=CARTESIAN_POINT('',(0.0739156081756484,0.,-0.125));
#62372=CARTESIAN_POINT('',(-0.0721687836487032,-0.25,-0.125));
#62373=CARTESIAN_POINT('',(-0.0721687836487032,0.,-0.125));
#62374=CARTESIAN_POINT('',(0.0721687836487032,-0.25,-0.125));
#62375=CARTESIAN_POINT('Origin',(-0.144337567297406,0.,-4.16333634234434E-17));
#62376=CARTESIAN_POINT('',(-0.144337567297406,0.,-1.76762539787485E-17));
#62377=CARTESIAN_POINT('',(-0.0987953713852306,0.,-0.0788813972081442));
#62378=CARTESIAN_POINT('',(-0.144337567297406,-0.25,-2.77555756156289E-17));
#62379=CARTESIAN_POINT('',(-0.144337567297406,0.,-1.76762539787485E-17));
#62380=CARTESIAN_POINT('',(-0.0721687836487032,-0.25,-0.125));
#62381=CARTESIAN_POINT('Origin',(-0.0721687836487033,0.,0.125));
#62382=CARTESIAN_POINT('',(-0.0721687836487033,0.,0.125));
#62383=CARTESIAN_POINT('',(-0.0627109795608791,0.,0.141381397208144));
#62384=CARTESIAN_POINT('',(-0.0721687836487033,-0.25,0.125));
#62385=CARTESIAN_POINT('',(-0.0721687836487033,0.,0.125));
#62386=CARTESIAN_POINT('',(-0.144337567297406,-0.25,-1.76762539787485E-17));
#62387=CARTESIAN_POINT('Origin',(0.0721687836487032,0.,0.125));
#62388=CARTESIAN_POINT('',(0.0721687836487032,0.,0.125));
#62389=CARTESIAN_POINT('',(0.146084391824352,0.,0.125));
#62390=CARTESIAN_POINT('',(0.0721687836487032,-0.25,0.125));
#62391=CARTESIAN_POINT('',(0.0721687836487032,0.,0.125));
#62392=CARTESIAN_POINT('',(-0.0721687836487033,-0.25,0.125));
#62393=CARTESIAN_POINT('Origin',(0.144337567297406,0.,0.));
#62394=CARTESIAN_POINT('',(0.153795371385231,0.,-0.0163813972081441));
#62395=CARTESIAN_POINT('',(0.0721687836487032,-0.25,0.125));
#62396=CARTESIAN_POINT('Origin',(0.,-0.25,0.));
#62397=CARTESIAN_POINT('Origin',(0.22,0.,0.));
#62398=CARTESIAN_POINT('',(-0.22,-8.67361737988404E-18,-2.69422295812418E-17));
#62399=CARTESIAN_POINT('Origin',(0.,0.,0.));
#62400=CARTESIAN_POINT('Origin',(0.,-0.015,0.));
#62401=CARTESIAN_POINT('',(-0.24505,-0.02505,-3.00099698131059E-17));
#62402=CARTESIAN_POINT('Origin',(0.,-0.02505,0.));
#62403=CARTESIAN_POINT('',(-0.235,-0.015,-2.87791997799628E-17));
#62404=CARTESIAN_POINT('Origin',(0.,-0.3775,0.));
#62405=CARTESIAN_POINT('',(-0.24505,-0.72995,3.00099698131059E-17));
#62406=CARTESIAN_POINT('Origin',(0.,-0.72995,0.));
#62407=CARTESIAN_POINT('',(-0.24505,-0.3775,-3.00099698131059E-17));
#62408=CARTESIAN_POINT('Origin',(0.,-0.7625,0.));
#62409=CARTESIAN_POINT('',(-0.175,-0.8,-2.14313189850787E-17));
#62410=CARTESIAN_POINT('Origin',(0.,-0.8,0.));
#62411=CARTESIAN_POINT('',(-0.2125,-0.7625,-2.60237444818813E-17));
#62412=CARTESIAN_POINT('Origin',(0.,-0.8,0.));
#62413=CARTESIAN_POINT('',(0.,0.,0.));
#62414=CARTESIAN_POINT('Origin',(0.3,0.4,0.));
#62415=CARTESIAN_POINT('',(-0.3,0.4,-3.67394039744206E-17));
#62416=CARTESIAN_POINT('Origin',(0.,0.4,0.));
#62417=CARTESIAN_POINT('Origin',(0.,0.375,0.));
#62418=CARTESIAN_POINT('',(-0.35,0.35,-4.28626379701573E-17));
#62419=CARTESIAN_POINT('Origin',(0.,0.35,0.));
#62420=CARTESIAN_POINT('',(-0.325,0.375,-3.9801020972289E-17));
#62421=CARTESIAN_POINT('Origin',(0.,0.19,0.));
#62422=CARTESIAN_POINT('',(-0.35,0.03,-4.28626379701574E-17));
#62423=CARTESIAN_POINT('Origin',(0.,0.03,0.));
#62424=CARTESIAN_POINT('',(-0.35,0.19,-4.28626379701574E-17));
#62425=CARTESIAN_POINT('Origin',(0.,0.0149999999999999,0.));
#62426=CARTESIAN_POINT('',(-0.32,-3.29597460435593E-17,-3.91886975727153E-17));
#62427=CARTESIAN_POINT('Origin',(0.,0.,0.));
#62428=CARTESIAN_POINT('',(-0.335,0.0149999999999999,-4.10256677714363E-17));
#62429=CARTESIAN_POINT('Origin',(0.22,0.,0.));
#62430=CARTESIAN_POINT('',(-0.22,-6.93889390390723E-18,-2.69422295812418E-17));
#62431=CARTESIAN_POINT('Origin',(0.,0.,0.));
#62432=CARTESIAN_POINT('Origin',(0.,-0.02,0.));
#62433=CARTESIAN_POINT('',(-0.1954,-0.0492,2.39295984553393E-17));
#62434=CARTESIAN_POINT('Origin',(0.,-0.0492,0.));
#62435=CARTESIAN_POINT('',(-0.21,-0.02,-2.57175827820944E-17));
#62436=CARTESIAN_POINT('Origin',(0.,-0.8,0.));
#62437=CARTESIAN_POINT('',(-0.1954,-1.5646,2.39295984553393E-17));
#62438=CARTESIAN_POINT('Origin',(0.,-1.5646,0.));
#62439=CARTESIAN_POINT('',(-0.1954,-0.8,-2.39295984553393E-17));
#62440=CARTESIAN_POINT('Origin',(0.,-1.58,0.));
#62441=CARTESIAN_POINT('',(-0.16,-1.6,-1.95943487863577E-17));
#62442=CARTESIAN_POINT('Origin',(0.,-1.6,0.));
#62443=CARTESIAN_POINT('',(-0.18,-1.58,-2.20436423846524E-17));
#62444=CARTESIAN_POINT('Origin',(0.,-1.6,0.));
#62445=CARTESIAN_POINT('Origin',(0.0866025403784439,-0.4,-0.15));
#62446=CARTESIAN_POINT('',(0.173205080756888,-0.4,0.));
#62447=CARTESIAN_POINT('',(0.0866025403784439,-0.4,-0.15));
#62448=CARTESIAN_POINT('',(0.173205080756888,-0.4,0.));
#62449=CARTESIAN_POINT('',(0.0866025403784439,-0.64,-0.15));
#62450=CARTESIAN_POINT('',(0.0866025403784439,-0.4,-0.15));
#62451=CARTESIAN_POINT('',(0.173205080756888,-0.64,0.));
#62452=CARTESIAN_POINT('',(0.173205080756888,-0.64,0.));
#62453=CARTESIAN_POINT('',(0.173205080756888,-0.4,0.));
#62454=CARTESIAN_POINT('Origin',(-0.0866025403784438,-0.4,-0.15));
#62455=CARTESIAN_POINT('',(-0.0866025403784438,-0.4,-0.15));
#62456=CARTESIAN_POINT('',(0.0866025403784439,-0.4,-0.15));
#62457=CARTESIAN_POINT('',(-0.0866025403784438,-0.64,-0.15));
#62458=CARTESIAN_POINT('',(-0.0866025403784438,-0.4,-0.15));
#62459=CARTESIAN_POINT('',(0.0866025403784439,-0.64,-0.15));
#62460=CARTESIAN_POINT('Origin',(-0.173205080756888,-0.4,-2.77555756156289E-17));
#62461=CARTESIAN_POINT('',(-0.173205080756888,-0.4,-2.12115047744981E-17));
#62462=CARTESIAN_POINT('',(-0.0866025403784438,-0.4,-0.15));
#62463=CARTESIAN_POINT('',(-0.173205080756888,-0.64,-2.77555756156289E-17));
#62464=CARTESIAN_POINT('',(-0.173205080756888,-0.4,-2.12115047744981E-17));
#62465=CARTESIAN_POINT('',(-0.0866025403784438,-0.64,-0.15));
#62466=CARTESIAN_POINT('Origin',(-0.0866025403784439,-0.4,0.15));
#62467=CARTESIAN_POINT('',(-0.0866025403784439,-0.4,0.15));
#62468=CARTESIAN_POINT('',(-0.173205080756888,-0.4,-2.12115047744981E-17));
#62469=CARTESIAN_POINT('',(-0.0866025403784439,-0.64,0.15));
#62470=CARTESIAN_POINT('',(-0.0866025403784439,-0.4,0.15));
#62471=CARTESIAN_POINT('',(-0.173205080756888,-0.64,-2.12115047744981E-17));
#62472=CARTESIAN_POINT('Origin',(0.0866025403784439,-0.4,0.15));
#62473=CARTESIAN_POINT('',(0.0866025403784439,-0.4,0.15));
#62474=CARTESIAN_POINT('',(-0.0866025403784439,-0.4,0.15));
#62475=CARTESIAN_POINT('',(0.0866025403784439,-0.64,0.15));
#62476=CARTESIAN_POINT('',(0.0866025403784439,-0.4,0.15));
#62477=CARTESIAN_POINT('',(-0.0866025403784439,-0.64,0.15));
#62478=CARTESIAN_POINT('Origin',(0.173205080756888,-0.4,0.));
#62479=CARTESIAN_POINT('',(0.0866025403784439,-0.4,0.15));
#62480=CARTESIAN_POINT('',(0.0866025403784439,-0.64,0.15));
#62481=CARTESIAN_POINT('Origin',(0.,-0.4,-2.77555756156289E-17));
#62482=CARTESIAN_POINT('Origin',(0.,-0.64,-2.77555756156289E-17));
#62483=CARTESIAN_POINT('',(0.,0.,0.));
#62484=CARTESIAN_POINT('',(0.,0.,0.));
#62485=CARTESIAN_POINT('',(0.,0.,0.));
#62486=CARTESIAN_POINT('',(0.,0.,0.));
#62487=CARTESIAN_POINT('',(0.,0.,0.));
#62488=CARTESIAN_POINT('',(0.,0.,0.));
#62489=CARTESIAN_POINT('',(-2.,-5.,2.));
#62490=CARTESIAN_POINT('',(9.,-5.,2.));
#62491=CARTESIAN_POINT('',(22.,-5.,2.));
#62492=CARTESIAN_POINT('',(0.,-1.5,9.));
#62493=CARTESIAN_POINT('',(1.48492424049175,-2.6,10.4849242404918));
#62494=CARTESIAN_POINT('',(-1.48492424049175,-2.6,10.4849242404918));
#62495=CARTESIAN_POINT('',(-1.48492424049175,-2.6,7.51507575950825));
#62496=CARTESIAN_POINT('',(1.48492424049175,-2.6,7.51507575950825));
#62497=CARTESIAN_POINT('',(1.48492424049175,-0.4,10.4849242404918));
#62498=CARTESIAN_POINT('',(-1.48492424049175,-0.4,10.4849242404918));
#62499=CARTESIAN_POINT('',(-1.48492424049175,-0.4,7.51507575950825));
#62500=CARTESIAN_POINT('',(1.48492424049175,-0.4,7.51507575950825));
#62501=CARTESIAN_POINT('',(6.,-1.5,9.));
#62502=CARTESIAN_POINT('',(7.83847763108502,-2.6,10.838477631085));
#62503=CARTESIAN_POINT('',(4.16152236891498,-2.6,10.838477631085));
#62504=CARTESIAN_POINT('',(4.16152236891497,-2.6,7.16152236891498));
#62505=CARTESIAN_POINT('',(7.83847763108502,-2.6,7.16152236891498));
#62506=CARTESIAN_POINT('',(7.83847763108502,-0.4,10.838477631085));
#62507=CARTESIAN_POINT('',(4.16152236891498,-0.4,10.838477631085));
#62508=CARTESIAN_POINT('',(4.16152236891498,-0.4,7.16152236891498));
#62509=CARTESIAN_POINT('',(7.83847763108502,-0.4,7.16152236891498));
#62510=CARTESIAN_POINT('',(0.,0.,0.));
#62511=CARTESIAN_POINT('',(0.,0.,0.));
#62512=CARTESIAN_POINT('',(0.,0.,0.));
#62513=CARTESIAN_POINT('',(0.,0.,0.));
#62514=CARTESIAN_POINT('',(12.,-1.5,9.));
#62515=CARTESIAN_POINT('',(13.4849242404918,-2.6,10.4849242404918));
#62516=CARTESIAN_POINT('',(10.5150757595082,-2.6,10.4849242404918));
#62517=CARTESIAN_POINT('',(10.5150757595082,-2.6,7.51507575950825));
#62518=CARTESIAN_POINT('',(13.4849242404918,-2.6,7.51507575950825));
#62519=CARTESIAN_POINT('',(13.4849242404918,-0.399999999999999,10.4849242404918));
#62520=CARTESIAN_POINT('',(10.5150757595082,-0.399999999999999,10.4849242404918));
#62521=CARTESIAN_POINT('',(10.5150757595082,-0.399999999999999,7.51507575950825));
#62522=CARTESIAN_POINT('',(13.4849242404918,-0.399999999999999,7.51507575950825));
#62523=CARTESIAN_POINT('',(18.,-1.5,9.));
#62524=CARTESIAN_POINT('',(19.838477631085,-2.6,10.838477631085));
#62525=CARTESIAN_POINT('',(16.161522368915,-2.6,10.838477631085));
#62526=CARTESIAN_POINT('',(16.161522368915,-2.6,7.16152236891498));
#62527=CARTESIAN_POINT('',(19.838477631085,-2.6,7.16152236891498));
#62528=CARTESIAN_POINT('',(19.838477631085,-0.4,10.838477631085));
#62529=CARTESIAN_POINT('',(16.161522368915,-0.4,10.838477631085));
#62530=CARTESIAN_POINT('',(16.161522368915,-0.4,7.16152236891498));
#62531=CARTESIAN_POINT('',(19.838477631085,-0.4,7.16152236891498));
#62532=CARTESIAN_POINT('',(0.,0.,0.));
#62533=CARTESIAN_POINT('',(0.,0.,0.));
#62534=CARTESIAN_POINT('',(0.,0.,0.));
#62535=CARTESIAN_POINT('',(0.,0.,0.));
#62536=CARTESIAN_POINT('',(0.,0.,0.));
#62537=CARTESIAN_POINT('',(23.,4.2,4.));
#62538=CARTESIAN_POINT('',(23.,-2.4,4.));
#62539=CARTESIAN_POINT('',(23.,4.2,14.));
#62540=CARTESIAN_POINT('',(23.,-2.4,14.));
#62541=CARTESIAN_POINT('',(0.,0.,0.));
#62542=CARTESIAN_POINT('',(0.,0.,0.));
#62543=CARTESIAN_POINT('',(0.,0.,0.));
#62544=CARTESIAN_POINT('',(0.,0.,0.));
#62545=CARTESIAN_POINT('',(0.,0.,0.));
#62546=CARTESIAN_POINT('',(0.,0.,0.));
#62547=CARTESIAN_POINT('',(0.,0.,0.));
#62548=CARTESIAN_POINT('',(0.,0.,0.));
#62549=CARTESIAN_POINT('',(0.,0.,0.));
#62550=CARTESIAN_POINT('',(0.,-3.2,10.4));
#62551=CARTESIAN_POINT('',(0.,1.,9.));
#62552=CARTESIAN_POINT('',(0.,1.6,8.65));
#62553=CARTESIAN_POINT('',(0.,4.6,8.65));
#62554=CARTESIAN_POINT('',(0.,6.2,9.));
#62555=CARTESIAN_POINT('',(0.,6.8,13.));
#62556=CARTESIAN_POINT('',(0.,6.96,13.));
#62557=CARTESIAN_POINT('',(0.,0.,0.));
#62558=CARTESIAN_POINT('',(0.,0.,0.));
#62559=CARTESIAN_POINT('',(0.,0.,0.));
#62560=CARTESIAN_POINT('',(0.,0.,0.));
#62561=CARTESIAN_POINT('',(0.,0.,0.));
#62562=CARTESIAN_POINT('',(6.,-3.2,10.8));
#62563=CARTESIAN_POINT('',(6.,1.,9.));
#62564=CARTESIAN_POINT('',(6.,1.6,8.35));
#62565=CARTESIAN_POINT('',(6.,3.4,9.));
#62566=CARTESIAN_POINT('',(0.,0.,0.));
#62567=CARTESIAN_POINT('',(0.,0.,0.));
#62568=CARTESIAN_POINT('',(0.,0.,0.));
#62569=CARTESIAN_POINT('',(0.,0.,0.));
#62570=CARTESIAN_POINT('',(0.,0.,0.));
#62571=CARTESIAN_POINT('',(12.,-3.2,10.4));
#62572=CARTESIAN_POINT('',(12.,1.,9.));
#62573=CARTESIAN_POINT('',(12.,1.6,8.65));
#62574=CARTESIAN_POINT('',(12.,3.4,9.));
#62575=CARTESIAN_POINT('',(0.,0.,0.));
#62576=CARTESIAN_POINT('',(0.,0.,0.));
#62577=CARTESIAN_POINT('',(0.,0.,0.));
#62578=CARTESIAN_POINT('',(0.,0.,0.));
#62579=CARTESIAN_POINT('',(0.,0.,0.));
#62580=CARTESIAN_POINT('',(0.,0.,0.));
#62581=CARTESIAN_POINT('',(0.,0.,0.));
#62582=CARTESIAN_POINT('',(0.,0.,0.));
#62583=CARTESIAN_POINT('',(18.,-3.2,10.8));
#62584=CARTESIAN_POINT('',(18.,1.,9.));
#62585=CARTESIAN_POINT('',(18.,1.6,8.35));
#62586=CARTESIAN_POINT('',(18.,4.8,10.8));
#62587=CARTESIAN_POINT('',(18.,6.2,9.));
#62588=CARTESIAN_POINT('',(0.,0.,0.));
#62589=CARTESIAN_POINT('',(0.,0.,0.));
#62590=CARTESIAN_POINT('Origin',(0.,4.8,13.));
#62591=CARTESIAN_POINT('',(-0.405,6.77,13.));
#62592=CARTESIAN_POINT('Origin',(0.,6.77,13.));
#62593=CARTESIAN_POINT('',(-0.405,4.8,13.));
#62594=CARTESIAN_POINT('',(-0.405,4.8,13.));
#62595=CARTESIAN_POINT('Origin',(0.,4.8,13.));
#62596=CARTESIAN_POINT('Origin',(0.,4.8,13.));
#62597=CARTESIAN_POINT('',(-0.9,6.77,13.));
#62598=CARTESIAN_POINT('Origin',(0.,6.77,13.));
#62599=CARTESIAN_POINT('',(-0.9,4.8,13.));
#62600=CARTESIAN_POINT('',(-0.9,4.8,13.));
#62601=CARTESIAN_POINT('Origin',(0.,4.8,13.));
#62602=CARTESIAN_POINT('Origin',(0.,6.77,13.));
#62603=CARTESIAN_POINT('Origin',(0.,4.8,13.));
#62604=CARTESIAN_POINT('',(0.,0.,0.));
#62605=CARTESIAN_POINT('',(0.,0.,0.));
#62606=CARTESIAN_POINT('',(0.,0.,0.));
#62607=CARTESIAN_POINT('',(-0.687635863949372,0.,0.498498570768918));
#62608=CARTESIAN_POINT('',(0.,0.,0.));
#62609=CARTESIAN_POINT('',(-0.650643868746908,0.,1.44000771950306));
#62610=CARTESIAN_POINT('',(0.,0.,0.));
#62611=UNCERTAINTY_MEASURE_WITH_UNIT(LENGTH_MEASURE(0.001),#62759,
'DISTANCE_ACCURACY_VALUE',
'Maximum model space distance between geometric entities at asserted c
onnectivities');
#62612=UNCERTAINTY_MEASURE_WITH_UNIT(LENGTH_MEASURE(0.001),#62759,
'DISTANCE_ACCURACY_VALUE',
'Maximum model space distance between geometric entities at asserted c
onnectivities');
#62613=UNCERTAINTY_MEASURE_WITH_UNIT(LENGTH_MEASURE(0.001),#62759,
'DISTANCE_ACCURACY_VALUE',
'Maximum model space distance between geometric entities at asserted c
onnectivities');
#62614=UNCERTAINTY_MEASURE_WITH_UNIT(LENGTH_MEASURE(0.001),#62759,
'DISTANCE_ACCURACY_VALUE',
'Maximum model space distance between geometric entities at asserted c
onnectivities');
#62615=UNCERTAINTY_MEASURE_WITH_UNIT(LENGTH_MEASURE(0.001),#62759,
'DISTANCE_ACCURACY_VALUE',
'Maximum model space distance between geometric entities at asserted c
onnectivities');
#62616=UNCERTAINTY_MEASURE_WITH_UNIT(LENGTH_MEASURE(0.001),#62759,
'DISTANCE_ACCURACY_VALUE',
'Maximum model space distance between geometric entities at asserted c
onnectivities');
#62617=UNCERTAINTY_MEASURE_WITH_UNIT(LENGTH_MEASURE(0.001),#62759,
'DISTANCE_ACCURACY_VALUE',
'Maximum model space distance between geometric entities at asserted c
onnectivities');
#62618=UNCERTAINTY_MEASURE_WITH_UNIT(LENGTH_MEASURE(0.001),#62759,
'DISTANCE_ACCURACY_VALUE',
'Maximum model space distance between geometric entities at asserted c
onnectivities');
#62619=UNCERTAINTY_MEASURE_WITH_UNIT(LENGTH_MEASURE(0.001),#62759,
'DISTANCE_ACCURACY_VALUE',
'Maximum model space distance between geometric entities at asserted c
onnectivities');
#62620=UNCERTAINTY_MEASURE_WITH_UNIT(LENGTH_MEASURE(0.001),#62759,
'DISTANCE_ACCURACY_VALUE',
'Maximum model space distance between geometric entities at asserted c
onnectivities');
#62621=UNCERTAINTY_MEASURE_WITH_UNIT(LENGTH_MEASURE(0.001),#62759,
'DISTANCE_ACCURACY_VALUE',
'Maximum model space distance between geometric entities at asserted c
onnectivities');
#62622=UNCERTAINTY_MEASURE_WITH_UNIT(LENGTH_MEASURE(0.001),#62759,
'DISTANCE_ACCURACY_VALUE',
'Maximum model space distance between geometric entities at asserted c
onnectivities');
#62623=UNCERTAINTY_MEASURE_WITH_UNIT(LENGTH_MEASURE(0.001),#62759,
'DISTANCE_ACCURACY_VALUE',
'Maximum model space distance between geometric entities at asserted c
onnectivities');
#62624=UNCERTAINTY_MEASURE_WITH_UNIT(LENGTH_MEASURE(0.001),#62759,
'DISTANCE_ACCURACY_VALUE',
'Maximum model space distance between geometric entities at asserted c
onnectivities');
#62625=UNCERTAINTY_MEASURE_WITH_UNIT(LENGTH_MEASURE(0.001),#62759,
'DISTANCE_ACCURACY_VALUE',
'Maximum model space distance between geometric entities at asserted c
onnectivities');
#62626=UNCERTAINTY_MEASURE_WITH_UNIT(LENGTH_MEASURE(0.001),#62759,
'DISTANCE_ACCURACY_VALUE',
'Maximum model space distance between geometric entities at asserted c
onnectivities');
#62627=UNCERTAINTY_MEASURE_WITH_UNIT(LENGTH_MEASURE(0.001),#62759,
'DISTANCE_ACCURACY_VALUE',
'Maximum model space distance between geometric entities at asserted c
onnectivities');
#62628=UNCERTAINTY_MEASURE_WITH_UNIT(LENGTH_MEASURE(0.001),#62759,
'DISTANCE_ACCURACY_VALUE',
'Maximum model space distance between geometric entities at asserted c
onnectivities');
#62629=UNCERTAINTY_MEASURE_WITH_UNIT(LENGTH_MEASURE(0.001),#62759,
'DISTANCE_ACCURACY_VALUE',
'Maximum model space distance between geometric entities at asserted c
onnectivities');
#62630=UNCERTAINTY_MEASURE_WITH_UNIT(LENGTH_MEASURE(0.001),#62759,
'DISTANCE_ACCURACY_VALUE',
'Maximum model space distance between geometric entities at asserted c
onnectivities');
#62631=UNCERTAINTY_MEASURE_WITH_UNIT(LENGTH_MEASURE(0.001),#62759,
'DISTANCE_ACCURACY_VALUE',
'Maximum model space distance between geometric entities at asserted c
onnectivities');
#62632=UNCERTAINTY_MEASURE_WITH_UNIT(LENGTH_MEASURE(0.001),#62759,
'DISTANCE_ACCURACY_VALUE',
'Maximum model space distance between geometric entities at asserted c
onnectivities');
#62633=UNCERTAINTY_MEASURE_WITH_UNIT(LENGTH_MEASURE(0.001),#62759,
'DISTANCE_ACCURACY_VALUE',
'Maximum model space distance between geometric entities at asserted c
onnectivities');
#62634=UNCERTAINTY_MEASURE_WITH_UNIT(LENGTH_MEASURE(0.001),#62759,
'DISTANCE_ACCURACY_VALUE',
'Maximum model space distance between geometric entities at asserted c
onnectivities');
#62635=UNCERTAINTY_MEASURE_WITH_UNIT(LENGTH_MEASURE(0.001),#62759,
'DISTANCE_ACCURACY_VALUE',
'Maximum model space distance between geometric entities at asserted c
onnectivities');
#62636=UNCERTAINTY_MEASURE_WITH_UNIT(LENGTH_MEASURE(0.001),#62759,
'DISTANCE_ACCURACY_VALUE',
'Maximum model space distance between geometric entities at asserted c
onnectivities');
#62637=UNCERTAINTY_MEASURE_WITH_UNIT(LENGTH_MEASURE(0.001),#62759,
'DISTANCE_ACCURACY_VALUE',
'Maximum model space distance between geometric entities at asserted c
onnectivities');
#62638=UNCERTAINTY_MEASURE_WITH_UNIT(LENGTH_MEASURE(0.001),#62759,
'DISTANCE_ACCURACY_VALUE',
'Maximum model space distance between geometric entities at asserted c
onnectivities');
#62639=UNCERTAINTY_MEASURE_WITH_UNIT(LENGTH_MEASURE(0.001),#62759,
'DISTANCE_ACCURACY_VALUE',
'Maximum model space distance between geometric entities at asserted c
onnectivities');
#62640=UNCERTAINTY_MEASURE_WITH_UNIT(LENGTH_MEASURE(0.001),#62759,
'DISTANCE_ACCURACY_VALUE',
'Maximum model space distance between geometric entities at asserted c
onnectivities');
#62641=UNCERTAINTY_MEASURE_WITH_UNIT(LENGTH_MEASURE(0.001),#62759,
'DISTANCE_ACCURACY_VALUE',
'Maximum model space distance between geometric entities at asserted c
onnectivities');
#62642=UNCERTAINTY_MEASURE_WITH_UNIT(LENGTH_MEASURE(0.001),#62759,
'DISTANCE_ACCURACY_VALUE',
'Maximum model space distance between geometric entities at asserted c
onnectivities');
#62643=UNCERTAINTY_MEASURE_WITH_UNIT(LENGTH_MEASURE(0.001),#62759,
'DISTANCE_ACCURACY_VALUE',
'Maximum model space distance between geometric entities at asserted c
onnectivities');
#62644=UNCERTAINTY_MEASURE_WITH_UNIT(LENGTH_MEASURE(0.001),#62759,
'DISTANCE_ACCURACY_VALUE',
'Maximum model space distance between geometric entities at asserted c
onnectivities');
#62645=UNCERTAINTY_MEASURE_WITH_UNIT(LENGTH_MEASURE(0.001),#62759,
'DISTANCE_ACCURACY_VALUE',
'Maximum model space distance between geometric entities at asserted c
onnectivities');
#62646=UNCERTAINTY_MEASURE_WITH_UNIT(LENGTH_MEASURE(0.001),#62759,
'DISTANCE_ACCURACY_VALUE',
'Maximum model space distance between geometric entities at asserted c
onnectivities');
#62647=UNCERTAINTY_MEASURE_WITH_UNIT(LENGTH_MEASURE(0.001),#62759,
'DISTANCE_ACCURACY_VALUE',
'Maximum model space distance between geometric entities at asserted c
onnectivities');
#62648=UNCERTAINTY_MEASURE_WITH_UNIT(LENGTH_MEASURE(0.001),#62759,
'DISTANCE_ACCURACY_VALUE',
'Maximum model space distance between geometric entities at asserted c
onnectivities');
#62649=UNCERTAINTY_MEASURE_WITH_UNIT(LENGTH_MEASURE(0.001),#62759,
'DISTANCE_ACCURACY_VALUE',
'Maximum model space distance between geometric entities at asserted c
onnectivities');
#62650=UNCERTAINTY_MEASURE_WITH_UNIT(LENGTH_MEASURE(0.001),#62759,
'DISTANCE_ACCURACY_VALUE',
'Maximum model space distance between geometric entities at asserted c
onnectivities');
#62651=UNCERTAINTY_MEASURE_WITH_UNIT(LENGTH_MEASURE(0.001),#62759,
'DISTANCE_ACCURACY_VALUE',
'Maximum model space distance between geometric entities at asserted c
onnectivities');
#62652=UNCERTAINTY_MEASURE_WITH_UNIT(LENGTH_MEASURE(0.001),#62759,
'DISTANCE_ACCURACY_VALUE',
'Maximum model space distance between geometric entities at asserted c
onnectivities');
#62653=UNCERTAINTY_MEASURE_WITH_UNIT(LENGTH_MEASURE(0.001),#62759,
'DISTANCE_ACCURACY_VALUE',
'Maximum model space distance between geometric entities at asserted c
onnectivities');
#62654=UNCERTAINTY_MEASURE_WITH_UNIT(LENGTH_MEASURE(0.001),#62759,
'DISTANCE_ACCURACY_VALUE',
'Maximum model space distance between geometric entities at asserted c
onnectivities');
#62655=UNCERTAINTY_MEASURE_WITH_UNIT(LENGTH_MEASURE(0.001),#62759,
'DISTANCE_ACCURACY_VALUE',
'Maximum model space distance between geometric entities at asserted c
onnectivities');
#62656=UNCERTAINTY_MEASURE_WITH_UNIT(LENGTH_MEASURE(0.001),#62759,
'DISTANCE_ACCURACY_VALUE',
'Maximum model space distance between geometric entities at asserted c
onnectivities');
#62657=UNCERTAINTY_MEASURE_WITH_UNIT(LENGTH_MEASURE(0.001),#62759,
'DISTANCE_ACCURACY_VALUE',
'Maximum model space distance between geometric entities at asserted c
onnectivities');
#62658=UNCERTAINTY_MEASURE_WITH_UNIT(LENGTH_MEASURE(0.001),#62759,
'DISTANCE_ACCURACY_VALUE',
'Maximum model space distance between geometric entities at asserted c
onnectivities');
#62659=UNCERTAINTY_MEASURE_WITH_UNIT(LENGTH_MEASURE(0.001),#62759,
'DISTANCE_ACCURACY_VALUE',
'Maximum model space distance between geometric entities at asserted c
onnectivities');
#62660=UNCERTAINTY_MEASURE_WITH_UNIT(LENGTH_MEASURE(0.001),#62759,
'DISTANCE_ACCURACY_VALUE',
'Maximum model space distance between geometric entities at asserted c
onnectivities');
#62661=UNCERTAINTY_MEASURE_WITH_UNIT(LENGTH_MEASURE(0.001),#62759,
'DISTANCE_ACCURACY_VALUE',
'Maximum model space distance between geometric entities at asserted c
onnectivities');
#62662=UNCERTAINTY_MEASURE_WITH_UNIT(LENGTH_MEASURE(0.001),#62759,
'DISTANCE_ACCURACY_VALUE',
'Maximum model space distance between geometric entities at asserted c
onnectivities');
#62663=UNCERTAINTY_MEASURE_WITH_UNIT(LENGTH_MEASURE(0.001),#62759,
'DISTANCE_ACCURACY_VALUE',
'Maximum model space distance between geometric entities at asserted c
onnectivities');
#62664=UNCERTAINTY_MEASURE_WITH_UNIT(LENGTH_MEASURE(0.001),#62759,
'DISTANCE_ACCURACY_VALUE',
'Maximum model space distance between geometric entities at asserted c
onnectivities');
#62665=UNCERTAINTY_MEASURE_WITH_UNIT(LENGTH_MEASURE(0.001),#62759,
'DISTANCE_ACCURACY_VALUE',
'Maximum model space distance between geometric entities at asserted c
onnectivities');
#62666=UNCERTAINTY_MEASURE_WITH_UNIT(LENGTH_MEASURE(0.001),#62759,
'DISTANCE_ACCURACY_VALUE',
'Maximum model space distance between geometric entities at asserted c
onnectivities');
#62667=UNCERTAINTY_MEASURE_WITH_UNIT(LENGTH_MEASURE(0.001),#62759,
'DISTANCE_ACCURACY_VALUE',
'Maximum model space distance between geometric entities at asserted c
onnectivities');
#62668=UNCERTAINTY_MEASURE_WITH_UNIT(LENGTH_MEASURE(0.001),#62759,
'DISTANCE_ACCURACY_VALUE',
'Maximum model space distance between geometric entities at asserted c
onnectivities');
#62669=UNCERTAINTY_MEASURE_WITH_UNIT(LENGTH_MEASURE(0.001),#62759,
'DISTANCE_ACCURACY_VALUE',
'Maximum model space distance between geometric entities at asserted c
onnectivities');
#62670=UNCERTAINTY_MEASURE_WITH_UNIT(LENGTH_MEASURE(0.001),#62759,
'DISTANCE_ACCURACY_VALUE',
'Maximum model space distance between geometric entities at asserted c
onnectivities');
#62671=UNCERTAINTY_MEASURE_WITH_UNIT(LENGTH_MEASURE(0.001),#62759,
'DISTANCE_ACCURACY_VALUE',
'Maximum model space distance between geometric entities at asserted c
onnectivities');
#62672=UNCERTAINTY_MEASURE_WITH_UNIT(LENGTH_MEASURE(0.001),#62759,
'DISTANCE_ACCURACY_VALUE',
'Maximum model space distance between geometric entities at asserted c
onnectivities');
#62673=UNCERTAINTY_MEASURE_WITH_UNIT(LENGTH_MEASURE(0.001),#62759,
'DISTANCE_ACCURACY_VALUE',
'Maximum model space distance between geometric entities at asserted c
onnectivities');
#62674=UNCERTAINTY_MEASURE_WITH_UNIT(LENGTH_MEASURE(0.001),#62759,
'DISTANCE_ACCURACY_VALUE',
'Maximum model space distance between geometric entities at asserted c
onnectivities');
#62675=UNCERTAINTY_MEASURE_WITH_UNIT(LENGTH_MEASURE(0.001),#62759,
'DISTANCE_ACCURACY_VALUE',
'Maximum model space distance between geometric entities at asserted c
onnectivities');
#62676=UNCERTAINTY_MEASURE_WITH_UNIT(LENGTH_MEASURE(0.001),#62759,
'DISTANCE_ACCURACY_VALUE',
'Maximum model space distance between geometric entities at asserted c
onnectivities');
#62677=UNCERTAINTY_MEASURE_WITH_UNIT(LENGTH_MEASURE(0.001),#62759,
'DISTANCE_ACCURACY_VALUE',
'Maximum model space distance between geometric entities at asserted c
onnectivities');
#62678=UNCERTAINTY_MEASURE_WITH_UNIT(LENGTH_MEASURE(0.001),#62759,
'DISTANCE_ACCURACY_VALUE',
'Maximum model space distance between geometric entities at asserted c
onnectivities');
#62679=UNCERTAINTY_MEASURE_WITH_UNIT(LENGTH_MEASURE(0.001),#62759,
'DISTANCE_ACCURACY_VALUE',
'Maximum model space distance between geometric entities at asserted c
onnectivities');
#62680=UNCERTAINTY_MEASURE_WITH_UNIT(LENGTH_MEASURE(0.001),#62759,
'DISTANCE_ACCURACY_VALUE',
'Maximum model space distance between geometric entities at asserted c
onnectivities');
#62681=UNCERTAINTY_MEASURE_WITH_UNIT(LENGTH_MEASURE(0.001),#62759,
'DISTANCE_ACCURACY_VALUE',
'Maximum model space distance between geometric entities at asserted c
onnectivities');
#62682=UNCERTAINTY_MEASURE_WITH_UNIT(LENGTH_MEASURE(0.001),#62759,
'DISTANCE_ACCURACY_VALUE',
'Maximum model space distance between geometric entities at asserted c
onnectivities');
#62683=UNCERTAINTY_MEASURE_WITH_UNIT(LENGTH_MEASURE(0.001),#62759,
'DISTANCE_ACCURACY_VALUE',
'Maximum model space distance between geometric entities at asserted c
onnectivities');
#62684=UNCERTAINTY_MEASURE_WITH_UNIT(LENGTH_MEASURE(0.001),#62759,
'DISTANCE_ACCURACY_VALUE',
'Maximum model space distance between geometric entities at asserted c
onnectivities');
#62685=(
GEOMETRIC_REPRESENTATION_CONTEXT(3)
GLOBAL_UNCERTAINTY_ASSIGNED_CONTEXT((#62611))
GLOBAL_UNIT_ASSIGNED_CONTEXT((#62759,#62761,#62762))
REPRESENTATION_CONTEXT('','3D')
);
#62686=(
GEOMETRIC_REPRESENTATION_CONTEXT(3)
GLOBAL_UNCERTAINTY_ASSIGNED_CONTEXT((#62612))
GLOBAL_UNIT_ASSIGNED_CONTEXT((#62759,#62761,#62762))
REPRESENTATION_CONTEXT('','3D')
);
#62687=(
GEOMETRIC_REPRESENTATION_CONTEXT(3)
GLOBAL_UNCERTAINTY_ASSIGNED_CONTEXT((#62613))
GLOBAL_UNIT_ASSIGNED_CONTEXT((#62759,#62761,#62762))
REPRESENTATION_CONTEXT('','3D')
);
#62688=(
GEOMETRIC_REPRESENTATION_CONTEXT(3)
GLOBAL_UNCERTAINTY_ASSIGNED_CONTEXT((#62614))
GLOBAL_UNIT_ASSIGNED_CONTEXT((#62759,#62761,#62762))
REPRESENTATION_CONTEXT('','3D')
);
#62689=(
GEOMETRIC_REPRESENTATION_CONTEXT(3)
GLOBAL_UNCERTAINTY_ASSIGNED_CONTEXT((#62615))
GLOBAL_UNIT_ASSIGNED_CONTEXT((#62759,#62761,#62762))
REPRESENTATION_CONTEXT('','3D')
);
#62690=(
GEOMETRIC_REPRESENTATION_CONTEXT(3)
GLOBAL_UNCERTAINTY_ASSIGNED_CONTEXT((#62616))
GLOBAL_UNIT_ASSIGNED_CONTEXT((#62759,#62761,#62762))
REPRESENTATION_CONTEXT('','3D')
);
#62691=(
GEOMETRIC_REPRESENTATION_CONTEXT(3)
GLOBAL_UNCERTAINTY_ASSIGNED_CONTEXT((#62617))
GLOBAL_UNIT_ASSIGNED_CONTEXT((#62759,#62761,#62762))
REPRESENTATION_CONTEXT('','3D')
);
#62692=(
GEOMETRIC_REPRESENTATION_CONTEXT(3)
GLOBAL_UNCERTAINTY_ASSIGNED_CONTEXT((#62618))
GLOBAL_UNIT_ASSIGNED_CONTEXT((#62759,#62761,#62762))
REPRESENTATION_CONTEXT('','3D')
);
#62693=(
GEOMETRIC_REPRESENTATION_CONTEXT(3)
GLOBAL_UNCERTAINTY_ASSIGNED_CONTEXT((#62619))
GLOBAL_UNIT_ASSIGNED_CONTEXT((#62759,#62761,#62762))
REPRESENTATION_CONTEXT('','3D')
);
#62694=(
GEOMETRIC_REPRESENTATION_CONTEXT(3)
GLOBAL_UNCERTAINTY_ASSIGNED_CONTEXT((#62620))
GLOBAL_UNIT_ASSIGNED_CONTEXT((#62759,#62761,#62762))
REPRESENTATION_CONTEXT('','3D')
);
#62695=(
GEOMETRIC_REPRESENTATION_CONTEXT(3)
GLOBAL_UNCERTAINTY_ASSIGNED_CONTEXT((#62621))
GLOBAL_UNIT_ASSIGNED_CONTEXT((#62759,#62761,#62762))
REPRESENTATION_CONTEXT('','3D')
);
#62696=(
GEOMETRIC_REPRESENTATION_CONTEXT(3)
GLOBAL_UNCERTAINTY_ASSIGNED_CONTEXT((#62622))
GLOBAL_UNIT_ASSIGNED_CONTEXT((#62759,#62761,#62762))
REPRESENTATION_CONTEXT('','3D')
);
#62697=(
GEOMETRIC_REPRESENTATION_CONTEXT(3)
GLOBAL_UNCERTAINTY_ASSIGNED_CONTEXT((#62623))
GLOBAL_UNIT_ASSIGNED_CONTEXT((#62759,#62761,#62762))
REPRESENTATION_CONTEXT('','3D')
);
#62698=(
GEOMETRIC_REPRESENTATION_CONTEXT(3)
GLOBAL_UNCERTAINTY_ASSIGNED_CONTEXT((#62624))
GLOBAL_UNIT_ASSIGNED_CONTEXT((#62759,#62761,#62762))
REPRESENTATION_CONTEXT('','3D')
);
#62699=(
GEOMETRIC_REPRESENTATION_CONTEXT(3)
GLOBAL_UNCERTAINTY_ASSIGNED_CONTEXT((#62625))
GLOBAL_UNIT_ASSIGNED_CONTEXT((#62759,#62761,#62762))
REPRESENTATION_CONTEXT('','3D')
);
#62700=(
GEOMETRIC_REPRESENTATION_CONTEXT(3)
GLOBAL_UNCERTAINTY_ASSIGNED_CONTEXT((#62626))
GLOBAL_UNIT_ASSIGNED_CONTEXT((#62759,#62761,#62762))
REPRESENTATION_CONTEXT('','3D')
);
#62701=(
GEOMETRIC_REPRESENTATION_CONTEXT(3)
GLOBAL_UNCERTAINTY_ASSIGNED_CONTEXT((#62627))
GLOBAL_UNIT_ASSIGNED_CONTEXT((#62759,#62761,#62762))
REPRESENTATION_CONTEXT('','3D')
);
#62702=(
GEOMETRIC_REPRESENTATION_CONTEXT(3)
GLOBAL_UNCERTAINTY_ASSIGNED_CONTEXT((#62628))
GLOBAL_UNIT_ASSIGNED_CONTEXT((#62759,#62761,#62762))
REPRESENTATION_CONTEXT('','3D')
);
#62703=(
GEOMETRIC_REPRESENTATION_CONTEXT(3)
GLOBAL_UNCERTAINTY_ASSIGNED_CONTEXT((#62629))
GLOBAL_UNIT_ASSIGNED_CONTEXT((#62759,#62761,#62762))
REPRESENTATION_CONTEXT('','3D')
);
#62704=(
GEOMETRIC_REPRESENTATION_CONTEXT(3)
GLOBAL_UNCERTAINTY_ASSIGNED_CONTEXT((#62630))
GLOBAL_UNIT_ASSIGNED_CONTEXT((#62759,#62761,#62762))
REPRESENTATION_CONTEXT('','3D')
);
#62705=(
GEOMETRIC_REPRESENTATION_CONTEXT(3)
GLOBAL_UNCERTAINTY_ASSIGNED_CONTEXT((#62631))
GLOBAL_UNIT_ASSIGNED_CONTEXT((#62759,#62761,#62762))
REPRESENTATION_CONTEXT('','3D')
);
#62706=(
GEOMETRIC_REPRESENTATION_CONTEXT(3)
GLOBAL_UNCERTAINTY_ASSIGNED_CONTEXT((#62632))
GLOBAL_UNIT_ASSIGNED_CONTEXT((#62759,#62761,#62762))
REPRESENTATION_CONTEXT('','3D')
);
#62707=(
GEOMETRIC_REPRESENTATION_CONTEXT(3)
GLOBAL_UNCERTAINTY_ASSIGNED_CONTEXT((#62633))
GLOBAL_UNIT_ASSIGNED_CONTEXT((#62759,#62761,#62762))
REPRESENTATION_CONTEXT('','3D')
);
#62708=(
GEOMETRIC_REPRESENTATION_CONTEXT(3)
GLOBAL_UNCERTAINTY_ASSIGNED_CONTEXT((#62634))
GLOBAL_UNIT_ASSIGNED_CONTEXT((#62759,#62761,#62762))
REPRESENTATION_CONTEXT('','3D')
);
#62709=(
GEOMETRIC_REPRESENTATION_CONTEXT(3)
GLOBAL_UNCERTAINTY_ASSIGNED_CONTEXT((#62635))
GLOBAL_UNIT_ASSIGNED_CONTEXT((#62759,#62761,#62762))
REPRESENTATION_CONTEXT('','3D')
);
#62710=(
GEOMETRIC_REPRESENTATION_CONTEXT(3)
GLOBAL_UNCERTAINTY_ASSIGNED_CONTEXT((#62636))
GLOBAL_UNIT_ASSIGNED_CONTEXT((#62759,#62761,#62762))
REPRESENTATION_CONTEXT('','3D')
);
#62711=(
GEOMETRIC_REPRESENTATION_CONTEXT(3)
GLOBAL_UNCERTAINTY_ASSIGNED_CONTEXT((#62637))
GLOBAL_UNIT_ASSIGNED_CONTEXT((#62759,#62761,#62762))
REPRESENTATION_CONTEXT('','3D')
);
#62712=(
GEOMETRIC_REPRESENTATION_CONTEXT(3)
GLOBAL_UNCERTAINTY_ASSIGNED_CONTEXT((#62638))
GLOBAL_UNIT_ASSIGNED_CONTEXT((#62759,#62761,#62762))
REPRESENTATION_CONTEXT('','3D')
);
#62713=(
GEOMETRIC_REPRESENTATION_CONTEXT(3)
GLOBAL_UNCERTAINTY_ASSIGNED_CONTEXT((#62639))
GLOBAL_UNIT_ASSIGNED_CONTEXT((#62759,#62761,#62762))
REPRESENTATION_CONTEXT('','3D')
);
#62714=(
GEOMETRIC_REPRESENTATION_CONTEXT(3)
GLOBAL_UNCERTAINTY_ASSIGNED_CONTEXT((#62640))
GLOBAL_UNIT_ASSIGNED_CONTEXT((#62759,#62761,#62762))
REPRESENTATION_CONTEXT('','3D')
);
#62715=(
GEOMETRIC_REPRESENTATION_CONTEXT(3)
GLOBAL_UNCERTAINTY_ASSIGNED_CONTEXT((#62641))
GLOBAL_UNIT_ASSIGNED_CONTEXT((#62759,#62761,#62762))
REPRESENTATION_CONTEXT('','3D')
);
#62716=(
GEOMETRIC_REPRESENTATION_CONTEXT(3)
GLOBAL_UNCERTAINTY_ASSIGNED_CONTEXT((#62642))
GLOBAL_UNIT_ASSIGNED_CONTEXT((#62759,#62761,#62762))
REPRESENTATION_CONTEXT('','3D')
);
#62717=(
GEOMETRIC_REPRESENTATION_CONTEXT(3)
GLOBAL_UNCERTAINTY_ASSIGNED_CONTEXT((#62643))
GLOBAL_UNIT_ASSIGNED_CONTEXT((#62759,#62761,#62762))
REPRESENTATION_CONTEXT('','3D')
);
#62718=(
GEOMETRIC_REPRESENTATION_CONTEXT(3)
GLOBAL_UNCERTAINTY_ASSIGNED_CONTEXT((#62644))
GLOBAL_UNIT_ASSIGNED_CONTEXT((#62759,#62761,#62762))
REPRESENTATION_CONTEXT('','3D')
);
#62719=(
GEOMETRIC_REPRESENTATION_CONTEXT(3)
GLOBAL_UNCERTAINTY_ASSIGNED_CONTEXT((#62645))
GLOBAL_UNIT_ASSIGNED_CONTEXT((#62759,#62761,#62762))
REPRESENTATION_CONTEXT('','3D')
);
#62720=(
GEOMETRIC_REPRESENTATION_CONTEXT(3)
GLOBAL_UNCERTAINTY_ASSIGNED_CONTEXT((#62646))
GLOBAL_UNIT_ASSIGNED_CONTEXT((#62759,#62761,#62762))
REPRESENTATION_CONTEXT('','3D')
);
#62721=(
GEOMETRIC_REPRESENTATION_CONTEXT(3)
GLOBAL_UNCERTAINTY_ASSIGNED_CONTEXT((#62647))
GLOBAL_UNIT_ASSIGNED_CONTEXT((#62759,#62761,#62762))
REPRESENTATION_CONTEXT('','3D')
);
#62722=(
GEOMETRIC_REPRESENTATION_CONTEXT(3)
GLOBAL_UNCERTAINTY_ASSIGNED_CONTEXT((#62648))
GLOBAL_UNIT_ASSIGNED_CONTEXT((#62759,#62761,#62762))
REPRESENTATION_CONTEXT('','3D')
);
#62723=(
GEOMETRIC_REPRESENTATION_CONTEXT(3)
GLOBAL_UNCERTAINTY_ASSIGNED_CONTEXT((#62649))
GLOBAL_UNIT_ASSIGNED_CONTEXT((#62759,#62761,#62762))
REPRESENTATION_CONTEXT('','3D')
);
#62724=(
GEOMETRIC_REPRESENTATION_CONTEXT(3)
GLOBAL_UNCERTAINTY_ASSIGNED_CONTEXT((#62650))
GLOBAL_UNIT_ASSIGNED_CONTEXT((#62759,#62761,#62762))
REPRESENTATION_CONTEXT('','3D')
);
#62725=(
GEOMETRIC_REPRESENTATION_CONTEXT(3)
GLOBAL_UNCERTAINTY_ASSIGNED_CONTEXT((#62651))
GLOBAL_UNIT_ASSIGNED_CONTEXT((#62759,#62761,#62762))
REPRESENTATION_CONTEXT('','3D')
);
#62726=(
GEOMETRIC_REPRESENTATION_CONTEXT(3)
GLOBAL_UNCERTAINTY_ASSIGNED_CONTEXT((#62652))
GLOBAL_UNIT_ASSIGNED_CONTEXT((#62759,#62761,#62762))
REPRESENTATION_CONTEXT('','3D')
);
#62727=(
GEOMETRIC_REPRESENTATION_CONTEXT(3)
GLOBAL_UNCERTAINTY_ASSIGNED_CONTEXT((#62653))
GLOBAL_UNIT_ASSIGNED_CONTEXT((#62759,#62761,#62762))
REPRESENTATION_CONTEXT('','3D')
);
#62728=(
GEOMETRIC_REPRESENTATION_CONTEXT(3)
GLOBAL_UNCERTAINTY_ASSIGNED_CONTEXT((#62654))
GLOBAL_UNIT_ASSIGNED_CONTEXT((#62759,#62761,#62762))
REPRESENTATION_CONTEXT('','3D')
);
#62729=(
GEOMETRIC_REPRESENTATION_CONTEXT(3)
GLOBAL_UNCERTAINTY_ASSIGNED_CONTEXT((#62655))
GLOBAL_UNIT_ASSIGNED_CONTEXT((#62759,#62761,#62762))
REPRESENTATION_CONTEXT('','3D')
);
#62730=(
GEOMETRIC_REPRESENTATION_CONTEXT(3)
GLOBAL_UNCERTAINTY_ASSIGNED_CONTEXT((#62656))
GLOBAL_UNIT_ASSIGNED_CONTEXT((#62759,#62761,#62762))
REPRESENTATION_CONTEXT('','3D')
);
#62731=(
GEOMETRIC_REPRESENTATION_CONTEXT(3)
GLOBAL_UNCERTAINTY_ASSIGNED_CONTEXT((#62657))
GLOBAL_UNIT_ASSIGNED_CONTEXT((#62759,#62761,#62762))
REPRESENTATION_CONTEXT('','3D')
);
#62732=(
GEOMETRIC_REPRESENTATION_CONTEXT(3)
GLOBAL_UNCERTAINTY_ASSIGNED_CONTEXT((#62658))
GLOBAL_UNIT_ASSIGNED_CONTEXT((#62759,#62761,#62762))
REPRESENTATION_CONTEXT('','3D')
);
#62733=(
GEOMETRIC_REPRESENTATION_CONTEXT(3)
GLOBAL_UNCERTAINTY_ASSIGNED_CONTEXT((#62659))
GLOBAL_UNIT_ASSIGNED_CONTEXT((#62759,#62761,#62762))
REPRESENTATION_CONTEXT('','3D')
);
#62734=(
GEOMETRIC_REPRESENTATION_CONTEXT(3)
GLOBAL_UNCERTAINTY_ASSIGNED_CONTEXT((#62660))
GLOBAL_UNIT_ASSIGNED_CONTEXT((#62759,#62761,#62762))
REPRESENTATION_CONTEXT('','3D')
);
#62735=(
GEOMETRIC_REPRESENTATION_CONTEXT(3)
GLOBAL_UNCERTAINTY_ASSIGNED_CONTEXT((#62661))
GLOBAL_UNIT_ASSIGNED_CONTEXT((#62759,#62761,#62762))
REPRESENTATION_CONTEXT('','3D')
);
#62736=(
GEOMETRIC_REPRESENTATION_CONTEXT(3)
GLOBAL_UNCERTAINTY_ASSIGNED_CONTEXT((#62662))
GLOBAL_UNIT_ASSIGNED_CONTEXT((#62759,#62761,#62762))
REPRESENTATION_CONTEXT('','3D')
);
#62737=(
GEOMETRIC_REPRESENTATION_CONTEXT(3)
GLOBAL_UNCERTAINTY_ASSIGNED_CONTEXT((#62663))
GLOBAL_UNIT_ASSIGNED_CONTEXT((#62759,#62761,#62762))
REPRESENTATION_CONTEXT('','3D')
);
#62738=(
GEOMETRIC_REPRESENTATION_CONTEXT(3)
GLOBAL_UNCERTAINTY_ASSIGNED_CONTEXT((#62664))
GLOBAL_UNIT_ASSIGNED_CONTEXT((#62759,#62761,#62762))
REPRESENTATION_CONTEXT('','3D')
);
#62739=(
GEOMETRIC_REPRESENTATION_CONTEXT(3)
GLOBAL_UNCERTAINTY_ASSIGNED_CONTEXT((#62665))
GLOBAL_UNIT_ASSIGNED_CONTEXT((#62759,#62761,#62762))
REPRESENTATION_CONTEXT('','3D')
);
#62740=(
GEOMETRIC_REPRESENTATION_CONTEXT(3)
GLOBAL_UNCERTAINTY_ASSIGNED_CONTEXT((#62666))
GLOBAL_UNIT_ASSIGNED_CONTEXT((#62759,#62761,#62762))
REPRESENTATION_CONTEXT('','3D')
);
#62741=(
GEOMETRIC_REPRESENTATION_CONTEXT(3)
GLOBAL_UNCERTAINTY_ASSIGNED_CONTEXT((#62667))
GLOBAL_UNIT_ASSIGNED_CONTEXT((#62759,#62761,#62762))
REPRESENTATION_CONTEXT('','3D')
);
#62742=(
GEOMETRIC_REPRESENTATION_CONTEXT(3)
GLOBAL_UNCERTAINTY_ASSIGNED_CONTEXT((#62668))
GLOBAL_UNIT_ASSIGNED_CONTEXT((#62759,#62761,#62762))
REPRESENTATION_CONTEXT('','3D')
);
#62743=(
GEOMETRIC_REPRESENTATION_CONTEXT(3)
GLOBAL_UNCERTAINTY_ASSIGNED_CONTEXT((#62669))
GLOBAL_UNIT_ASSIGNED_CONTEXT((#62759,#62761,#62762))
REPRESENTATION_CONTEXT('','3D')
);
#62744=(
GEOMETRIC_REPRESENTATION_CONTEXT(3)
GLOBAL_UNCERTAINTY_ASSIGNED_CONTEXT((#62670))
GLOBAL_UNIT_ASSIGNED_CONTEXT((#62759,#62761,#62762))
REPRESENTATION_CONTEXT('','3D')
);
#62745=(
GEOMETRIC_REPRESENTATION_CONTEXT(3)
GLOBAL_UNCERTAINTY_ASSIGNED_CONTEXT((#62671))
GLOBAL_UNIT_ASSIGNED_CONTEXT((#62759,#62761,#62762))
REPRESENTATION_CONTEXT('','3D')
);
#62746=(
GEOMETRIC_REPRESENTATION_CONTEXT(3)
GLOBAL_UNCERTAINTY_ASSIGNED_CONTEXT((#62672))
GLOBAL_UNIT_ASSIGNED_CONTEXT((#62759,#62761,#62762))
REPRESENTATION_CONTEXT('','3D')
);
#62747=(
GEOMETRIC_REPRESENTATION_CONTEXT(3)
GLOBAL_UNCERTAINTY_ASSIGNED_CONTEXT((#62673))
GLOBAL_UNIT_ASSIGNED_CONTEXT((#62759,#62761,#62762))
REPRESENTATION_CONTEXT('','3D')
);
#62748=(
GEOMETRIC_REPRESENTATION_CONTEXT(3)
GLOBAL_UNCERTAINTY_ASSIGNED_CONTEXT((#62674))
GLOBAL_UNIT_ASSIGNED_CONTEXT((#62759,#62761,#62762))
REPRESENTATION_CONTEXT('','3D')
);
#62749=(
GEOMETRIC_REPRESENTATION_CONTEXT(3)
GLOBAL_UNCERTAINTY_ASSIGNED_CONTEXT((#62675))
GLOBAL_UNIT_ASSIGNED_CONTEXT((#62759,#62761,#62762))
REPRESENTATION_CONTEXT('','3D')
);
#62750=(
GEOMETRIC_REPRESENTATION_CONTEXT(3)
GLOBAL_UNCERTAINTY_ASSIGNED_CONTEXT((#62676))
GLOBAL_UNIT_ASSIGNED_CONTEXT((#62759,#62761,#62762))
REPRESENTATION_CONTEXT('','3D')
);
#62751=(
GEOMETRIC_REPRESENTATION_CONTEXT(3)
GLOBAL_UNCERTAINTY_ASSIGNED_CONTEXT((#62677))
GLOBAL_UNIT_ASSIGNED_CONTEXT((#62759,#62761,#62762))
REPRESENTATION_CONTEXT('','3D')
);
#62752=(
GEOMETRIC_REPRESENTATION_CONTEXT(3)
GLOBAL_UNCERTAINTY_ASSIGNED_CONTEXT((#62678))
GLOBAL_UNIT_ASSIGNED_CONTEXT((#62759,#62761,#62762))
REPRESENTATION_CONTEXT('','3D')
);
#62753=(
GEOMETRIC_REPRESENTATION_CONTEXT(3)
GLOBAL_UNCERTAINTY_ASSIGNED_CONTEXT((#62679))
GLOBAL_UNIT_ASSIGNED_CONTEXT((#62759,#62761,#62762))
REPRESENTATION_CONTEXT('','3D')
);
#62754=(
GEOMETRIC_REPRESENTATION_CONTEXT(3)
GLOBAL_UNCERTAINTY_ASSIGNED_CONTEXT((#62680))
GLOBAL_UNIT_ASSIGNED_CONTEXT((#62759,#62761,#62762))
REPRESENTATION_CONTEXT('','3D')
);
#62755=(
GEOMETRIC_REPRESENTATION_CONTEXT(3)
GLOBAL_UNCERTAINTY_ASSIGNED_CONTEXT((#62681))
GLOBAL_UNIT_ASSIGNED_CONTEXT((#62759,#62761,#62762))
REPRESENTATION_CONTEXT('','3D')
);
#62756=(
GEOMETRIC_REPRESENTATION_CONTEXT(3)
GLOBAL_UNCERTAINTY_ASSIGNED_CONTEXT((#62682))
GLOBAL_UNIT_ASSIGNED_CONTEXT((#62759,#62761,#62762))
REPRESENTATION_CONTEXT('','3D')
);
#62757=(
GEOMETRIC_REPRESENTATION_CONTEXT(3)
GLOBAL_UNCERTAINTY_ASSIGNED_CONTEXT((#62683))
GLOBAL_UNIT_ASSIGNED_CONTEXT((#62759,#62761,#62762))
REPRESENTATION_CONTEXT('','3D')
);
#62758=(
GEOMETRIC_REPRESENTATION_CONTEXT(3)
GLOBAL_UNCERTAINTY_ASSIGNED_CONTEXT((#62684))
GLOBAL_UNIT_ASSIGNED_CONTEXT((#62759,#62761,#62762))
REPRESENTATION_CONTEXT('','3D')
);
#62759=(
LENGTH_UNIT()
NAMED_UNIT(*)
SI_UNIT(.CENTI.,.METRE.)
);
#62760=(
LENGTH_UNIT()
NAMED_UNIT(*)
SI_UNIT($,.METRE.)
);
#62761=(
NAMED_UNIT(*)
PLANE_ANGLE_UNIT()
SI_UNIT($,.RADIAN.)
);
#62762=(
NAMED_UNIT(*)
SI_UNIT($,.STERADIAN.)
SOLID_ANGLE_UNIT()
);
#62763=SHAPE_DEFINITION_REPRESENTATION(#62836,#63031);
#62764=SHAPE_DEFINITION_REPRESENTATION(#62837,#63032);
#62765=SHAPE_DEFINITION_REPRESENTATION(#62838,#63033);
#62766=SHAPE_DEFINITION_REPRESENTATION(#62839,#63034);
#62767=SHAPE_DEFINITION_REPRESENTATION(#62840,#63035);
#62768=SHAPE_DEFINITION_REPRESENTATION(#62841,#63036);
#62769=SHAPE_DEFINITION_REPRESENTATION(#62842,#63037);
#62770=SHAPE_DEFINITION_REPRESENTATION(#62843,#63038);
#62771=SHAPE_DEFINITION_REPRESENTATION(#62844,#63039);
#62772=SHAPE_DEFINITION_REPRESENTATION(#62845,#63040);
#62773=SHAPE_DEFINITION_REPRESENTATION(#62846,#63041);
#62774=SHAPE_DEFINITION_REPRESENTATION(#62847,#63042);
#62775=SHAPE_DEFINITION_REPRESENTATION(#62848,#63043);
#62776=SHAPE_DEFINITION_REPRESENTATION(#62849,#63044);
#62777=SHAPE_DEFINITION_REPRESENTATION(#62850,#63045);
#62778=SHAPE_DEFINITION_REPRESENTATION(#62851,#63046);
#62779=SHAPE_DEFINITION_REPRESENTATION(#62852,#63047);
#62780=SHAPE_DEFINITION_REPRESENTATION(#62853,#63048);
#62781=SHAPE_DEFINITION_REPRESENTATION(#62854,#63049);
#62782=SHAPE_DEFINITION_REPRESENTATION(#62860,#63050);
#62783=SHAPE_DEFINITION_REPRESENTATION(#62861,#63051);
#62784=SHAPE_DEFINITION_REPRESENTATION(#62862,#63052);
#62785=SHAPE_DEFINITION_REPRESENTATION(#62863,#63053);
#62786=SHAPE_DEFINITION_REPRESENTATION(#62864,#63054);
#62787=SHAPE_DEFINITION_REPRESENTATION(#62865,#63055);
#62788=SHAPE_DEFINITION_REPRESENTATION(#62871,#63056);
#62789=SHAPE_DEFINITION_REPRESENTATION(#62872,#63057);
#62790=SHAPE_DEFINITION_REPRESENTATION(#62873,#63058);
#62791=SHAPE_DEFINITION_REPRESENTATION(#62874,#63059);
#62792=SHAPE_DEFINITION_REPRESENTATION(#62875,#63060);
#62793=SHAPE_DEFINITION_REPRESENTATION(#62876,#63061);
#62794=SHAPE_DEFINITION_REPRESENTATION(#62877,#63062);
#62795=SHAPE_DEFINITION_REPRESENTATION(#62878,#63063);
#62796=SHAPE_DEFINITION_REPRESENTATION(#62879,#63064);
#62797=SHAPE_DEFINITION_REPRESENTATION(#62880,#63065);
#62798=SHAPE_DEFINITION_REPRESENTATION(#62881,#63066);
#62799=SHAPE_DEFINITION_REPRESENTATION(#62882,#63067);
#62800=SHAPE_DEFINITION_REPRESENTATION(#62883,#63068);
#62801=SHAPE_DEFINITION_REPRESENTATION(#62884,#63069);
#62802=SHAPE_DEFINITION_REPRESENTATION(#62885,#63070);
#62803=SHAPE_DEFINITION_REPRESENTATION(#62886,#63071);
#62804=SHAPE_DEFINITION_REPRESENTATION(#62887,#63072);
#62805=SHAPE_DEFINITION_REPRESENTATION(#62888,#63073);
#62806=SHAPE_DEFINITION_REPRESENTATION(#62889,#63074);
#62807=SHAPE_DEFINITION_REPRESENTATION(#62890,#63075);
#62808=SHAPE_DEFINITION_REPRESENTATION(#62891,#63076);
#62809=SHAPE_DEFINITION_REPRESENTATION(#62892,#63077);
#62810=SHAPE_DEFINITION_REPRESENTATION(#62893,#63078);
#62811=SHAPE_DEFINITION_REPRESENTATION(#62894,#63079);
#62812=SHAPE_DEFINITION_REPRESENTATION(#62895,#63080);
#62813=SHAPE_DEFINITION_REPRESENTATION(#62896,#63081);
#62814=SHAPE_DEFINITION_REPRESENTATION(#62897,#63082);
#62815=SHAPE_DEFINITION_REPRESENTATION(#62898,#63083);
#62816=SHAPE_DEFINITION_REPRESENTATION(#62899,#63084);
#62817=SHAPE_DEFINITION_REPRESENTATION(#62900,#63085);
#62818=SHAPE_DEFINITION_REPRESENTATION(#62901,#63086);
#62819=SHAPE_DEFINITION_REPRESENTATION(#62902,#63087);
#62820=SHAPE_DEFINITION_REPRESENTATION(#62903,#63088);
#62821=SHAPE_DEFINITION_REPRESENTATION(#62904,#63089);
#62822=SHAPE_DEFINITION_REPRESENTATION(#62905,#63090);
#62823=SHAPE_DEFINITION_REPRESENTATION(#62906,#63091);
#62824=SHAPE_DEFINITION_REPRESENTATION(#62907,#63092);
#62825=SHAPE_DEFINITION_REPRESENTATION(#62908,#63093);
#62826=SHAPE_DEFINITION_REPRESENTATION(#62909,#63094);
#62827=SHAPE_DEFINITION_REPRESENTATION(#62910,#63095);
#62828=SHAPE_DEFINITION_REPRESENTATION(#62911,#63096);
#62829=SHAPE_DEFINITION_REPRESENTATION(#62912,#63097);
#62830=SHAPE_DEFINITION_REPRESENTATION(#62913,#63098);
#62831=SHAPE_DEFINITION_REPRESENTATION(#62914,#63099);
#62832=SHAPE_DEFINITION_REPRESENTATION(#62915,#63100);
#62833=SHAPE_DEFINITION_REPRESENTATION(#62916,#63101);
#62834=SHAPE_DEFINITION_REPRESENTATION(#63022,#63102);
#62835=SHAPE_DEFINITION_REPRESENTATION(#63023,#63103);
#62836=PRODUCT_DEFINITION_SHAPE('',$,#63105);
#62837=PRODUCT_DEFINITION_SHAPE('',$,#63106);
#62838=PRODUCT_DEFINITION_SHAPE('',$,#63107);
#62839=PRODUCT_DEFINITION_SHAPE('',$,#63108);
#62840=PRODUCT_DEFINITION_SHAPE('',$,#63109);
#62841=PRODUCT_DEFINITION_SHAPE('',$,#63110);
#62842=PRODUCT_DEFINITION_SHAPE('',$,#63111);
#62843=PRODUCT_DEFINITION_SHAPE('',$,#63112);
#62844=PRODUCT_DEFINITION_SHAPE('',$,#63113);
#62845=PRODUCT_DEFINITION_SHAPE('',$,#63114);
#62846=PRODUCT_DEFINITION_SHAPE('',$,#63115);
#62847=PRODUCT_DEFINITION_SHAPE('',$,#63116);
#62848=PRODUCT_DEFINITION_SHAPE('',$,#63117);
#62849=PRODUCT_DEFINITION_SHAPE('',$,#63118);
#62850=PRODUCT_DEFINITION_SHAPE('',$,#63119);
#62851=PRODUCT_DEFINITION_SHAPE('',$,#63120);
#62852=PRODUCT_DEFINITION_SHAPE('',$,#63121);
#62853=PRODUCT_DEFINITION_SHAPE('',$,#63122);
#62854=PRODUCT_DEFINITION_SHAPE('',$,#63123);
#62855=PRODUCT_DEFINITION_SHAPE($,$,#737);
#62856=PRODUCT_DEFINITION_SHAPE($,$,#738);
#62857=PRODUCT_DEFINITION_SHAPE($,$,#739);
#62858=PRODUCT_DEFINITION_SHAPE($,$,#740);
#62859=PRODUCT_DEFINITION_SHAPE($,$,#741);
#62860=PRODUCT_DEFINITION_SHAPE('',$,#63124);
#62861=PRODUCT_DEFINITION_SHAPE('',$,#63125);
#62862=PRODUCT_DEFINITION_SHAPE('',$,#63126);
#62863=PRODUCT_DEFINITION_SHAPE('',$,#63127);
#62864=PRODUCT_DEFINITION_SHAPE('',$,#63128);
#62865=PRODUCT_DEFINITION_SHAPE('',$,#63129);
#62866=PRODUCT_DEFINITION_SHAPE($,$,#742);
#62867=PRODUCT_DEFINITION_SHAPE($,$,#743);
#62868=PRODUCT_DEFINITION_SHAPE($,$,#744);
#62869=PRODUCT_DEFINITION_SHAPE($,$,#745);
#62870=PRODUCT_DEFINITION_SHAPE($,$,#746);
#62871=PRODUCT_DEFINITION_SHAPE('',$,#63130);
#62872=PRODUCT_DEFINITION_SHAPE('',$,#63131);
#62873=PRODUCT_DEFINITION_SHAPE('',$,#63132);
#62874=PRODUCT_DEFINITION_SHAPE('',$,#63133);
#62875=PRODUCT_DEFINITION_SHAPE('',$,#63134);
#62876=PRODUCT_DEFINITION_SHAPE('',$,#63135);
#62877=PRODUCT_DEFINITION_SHAPE('',$,#63136);
#62878=PRODUCT_DEFINITION_SHAPE('',$,#63137);
#62879=PRODUCT_DEFINITION_SHAPE('',$,#63138);
#62880=PRODUCT_DEFINITION_SHAPE('',$,#63139);
#62881=PRODUCT_DEFINITION_SHAPE('',$,#63140);
#62882=PRODUCT_DEFINITION_SHAPE('',$,#63141);
#62883=PRODUCT_DEFINITION_SHAPE('',$,#63142);
#62884=PRODUCT_DEFINITION_SHAPE('',$,#63143);
#62885=PRODUCT_DEFINITION_SHAPE('',$,#63144);
#62886=PRODUCT_DEFINITION_SHAPE('',$,#63145);
#62887=PRODUCT_DEFINITION_SHAPE('',$,#63146);
#62888=PRODUCT_DEFINITION_SHAPE('',$,#63147);
#62889=PRODUCT_DEFINITION_SHAPE('',$,#63148);
#62890=PRODUCT_DEFINITION_SHAPE('',$,#63149);
#62891=PRODUCT_DEFINITION_SHAPE('',$,#63150);
#62892=PRODUCT_DEFINITION_SHAPE('',$,#63151);
#62893=PRODUCT_DEFINITION_SHAPE('',$,#63152);
#62894=PRODUCT_DEFINITION_SHAPE('',$,#63153);
#62895=PRODUCT_DEFINITION_SHAPE('',$,#63154);
#62896=PRODUCT_DEFINITION_SHAPE('',$,#63155);
#62897=PRODUCT_DEFINITION_SHAPE('',$,#63156);
#62898=PRODUCT_DEFINITION_SHAPE('',$,#63157);
#62899=PRODUCT_DEFINITION_SHAPE('',$,#63158);
#62900=PRODUCT_DEFINITION_SHAPE('',$,#63159);
#62901=PRODUCT_DEFINITION_SHAPE('',$,#63160);
#62902=PRODUCT_DEFINITION_SHAPE('',$,#63161);
#62903=PRODUCT_DEFINITION_SHAPE('',$,#63162);
#62904=PRODUCT_DEFINITION_SHAPE('',$,#63163);
#62905=PRODUCT_DEFINITION_SHAPE('',$,#63164);
#62906=PRODUCT_DEFINITION_SHAPE('',$,#63165);
#62907=PRODUCT_DEFINITION_SHAPE('',$,#63166);
#62908=PRODUCT_DEFINITION_SHAPE('',$,#63167);
#62909=PRODUCT_DEFINITION_SHAPE('',$,#63168);
#62910=PRODUCT_DEFINITION_SHAPE('',$,#63169);
#62911=PRODUCT_DEFINITION_SHAPE('',$,#63170);
#62912=PRODUCT_DEFINITION_SHAPE('',$,#63171);
#62913=PRODUCT_DEFINITION_SHAPE('',$,#63172);
#62914=PRODUCT_DEFINITION_SHAPE('',$,#63173);
#62915=PRODUCT_DEFINITION_SHAPE('',$,#63174);
#62916=PRODUCT_DEFINITION_SHAPE('',$,#63175);
#62917=PRODUCT_DEFINITION_SHAPE($,$,#747);
#62918=PRODUCT_DEFINITION_SHAPE($,$,#748);
#62919=PRODUCT_DEFINITION_SHAPE($,$,#749);
#62920=PRODUCT_DEFINITION_SHAPE($,$,#750);
#62921=PRODUCT_DEFINITION_SHAPE($,$,#751);
#62922=PRODUCT_DEFINITION_SHAPE($,$,#752);
#62923=PRODUCT_DEFINITION_SHAPE($,$,#753);
#62924=PRODUCT_DEFINITION_SHAPE($,$,#754);
#62925=PRODUCT_DEFINITION_SHAPE($,$,#755);
#62926=PRODUCT_DEFINITION_SHAPE($,$,#756);
#62927=PRODUCT_DEFINITION_SHAPE($,$,#757);
#62928=PRODUCT_DEFINITION_SHAPE($,$,#758);
#62929=PRODUCT_DEFINITION_SHAPE($,$,#759);
#62930=PRODUCT_DEFINITION_SHAPE($,$,#760);
#62931=PRODUCT_DEFINITION_SHAPE($,$,#761);
#62932=PRODUCT_DEFINITION_SHAPE($,$,#762);
#62933=PRODUCT_DEFINITION_SHAPE($,$,#763);
#62934=PRODUCT_DEFINITION_SHAPE($,$,#764);
#62935=PRODUCT_DEFINITION_SHAPE($,$,#765);
#62936=PRODUCT_DEFINITION_SHAPE($,$,#766);
#62937=PRODUCT_DEFINITION_SHAPE($,$,#767);
#62938=PRODUCT_DEFINITION_SHAPE($,$,#768);
#62939=PRODUCT_DEFINITION_SHAPE($,$,#769);
#62940=PRODUCT_DEFINITION_SHAPE($,$,#770);
#62941=PRODUCT_DEFINITION_SHAPE($,$,#771);
#62942=PRODUCT_DEFINITION_SHAPE($,$,#772);
#62943=PRODUCT_DEFINITION_SHAPE($,$,#773);
#62944=PRODUCT_DEFINITION_SHAPE($,$,#774);
#62945=PRODUCT_DEFINITION_SHAPE($,$,#775);
#62946=PRODUCT_DEFINITION_SHAPE($,$,#776);
#62947=PRODUCT_DEFINITION_SHAPE($,$,#777);
#62948=PRODUCT_DEFINITION_SHAPE($,$,#778);
#62949=PRODUCT_DEFINITION_SHAPE($,$,#779);
#62950=PRODUCT_DEFINITION_SHAPE($,$,#780);
#62951=PRODUCT_DEFINITION_SHAPE($,$,#781);
#62952=PRODUCT_DEFINITION_SHAPE($,$,#782);
#62953=PRODUCT_DEFINITION_SHAPE($,$,#783);
#62954=PRODUCT_DEFINITION_SHAPE($,$,#784);
#62955=PRODUCT_DEFINITION_SHAPE($,$,#785);
#62956=PRODUCT_DEFINITION_SHAPE($,$,#786);
#62957=PRODUCT_DEFINITION_SHAPE($,$,#787);
#62958=PRODUCT_DEFINITION_SHAPE($,$,#788);
#62959=PRODUCT_DEFINITION_SHAPE($,$,#789);
#62960=PRODUCT_DEFINITION_SHAPE($,$,#790);
#62961=PRODUCT_DEFINITION_SHAPE($,$,#791);
#62962=PRODUCT_DEFINITION_SHAPE($,$,#792);
#62963=PRODUCT_DEFINITION_SHAPE($,$,#793);
#62964=PRODUCT_DEFINITION_SHAPE($,$,#794);
#62965=PRODUCT_DEFINITION_SHAPE($,$,#795);
#62966=PRODUCT_DEFINITION_SHAPE($,$,#796);
#62967=PRODUCT_DEFINITION_SHAPE($,$,#797);
#62968=PRODUCT_DEFINITION_SHAPE($,$,#798);
#62969=PRODUCT_DEFINITION_SHAPE($,$,#799);
#62970=PRODUCT_DEFINITION_SHAPE($,$,#800);
#62971=PRODUCT_DEFINITION_SHAPE($,$,#801);
#62972=PRODUCT_DEFINITION_SHAPE($,$,#802);
#62973=PRODUCT_DEFINITION_SHAPE($,$,#803);
#62974=PRODUCT_DEFINITION_SHAPE($,$,#804);
#62975=PRODUCT_DEFINITION_SHAPE($,$,#805);
#62976=PRODUCT_DEFINITION_SHAPE($,$,#806);
#62977=PRODUCT_DEFINITION_SHAPE($,$,#807);
#62978=PRODUCT_DEFINITION_SHAPE($,$,#808);
#62979=PRODUCT_DEFINITION_SHAPE($,$,#809);
#62980=PRODUCT_DEFINITION_SHAPE($,$,#810);
#62981=PRODUCT_DEFINITION_SHAPE($,$,#811);
#62982=PRODUCT_DEFINITION_SHAPE($,$,#812);
#62983=PRODUCT_DEFINITION_SHAPE($,$,#813);
#62984=PRODUCT_DEFINITION_SHAPE($,$,#814);
#62985=PRODUCT_DEFINITION_SHAPE($,$,#815);
#62986=PRODUCT_DEFINITION_SHAPE($,$,#816);
#62987=PRODUCT_DEFINITION_SHAPE($,$,#817);
#62988=PRODUCT_DEFINITION_SHAPE($,$,#818);
#62989=PRODUCT_DEFINITION_SHAPE($,$,#819);
#62990=PRODUCT_DEFINITION_SHAPE($,$,#820);
#62991=PRODUCT_DEFINITION_SHAPE($,$,#821);
#62992=PRODUCT_DEFINITION_SHAPE($,$,#822);
#62993=PRODUCT_DEFINITION_SHAPE($,$,#823);
#62994=PRODUCT_DEFINITION_SHAPE($,$,#824);
#62995=PRODUCT_DEFINITION_SHAPE($,$,#825);
#62996=PRODUCT_DEFINITION_SHAPE($,$,#826);
#62997=PRODUCT_DEFINITION_SHAPE($,$,#827);
#62998=PRODUCT_DEFINITION_SHAPE($,$,#828);
#62999=PRODUCT_DEFINITION_SHAPE($,$,#829);
#63000=PRODUCT_DEFINITION_SHAPE($,$,#830);
#63001=PRODUCT_DEFINITION_SHAPE($,$,#831);
#63002=PRODUCT_DEFINITION_SHAPE($,$,#832);
#63003=PRODUCT_DEFINITION_SHAPE($,$,#833);
#63004=PRODUCT_DEFINITION_SHAPE($,$,#834);
#63005=PRODUCT_DEFINITION_SHAPE($,$,#835);
#63006=PRODUCT_DEFINITION_SHAPE($,$,#836);
#63007=PRODUCT_DEFINITION_SHAPE($,$,#837);
#63008=PRODUCT_DEFINITION_SHAPE($,$,#838);
#63009=PRODUCT_DEFINITION_SHAPE($,$,#839);
#63010=PRODUCT_DEFINITION_SHAPE($,$,#840);
#63011=PRODUCT_DEFINITION_SHAPE($,$,#841);
#63012=PRODUCT_DEFINITION_SHAPE($,$,#842);
#63013=PRODUCT_DEFINITION_SHAPE($,$,#843);
#63014=PRODUCT_DEFINITION_SHAPE($,$,#844);
#63015=PRODUCT_DEFINITION_SHAPE($,$,#845);
#63016=PRODUCT_DEFINITION_SHAPE($,$,#846);
#63017=PRODUCT_DEFINITION_SHAPE($,$,#847);
#63018=PRODUCT_DEFINITION_SHAPE($,$,#848);
#63019=PRODUCT_DEFINITION_SHAPE($,$,#849);
#63020=PRODUCT_DEFINITION_SHAPE($,$,#850);
#63021=PRODUCT_DEFINITION_SHAPE($,$,#851);
#63022=PRODUCT_DEFINITION_SHAPE('',$,#63176);
#63023=PRODUCT_DEFINITION_SHAPE('',$,#63177);
#63024=PRODUCT_DEFINITION_SHAPE($,$,#852);
#63025=PRODUCT_DEFINITION_SHAPE($,$,#853);
#63026=PRODUCT_DEFINITION_SHAPE($,$,#854);
#63027=PRODUCT_DEFINITION_SHAPE($,$,#855);
#63028=PRODUCT_DEFINITION_SHAPE($,$,#856);
#63029=PRODUCT_DEFINITION_SHAPE($,$,#857);
#63030=PRODUCT_DEFINITION_SHAPE($,$,#858);
#63031=SHAPE_REPRESENTATION('',(#17158,#18825,#18826,#18827,#18828,#18829,
#18830),#62685);
#63032=SHAPE_REPRESENTATION('',(#17159,#18709,#18710,#18711,#18712,#18713,
#18714,#18715,#18716,#18717,#18718,#18719,#18720,#18721,#18722,#18723,#18724,
#18725,#18726,#18727,#18728,#18729,#18730,#18731,#18732,#18733,#18734,#18735,
#18736,#18737,#18738,#18739,#18740,#18741,#18742,#18743,#18744,#18745,#18746,
#18747,#18748,#18749,#18750,#18751,#18752,#18753,#18754,#18755,#18756,#18757,
#18758,#18759,#18760,#18761,#18762,#18763,#18764,#18765,#18766),#62686);
#63033=SHAPE_REPRESENTATION('',(#17160),#62687);
#63034=SHAPE_REPRESENTATION('',(#17176),#62688);
#63035=SHAPE_REPRESENTATION('',(#17260),#62689);
#63036=SHAPE_REPRESENTATION('',(#17285),#62690);
#63037=SHAPE_REPRESENTATION('',(#17310),#62691);
#63038=SHAPE_REPRESENTATION('',(#17335),#62692);
#63039=SHAPE_REPRESENTATION('',(#17360),#62693);
#63040=SHAPE_REPRESENTATION('',(#17384),#62694);
#63041=SHAPE_REPRESENTATION('',(#17409),#62695);
#63042=SHAPE_REPRESENTATION('',(#17434),#62696);
#63043=SHAPE_REPRESENTATION('',(#17459),#62697);
#63044=SHAPE_REPRESENTATION('',(#17484,#17607,#17608,#17609,#17610,#17611),
#62698);
#63045=SHAPE_REPRESENTATION('',(#17485),#62699);
#63046=SHAPE_REPRESENTATION('',(#17505),#62700);
#63047=SHAPE_REPRESENTATION('',(#17525),#62701);
#63048=SHAPE_REPRESENTATION('',(#17540),#62702);
#63049=SHAPE_REPRESENTATION('',(#17590),#62703);
#63050=SHAPE_REPRESENTATION('',(#17612,#17741,#17742,#17743,#17744,#17745),
#62704);
#63051=SHAPE_REPRESENTATION('',(#17613),#62705);
#63052=SHAPE_REPRESENTATION('',(#17633),#62706);
#63053=SHAPE_REPRESENTATION('',(#17653),#62707);
#63054=SHAPE_REPRESENTATION('',(#17670),#62708);
#63055=SHAPE_REPRESENTATION('',(#17724),#62709);
#63056=SHAPE_REPRESENTATION('',(#17746),#62710);
#63057=SHAPE_REPRESENTATION('',(#17770),#62711);
#63058=SHAPE_REPRESENTATION('',(#17912),#62712);
#63059=SHAPE_REPRESENTATION('',(#17921),#62713);
#63060=SHAPE_REPRESENTATION('',(#17930),#62714);
#63061=SHAPE_REPRESENTATION('',(#17937),#62715);
#63062=SHAPE_REPRESENTATION('',(#17944),#62716);
#63063=SHAPE_REPRESENTATION('',(#17972,#18767,#18768,#18769,#18770,#18771,
#18772,#18773,#18774,#18775,#18776,#18777,#18778,#18779,#18780,#18781,#18782),
#62717);
#63064=SHAPE_REPRESENTATION('',(#17973),#62718);
#63065=SHAPE_REPRESENTATION('',(#18005),#62719);
#63066=SHAPE_REPRESENTATION('',(#18014),#62720);
#63067=SHAPE_REPRESENTATION('',(#18023),#62721);
#63068=SHAPE_REPRESENTATION('',(#18038),#62722);
#63069=SHAPE_REPRESENTATION('',(#18062),#62723);
#63070=SHAPE_REPRESENTATION('',(#18071),#62724);
#63071=SHAPE_REPRESENTATION('',(#18080),#62725);
#63072=SHAPE_REPRESENTATION('',(#18089),#62726);
#63073=SHAPE_REPRESENTATION('',(#18098),#62727);
#63074=SHAPE_REPRESENTATION('',(#18107),#62728);
#63075=SHAPE_REPRESENTATION('',(#18135,#18783,#18784,#18785,#18786,#18787,
#18788,#18789,#18790,#18791),#62729);
#63076=SHAPE_REPRESENTATION('',(#18136),#62730);
#63077=SHAPE_REPRESENTATION('',(#18161),#62731);
#63078=SHAPE_REPRESENTATION('',(#18170),#62732);
#63079=SHAPE_REPRESENTATION('',(#18179),#62733);
#63080=SHAPE_REPRESENTATION('',(#18194),#62734);
#63081=SHAPE_REPRESENTATION('',(#18203,#18792,#18793,#18794,#18795,#18796,
#18797,#18798,#18799,#18800),#62735);
#63082=SHAPE_REPRESENTATION('',(#18204),#62736);
#63083=SHAPE_REPRESENTATION('',(#18229),#62737);
#63084=SHAPE_REPRESENTATION('',(#18238),#62738);
#63085=SHAPE_REPRESENTATION('',(#18247),#62739);
#63086=SHAPE_REPRESENTATION('',(#18262),#62740);
#63087=SHAPE_REPRESENTATION('',(#18271),#62741);
#63088=SHAPE_REPRESENTATION('',(#18364),#62742);
#63089=SHAPE_REPRESENTATION('',(#18375,#18801,#18802,#18803,#18804,#18805,
#18806,#18807,#18808,#18809,#18810,#18811,#18812,#18813),#62743);
#63090=SHAPE_REPRESENTATION('',(#18376),#62744);
#63091=SHAPE_REPRESENTATION('',(#18401),#62745);
#63092=SHAPE_REPRESENTATION('',(#18410),#62746);
#63093=SHAPE_REPRESENTATION('',(#18419),#62747);
#63094=SHAPE_REPRESENTATION('',(#18434),#62748);
#63095=SHAPE_REPRESENTATION('',(#18443),#62749);
#63096=SHAPE_REPRESENTATION('',(#18452),#62750);
#63097=SHAPE_REPRESENTATION('',(#18473),#62751);
#63098=SHAPE_REPRESENTATION('',(#18482),#62752);
#63099=SHAPE_REPRESENTATION('',(#18655),#62753);
#63100=SHAPE_REPRESENTATION('',(#18666),#62754);
#63101=SHAPE_REPRESENTATION('',(#18683),#62755);
#63102=SHAPE_REPRESENTATION('',(#18814,#18824),#62756);
#63103=SHAPE_REPRESENTATION('',(#18815),#62757);
#63104=PRODUCT_DEFINITION_CONTEXT('part definition',#63325,'design');
#63105=PRODUCT_DEFINITION('PAT-052',
'PAT-052',#63178,#63104);
#63106=PRODUCT_DEFINITION('Bearing plate and dial',
'Bearing plate and dial',#63179,#63104);
#63107=PRODUCT_DEFINITION('Base','Base',#63180,#63104);
#63108=PRODUCT_DEFINITION('Bearing plate','Bearing plate',#63181,#63104);
#63109=PRODUCT_DEFINITION('mm bearing cap','mm bearing cap',#63182,#63104);
#63110=PRODUCT_DEFINITION('mm bearing cap (1)','mm bearing cap (1)',#63183,
#63104);
#63111=PRODUCT_DEFINITION('mm bearing cap (2)','mm bearing cap (2)',#63184,
#63104);
#63112=PRODUCT_DEFINITION('mm bearing cap (3)','mm bearing cap (3)',#63185,
#63104);
#63113=PRODUCT_DEFINITION('M6x18 mounting screw','M6x18 mounting screw',
#63186,#63104);
#63114=PRODUCT_DEFINITION('mm bearing cap (4)','mm bearing cap (4)',#63187,
#63104);
#63115=PRODUCT_DEFINITION('mm bearing cap (5)','mm bearing cap (5)',#63188,
#63104);
#63116=PRODUCT_DEFINITION('mm bearing cap (6)','mm bearing cap (6)',#63189,
#63104);
#63117=PRODUCT_DEFINITION('mm bearing cap (7)','mm bearing cap (7)',#63190,
#63104);
#63118=PRODUCT_DEFINITION('Sealed Ball Bearing - 12 x 32 x 10 mm',
'Sealed Ball Bearing - 12 x 32 x 10 mm',#63191,#63104);
#63119=PRODUCT_DEFINITION('Inner ring','Inner ring',#63192,#63104);
#63120=PRODUCT_DEFINITION('Outer ring','Outer ring',#63193,#63104);
#63121=PRODUCT_DEFINITION('Balls','Balls',#63194,#63104);
#63122=PRODUCT_DEFINITION('Cage','Cage',#63195,#63104);
#63123=PRODUCT_DEFINITION('Seals 2RS','Seals 2RS',#63196,#63104);
#63124=PRODUCT_DEFINITION('Sealed Ball Bearing - 20 x 47 x 14 mm',
'Sealed Ball Bearing - 20 x 47 x 14 mm',#63197,#63104);
#63125=PRODUCT_DEFINITION('Inner ring (1)','Inner ring (1)',#63198,#63104);
#63126=PRODUCT_DEFINITION('Outer ring (1)','Outer ring (1)',#63199,#63104);
#63127=PRODUCT_DEFINITION('Balls (1)','Balls (1)',#63200,#63104);
#63128=PRODUCT_DEFINITION('Cage (1)','Cage (1)',#63201,#63104);
#63129=PRODUCT_DEFINITION('Seals 2RS (1)','Seals 2RS (1)',#63202,#63104);
#63130=PRODUCT_DEFINITION('M4x10 Cap Screw','M4x10 Cap Screw',#63203,#63104);
#63131=PRODUCT_DEFINITION('Output dial','Output dial',#63204,#63104);
#63132=PRODUCT_DEFINITION('Dial post','Dial post',#63205,#63104);
#63133=PRODUCT_DEFINITION('Dial post (1)','Dial post (1)',#63206,#63104);
#63134=PRODUCT_DEFINITION('Foot strip','Foot strip',#63207,#63104);
#63135=PRODUCT_DEFINITION('Foot strip (1)','Foot strip (1)',#63208,#63104);
#63136=PRODUCT_DEFINITION('M4x30 post bolt','M4x30 post bolt',#63209,#63104);
#63137=PRODUCT_DEFINITION('Rotor 1','Rotor 1',#63210,#63104);
#63138=PRODUCT_DEFINITION('Shaft 1','Shaft 1',#63211,#63104);
#63139=PRODUCT_DEFINITION('mm gear spacer','mm gear spacer',#63212,#63104);
#63140=PRODUCT_DEFINITION('mm rear spacer','mm rear spacer',#63213,#63104);
#63141=PRODUCT_DEFINITION('mm rear collar','mm rear collar',#63214,#63104);
#63142=PRODUCT_DEFINITION('Crank arm','Crank arm',#63215,#63104);
#63143=PRODUCT_DEFINITION('Crank spacer','Crank spacer',#63216,#63104);
#63144=PRODUCT_DEFINITION('Crank spacer (1)','Crank spacer (1)',#63217,#63104);
#63145=PRODUCT_DEFINITION('Crank keeper','Crank keeper',#63218,#63104);
#63146=PRODUCT_DEFINITION('Grip sleeve','Grip sleeve',#63219,#63104);
#63147=PRODUCT_DEFINITION('Flat Washer - M6','Flat Washer - M6',#63220,
#63104);
#63148=PRODUCT_DEFINITION('M6x30 handle bolt','M6x30 handle bolt',#63221,
#63104);
#63149=PRODUCT_DEFINITION('Rotor 2','Rotor 2',#63222,#63104);
#63150=PRODUCT_DEFINITION('Shaft 2','Shaft 2',#63223,#63104);
#63151=PRODUCT_DEFINITION('mm gear spacer (1)','mm gear spacer (1)',#63224,
#63104);
#63152=PRODUCT_DEFINITION('mm rear spacer (1)','mm rear spacer (1)',#63225,
#63104);
#63153=PRODUCT_DEFINITION('mm rear collar (1)','mm rear collar (1)',#63226,
#63104);
#63154=PRODUCT_DEFINITION('mm shaft keeper','mm shaft keeper',#63227,#63104);
#63155=PRODUCT_DEFINITION('Rotor 3','Rotor 3',#63228,#63104);
#63156=PRODUCT_DEFINITION('Shaft 3','Shaft 3',#63229,#63104);
#63157=PRODUCT_DEFINITION('mm gear spacer (2)','mm gear spacer (2)',#63230,
#63104);
#63158=PRODUCT_DEFINITION('mm rear spacer (2)','mm rear spacer (2)',#63231,
#63104);
#63159=PRODUCT_DEFINITION('mm rear collar (2)','mm rear collar (2)',#63232,
#63104);
#63160=PRODUCT_DEFINITION('mm shaft keeper (1)','mm shaft keeper (1)',#63233,
#63104);
#63161=PRODUCT_DEFINITION('Spur Gear - Module 2, 20 Teeth, 12 mm Bore',
'Spur Gear - Module 2, 20 Teeth, 12 mm Bore',#63234,#63104);
#63162=PRODUCT_DEFINITION('Key 4x4x14','Key 4x4x14',#63235,#63104);
#63163=PRODUCT_DEFINITION('Rotor 4','Rotor 4',#63236,#63104);
#63164=PRODUCT_DEFINITION('Shaft 4','Shaft 4',#63237,#63104);
#63165=PRODUCT_DEFINITION('mm gear spacer (3)','mm gear spacer (3)',#63238,
#63104);
#63166=PRODUCT_DEFINITION('mm rear spacer (3)','mm rear spacer (3)',#63239,
#63104);
#63167=PRODUCT_DEFINITION('mm rear collar (3)','mm rear collar (3)',#63240,
#63104);
#63168=PRODUCT_DEFINITION('Dial rear spacer','Dial rear spacer',#63241,
#63104);
#63169=PRODUCT_DEFINITION('Dial front spacer','Dial front spacer',#63242,
#63104);
#63170=PRODUCT_DEFINITION('Pointer','Pointer',#63243,#63104);
#63171=PRODUCT_DEFINITION('Output keeper','Output keeper',#63244,#63104);
#63172=PRODUCT_DEFINITION('Spur Gear - Module 2, 40 Teeth, 20 mm Bore',
'Spur Gear - Module 2, 40 Teeth, 20 mm Bore',#63245,#63104);
#63173=PRODUCT_DEFINITION('Key 6x6x20','Key 6x6x20',#63246,#63104);
#63174=PRODUCT_DEFINITION('Socket Set Screw - M5x8',
'Socket Set Screw - M5x8',#63247,#63104);
#63175=PRODUCT_DEFINITION('Cap Screw - M4x16','Cap Screw - M4x16',#63248,
#63104);
#63176=PRODUCT_DEFINITION('Revolving grip (1)','Revolving grip (1)',#63249,
#63104);
#63177=PRODUCT_DEFINITION('Revolving grip','Revolving grip',#63250,#63104);
#63178=PRODUCT_DEFINITION_FORMATION('',$,#63327);
#63179=PRODUCT_DEFINITION_FORMATION('',$,#63328);
#63180=PRODUCT_DEFINITION_FORMATION('',$,#63329);
#63181=PRODUCT_DEFINITION_FORMATION('',$,#63330);
#63182=PRODUCT_DEFINITION_FORMATION('',$,#63331);
#63183=PRODUCT_DEFINITION_FORMATION('',$,#63332);
#63184=PRODUCT_DEFINITION_FORMATION('',$,#63333);
#63185=PRODUCT_DEFINITION_FORMATION('',$,#63334);
#63186=PRODUCT_DEFINITION_FORMATION('',$,#63335);
#63187=PRODUCT_DEFINITION_FORMATION('',$,#63336);
#63188=PRODUCT_DEFINITION_FORMATION('',$,#63337);
#63189=PRODUCT_DEFINITION_FORMATION('',$,#63338);
#63190=PRODUCT_DEFINITION_FORMATION('',$,#63339);
#63191=PRODUCT_DEFINITION_FORMATION('',$,#63340);
#63192=PRODUCT_DEFINITION_FORMATION('',$,#63341);
#63193=PRODUCT_DEFINITION_FORMATION('',$,#63342);
#63194=PRODUCT_DEFINITION_FORMATION('',$,#63343);
#63195=PRODUCT_DEFINITION_FORMATION('',$,#63344);
#63196=PRODUCT_DEFINITION_FORMATION('',$,#63345);
#63197=PRODUCT_DEFINITION_FORMATION('',$,#63346);
#63198=PRODUCT_DEFINITION_FORMATION('',$,#63347);
#63199=PRODUCT_DEFINITION_FORMATION('',$,#63348);
#63200=PRODUCT_DEFINITION_FORMATION('',$,#63349);
#63201=PRODUCT_DEFINITION_FORMATION('',$,#63350);
#63202=PRODUCT_DEFINITION_FORMATION('',$,#63351);
#63203=PRODUCT_DEFINITION_FORMATION('',$,#63352);
#63204=PRODUCT_DEFINITION_FORMATION('',$,#63353);
#63205=PRODUCT_DEFINITION_FORMATION('',$,#63354);
#63206=PRODUCT_DEFINITION_FORMATION('',$,#63355);
#63207=PRODUCT_DEFINITION_FORMATION('',$,#63356);
#63208=PRODUCT_DEFINITION_FORMATION('',$,#63357);
#63209=PRODUCT_DEFINITION_FORMATION('',$,#63358);
#63210=PRODUCT_DEFINITION_FORMATION('',$,#63359);
#63211=PRODUCT_DEFINITION_FORMATION('',$,#63360);
#63212=PRODUCT_DEFINITION_FORMATION('',$,#63361);
#63213=PRODUCT_DEFINITION_FORMATION('',$,#63362);
#63214=PRODUCT_DEFINITION_FORMATION('',$,#63363);
#63215=PRODUCT_DEFINITION_FORMATION('',$,#63364);
#63216=PRODUCT_DEFINITION_FORMATION('',$,#63365);
#63217=PRODUCT_DEFINITION_FORMATION('',$,#63366);
#63218=PRODUCT_DEFINITION_FORMATION('',$,#63367);
#63219=PRODUCT_DEFINITION_FORMATION('',$,#63368);
#63220=PRODUCT_DEFINITION_FORMATION('',$,#63369);
#63221=PRODUCT_DEFINITION_FORMATION('',$,#63370);
#63222=PRODUCT_DEFINITION_FORMATION('',$,#63371);
#63223=PRODUCT_DEFINITION_FORMATION('',$,#63372);
#63224=PRODUCT_DEFINITION_FORMATION('',$,#63373);
#63225=PRODUCT_DEFINITION_FORMATION('',$,#63374);
#63226=PRODUCT_DEFINITION_FORMATION('',$,#63375);
#63227=PRODUCT_DEFINITION_FORMATION('',$,#63376);
#63228=PRODUCT_DEFINITION_FORMATION('',$,#63377);
#63229=PRODUCT_DEFINITION_FORMATION('',$,#63378);
#63230=PRODUCT_DEFINITION_FORMATION('',$,#63379);
#63231=PRODUCT_DEFINITION_FORMATION('',$,#63380);
#63232=PRODUCT_DEFINITION_FORMATION('',$,#63381);
#63233=PRODUCT_DEFINITION_FORMATION('',$,#63382);
#63234=PRODUCT_DEFINITION_FORMATION('',$,#63383);
#63235=PRODUCT_DEFINITION_FORMATION('',$,#63384);
#63236=PRODUCT_DEFINITION_FORMATION('',$,#63385);
#63237=PRODUCT_DEFINITION_FORMATION('',$,#63386);
#63238=PRODUCT_DEFINITION_FORMATION('',$,#63387);
#63239=PRODUCT_DEFINITION_FORMATION('',$,#63388);
#63240=PRODUCT_DEFINITION_FORMATION('',$,#63389);
#63241=PRODUCT_DEFINITION_FORMATION('',$,#63390);
#63242=PRODUCT_DEFINITION_FORMATION('',$,#63391);
#63243=PRODUCT_DEFINITION_FORMATION('',$,#63392);
#63244=PRODUCT_DEFINITION_FORMATION('',$,#63393);
#63245=PRODUCT_DEFINITION_FORMATION('',$,#63394);
#63246=PRODUCT_DEFINITION_FORMATION('',$,#63395);
#63247=PRODUCT_DEFINITION_FORMATION('',$,#63396);
#63248=PRODUCT_DEFINITION_FORMATION('',$,#63397);
#63249=PRODUCT_DEFINITION_FORMATION('',$,#63398);
#63250=PRODUCT_DEFINITION_FORMATION('',$,#63399);
#63251=PRODUCT_RELATED_PRODUCT_CATEGORY('PAT-052','PAT-052',(#63327));
#63252=PRODUCT_RELATED_PRODUCT_CATEGORY('Bearing plate and dial',
'Bearing plate and dial',(#63328));
#63253=PRODUCT_RELATED_PRODUCT_CATEGORY('Base','Base',(#63329));
#63254=PRODUCT_RELATED_PRODUCT_CATEGORY('Bearing plate','Bearing plate',
(#63330));
#63255=PRODUCT_RELATED_PRODUCT_CATEGORY('mm bearing cap',
'mm bearing cap',(#63331));
#63256=PRODUCT_RELATED_PRODUCT_CATEGORY('mm bearing cap (1)',
'mm bearing cap (1)',(#63332));
#63257=PRODUCT_RELATED_PRODUCT_CATEGORY('mm bearing cap (2)',
'mm bearing cap (2)',(#63333));
#63258=PRODUCT_RELATED_PRODUCT_CATEGORY('mm bearing cap (3)',
'mm bearing cap (3)',(#63334));
#63259=PRODUCT_RELATED_PRODUCT_CATEGORY('M6x18 mounting screw',
'M6x18 mounting screw',(#63335));
#63260=PRODUCT_RELATED_PRODUCT_CATEGORY('mm bearing cap (4)',
'mm bearing cap (4)',(#63336));
#63261=PRODUCT_RELATED_PRODUCT_CATEGORY('mm bearing cap (5)',
'mm bearing cap (5)',(#63337));
#63262=PRODUCT_RELATED_PRODUCT_CATEGORY('mm bearing cap (6)',
'mm bearing cap (6)',(#63338));
#63263=PRODUCT_RELATED_PRODUCT_CATEGORY('mm bearing cap (7)',
'mm bearing cap (7)',(#63339));
#63264=PRODUCT_RELATED_PRODUCT_CATEGORY(
'Sealed Ball Bearing - 12 x 32 x 10 mm',
'Sealed Ball Bearing - 12 x 32 x 10 mm',(#63340));
#63265=PRODUCT_RELATED_PRODUCT_CATEGORY('Inner ring','Inner ring',(#63341));
#63266=PRODUCT_RELATED_PRODUCT_CATEGORY('Outer ring','Outer ring',(#63342));
#63267=PRODUCT_RELATED_PRODUCT_CATEGORY('Balls','Balls',(#63343));
#63268=PRODUCT_RELATED_PRODUCT_CATEGORY('Cage','Cage',(#63344));
#63269=PRODUCT_RELATED_PRODUCT_CATEGORY('Seals 2RS','Seals 2RS',(#63345));
#63270=PRODUCT_RELATED_PRODUCT_CATEGORY(
'Sealed Ball Bearing - 20 x 47 x 14 mm',
'Sealed Ball Bearing - 20 x 47 x 14 mm',(#63346));
#63271=PRODUCT_RELATED_PRODUCT_CATEGORY('Inner ring (1)',
'Inner ring (1)',(#63347));
#63272=PRODUCT_RELATED_PRODUCT_CATEGORY('Outer ring (1)',
'Outer ring (1)',(#63348));
#63273=PRODUCT_RELATED_PRODUCT_CATEGORY('Balls (1)','Balls (1)',(#63349));
#63274=PRODUCT_RELATED_PRODUCT_CATEGORY('Cage (1)','Cage (1)',(#63350));
#63275=PRODUCT_RELATED_PRODUCT_CATEGORY('Seals 2RS (1)','Seals 2RS (1)',
(#63351));
#63276=PRODUCT_RELATED_PRODUCT_CATEGORY('M4x10 Cap Screw',
'M4x10 Cap Screw',(#63352));
#63277=PRODUCT_RELATED_PRODUCT_CATEGORY('Output dial','Output dial',(#63353));
#63278=PRODUCT_RELATED_PRODUCT_CATEGORY('Dial post','Dial post',(#63354));
#63279=PRODUCT_RELATED_PRODUCT_CATEGORY('Dial post (1)','Dial post (1)',
(#63355));
#63280=PRODUCT_RELATED_PRODUCT_CATEGORY('Foot strip','Foot strip',(#63356));
#63281=PRODUCT_RELATED_PRODUCT_CATEGORY('Foot strip (1)',
'Foot strip (1)',(#63357));
#63282=PRODUCT_RELATED_PRODUCT_CATEGORY('M4x30 post bolt',
'M4x30 post bolt',(#63358));
#63283=PRODUCT_RELATED_PRODUCT_CATEGORY('Rotor 1','Rotor 1',(#63359));
#63284=PRODUCT_RELATED_PRODUCT_CATEGORY('Shaft 1','Shaft 1',(#63360));
#63285=PRODUCT_RELATED_PRODUCT_CATEGORY('mm gear spacer',
'mm gear spacer',(#63361));
#63286=PRODUCT_RELATED_PRODUCT_CATEGORY('mm rear spacer',
'mm rear spacer',(#63362));
#63287=PRODUCT_RELATED_PRODUCT_CATEGORY('mm rear collar',
'mm rear collar',(#63363));
#63288=PRODUCT_RELATED_PRODUCT_CATEGORY('Crank arm','Crank arm',(#63364));
#63289=PRODUCT_RELATED_PRODUCT_CATEGORY('Crank spacer','Crank spacer',(#63365));
#63290=PRODUCT_RELATED_PRODUCT_CATEGORY('Crank spacer (1)',
'Crank spacer (1)',(#63366));
#63291=PRODUCT_RELATED_PRODUCT_CATEGORY('Crank keeper','Crank keeper',(#63367));
#63292=PRODUCT_RELATED_PRODUCT_CATEGORY('Grip sleeve','Grip sleeve',(#63368));
#63293=PRODUCT_RELATED_PRODUCT_CATEGORY('Flat Washer - M6',
'Flat Washer - M6',(#63369));
#63294=PRODUCT_RELATED_PRODUCT_CATEGORY('M6x30 handle bolt',
'M6x30 handle bolt',(#63370));
#63295=PRODUCT_RELATED_PRODUCT_CATEGORY('Rotor 2','Rotor 2',(#63371));
#63296=PRODUCT_RELATED_PRODUCT_CATEGORY('Shaft 2','Shaft 2',(#63372));
#63297=PRODUCT_RELATED_PRODUCT_CATEGORY('mm gear spacer (1)',
'mm gear spacer (1)',(#63373));
#63298=PRODUCT_RELATED_PRODUCT_CATEGORY('mm rear spacer (1)',
'mm rear spacer (1)',(#63374));
#63299=PRODUCT_RELATED_PRODUCT_CATEGORY('mm rear collar (1)',
'mm rear collar (1)',(#63375));
#63300=PRODUCT_RELATED_PRODUCT_CATEGORY('mm shaft keeper',
'mm shaft keeper',(#63376));
#63301=PRODUCT_RELATED_PRODUCT_CATEGORY('Rotor 3','Rotor 3',(#63377));
#63302=PRODUCT_RELATED_PRODUCT_CATEGORY('Shaft 3','Shaft 3',(#63378));
#63303=PRODUCT_RELATED_PRODUCT_CATEGORY('mm gear spacer (2)',
'mm gear spacer (2)',(#63379));
#63304=PRODUCT_RELATED_PRODUCT_CATEGORY('mm rear spacer (2)',
'mm rear spacer (2)',(#63380));
#63305=PRODUCT_RELATED_PRODUCT_CATEGORY('mm rear collar (2)',
'mm rear collar (2)',(#63381));
#63306=PRODUCT_RELATED_PRODUCT_CATEGORY('mm shaft keeper (1)',
'mm shaft keeper (1)',(#63382));
#63307=PRODUCT_RELATED_PRODUCT_CATEGORY(
'Spur Gear - Module 2, 20 Teeth, 12 mm Bore',
'Spur Gear - Module 2, 20 Teeth, 12 mm Bore',(#63383));
#63308=PRODUCT_RELATED_PRODUCT_CATEGORY('Key 4x4x14','Key 4x4x14',(#63384));
#63309=PRODUCT_RELATED_PRODUCT_CATEGORY('Rotor 4','Rotor 4',(#63385));
#63310=PRODUCT_RELATED_PRODUCT_CATEGORY('Shaft 4','Shaft 4',(#63386));
#63311=PRODUCT_RELATED_PRODUCT_CATEGORY('mm gear spacer (3)',
'mm gear spacer (3)',(#63387));
#63312=PRODUCT_RELATED_PRODUCT_CATEGORY('mm rear spacer (3)',
'mm rear spacer (3)',(#63388));
#63313=PRODUCT_RELATED_PRODUCT_CATEGORY('mm rear collar (3)',
'mm rear collar (3)',(#63389));
#63314=PRODUCT_RELATED_PRODUCT_CATEGORY('Dial rear spacer',
'Dial rear spacer',(#63390));
#63315=PRODUCT_RELATED_PRODUCT_CATEGORY('Dial front spacer',
'Dial front spacer',(#63391));
#63316=PRODUCT_RELATED_PRODUCT_CATEGORY('Pointer','Pointer',(#63392));
#63317=PRODUCT_RELATED_PRODUCT_CATEGORY('Output keeper','Output keeper',
(#63393));
#63318=PRODUCT_RELATED_PRODUCT_CATEGORY(
'Spur Gear - Module 2, 40 Teeth, 20 mm Bore',
'Spur Gear - Module 2, 40 Teeth, 20 mm Bore',(#63394));
#63319=PRODUCT_RELATED_PRODUCT_CATEGORY('Key 6x6x20','Key 6x6x20',(#63395));
#63320=PRODUCT_RELATED_PRODUCT_CATEGORY('Socket Set Screw - M5x8',
'Socket Set Screw - M5x8',(#63396));
#63321=PRODUCT_RELATED_PRODUCT_CATEGORY('Cap Screw - M4x16',
'Cap Screw - M4x16',(#63397));
#63322=PRODUCT_RELATED_PRODUCT_CATEGORY('Revolving grip (1)',
'Revolving grip (1)',(#63398));
#63323=PRODUCT_RELATED_PRODUCT_CATEGORY('Revolving grip',
'Revolving grip',(#63399));
#63324=APPLICATION_PROTOCOL_DEFINITION('international standard',
'automotive_design',2009,#63325);
#63325=APPLICATION_CONTEXT(
'Core Data for Automotive Mechanical Design Process');
#63326=PRODUCT_CONTEXT('part definition',#63325,'mechanical');
#63327=PRODUCT('PAT-052','PAT-052',
'PAT-052',(#63326));
#63328=PRODUCT('Bearing plate and dial','Bearing plate and dial',
'Bearing plate and dial',(#63326));
#63329=PRODUCT('Base','Base','Base',(#63326));
#63330=PRODUCT('Bearing plate','Bearing plate','Bearing plate',(#63326));
#63331=PRODUCT('mm bearing cap','mm bearing cap','mm bearing cap',(#63326));
#63332=PRODUCT('mm bearing cap (1)','mm bearing cap (1)','mm bearing cap (1)',
(#63326));
#63333=PRODUCT('mm bearing cap (2)','mm bearing cap (2)','mm bearing cap (2)',
(#63326));
#63334=PRODUCT('mm bearing cap (3)','mm bearing cap (3)','mm bearing cap (3)',
(#63326));
#63335=PRODUCT('M6x18 mounting screw','M6x18 mounting screw',
'M6x18 mounting screw',(#63326));
#63336=PRODUCT('mm bearing cap (4)','mm bearing cap (4)','mm bearing cap (4)',
(#63326));
#63337=PRODUCT('mm bearing cap (5)','mm bearing cap (5)','mm bearing cap (5)',
(#63326));
#63338=PRODUCT('mm bearing cap (6)','mm bearing cap (6)','mm bearing cap (6)',
(#63326));
#63339=PRODUCT('mm bearing cap (7)','mm bearing cap (7)','mm bearing cap (7)',
(#63326));
#63340=PRODUCT('Sealed Ball Bearing - 12 x 32 x 10 mm',
'Sealed Ball Bearing - 12 x 32 x 10 mm',
'Sealed Ball Bearing - 12 x 32 x 10 mm',(#63326));
#63341=PRODUCT('Inner ring','Inner ring','Inner ring',(#63326));
#63342=PRODUCT('Outer ring','Outer ring','Outer ring',(#63326));
#63343=PRODUCT('Balls','Balls','Balls',(#63326));
#63344=PRODUCT('Cage','Cage','Cage',(#63326));
#63345=PRODUCT('Seals 2RS','Seals 2RS','Seals 2RS',(#63326));
#63346=PRODUCT('Sealed Ball Bearing - 20 x 47 x 14 mm',
'Sealed Ball Bearing - 20 x 47 x 14 mm',
'Sealed Ball Bearing - 20 x 47 x 14 mm',(#63326));
#63347=PRODUCT('Inner ring (1)','Inner ring (1)','Inner ring (1)',(#63326));
#63348=PRODUCT('Outer ring (1)','Outer ring (1)','Outer ring (1)',(#63326));
#63349=PRODUCT('Balls (1)','Balls (1)','Balls (1)',(#63326));
#63350=PRODUCT('Cage (1)','Cage (1)','Cage (1)',(#63326));
#63351=PRODUCT('Seals 2RS (1)','Seals 2RS (1)','Seals 2RS (1)',(#63326));
#63352=PRODUCT('M4x10 Cap Screw','M4x10 Cap Screw','M4x10 Cap Screw',(#63326));
#63353=PRODUCT('Output dial','Output dial','Output dial',(#63326));
#63354=PRODUCT('Dial post','Dial post','Dial post',(#63326));
#63355=PRODUCT('Dial post (1)','Dial post (1)','Dial post (1)',(#63326));
#63356=PRODUCT('Foot strip','Foot strip','Foot strip',(#63326));
#63357=PRODUCT('Foot strip (1)','Foot strip (1)','Foot strip (1)',(#63326));
#63358=PRODUCT('M4x30 post bolt','M4x30 post bolt','M4x30 post bolt',(#63326));
#63359=PRODUCT('Rotor 1','Rotor 1','Rotor 1',(#63326));
#63360=PRODUCT('Shaft 1','Shaft 1','Shaft 1',(#63326));
#63361=PRODUCT('mm gear spacer','mm gear spacer','mm gear spacer',(#63326));
#63362=PRODUCT('mm rear spacer','mm rear spacer','mm rear spacer',(#63326));
#63363=PRODUCT('mm rear collar','mm rear collar','mm rear collar',(#63326));
#63364=PRODUCT('Crank arm','Crank arm','Crank arm',(#63326));
#63365=PRODUCT('Crank spacer','Crank spacer','Crank spacer',(#63326));
#63366=PRODUCT('Crank spacer (1)','Crank spacer (1)','Crank spacer (1)',(#63326));
#63367=PRODUCT('Crank keeper','Crank keeper','Crank keeper',(#63326));
#63368=PRODUCT('Grip sleeve','Grip sleeve','Grip sleeve',(#63326));
#63369=PRODUCT('Flat Washer - M6','Flat Washer - M6','Flat Washer - M6',
(#63326));
#63370=PRODUCT('M6x30 handle bolt','M6x30 handle bolt',
'M6x30 handle bolt',(#63326));
#63371=PRODUCT('Rotor 2','Rotor 2','Rotor 2',(#63326));
#63372=PRODUCT('Shaft 2','Shaft 2','Shaft 2',(#63326));
#63373=PRODUCT('mm gear spacer (1)','mm gear spacer (1)','mm gear spacer (1)',
(#63326));
#63374=PRODUCT('mm rear spacer (1)','mm rear spacer (1)','mm rear spacer (1)',
(#63326));
#63375=PRODUCT('mm rear collar (1)','mm rear collar (1)','mm rear collar (1)',
(#63326));
#63376=PRODUCT('mm shaft keeper','mm shaft keeper','mm shaft keeper',(#63326));
#63377=PRODUCT('Rotor 3','Rotor 3','Rotor 3',(#63326));
#63378=PRODUCT('Shaft 3','Shaft 3','Shaft 3',(#63326));
#63379=PRODUCT('mm gear spacer (2)','mm gear spacer (2)','mm gear spacer (2)',
(#63326));
#63380=PRODUCT('mm rear spacer (2)','mm rear spacer (2)','mm rear spacer (2)',
(#63326));
#63381=PRODUCT('mm rear collar (2)','mm rear collar (2)','mm rear collar (2)',
(#63326));
#63382=PRODUCT('mm shaft keeper (1)','mm shaft keeper (1)',
'mm shaft keeper (1)',(#63326));
#63383=PRODUCT('Spur Gear - Module 2, 20 Teeth, 12 mm Bore',
'Spur Gear - Module 2, 20 Teeth, 12 mm Bore',
'Spur Gear - Module 2, 20 Teeth, 12 mm Bore',(#63326));
#63384=PRODUCT('Key 4x4x14','Key 4x4x14','Key 4x4x14',(#63326));
#63385=PRODUCT('Rotor 4','Rotor 4','Rotor 4',(#63326));
#63386=PRODUCT('Shaft 4','Shaft 4','Shaft 4',(#63326));
#63387=PRODUCT('mm gear spacer (3)','mm gear spacer (3)','mm gear spacer (3)',
(#63326));
#63388=PRODUCT('mm rear spacer (3)','mm rear spacer (3)','mm rear spacer (3)',
(#63326));
#63389=PRODUCT('mm rear collar (3)','mm rear collar (3)','mm rear collar (3)',
(#63326));
#63390=PRODUCT('Dial rear spacer','Dial rear spacer','Dial rear spacer',
(#63326));
#63391=PRODUCT('Dial front spacer','Dial front spacer',
'Dial front spacer',(#63326));
#63392=PRODUCT('Pointer','Pointer','Pointer',(#63326));
#63393=PRODUCT('Output keeper','Output keeper','Output keeper',(#63326));
#63394=PRODUCT('Spur Gear - Module 2, 40 Teeth, 20 mm Bore',
'Spur Gear - Module 2, 40 Teeth, 20 mm Bore',
'Spur Gear - Module 2, 40 Teeth, 20 mm Bore',(#63326));
#63395=PRODUCT('Key 6x6x20','Key 6x6x20','Key 6x6x20',(#63326));
#63396=PRODUCT('Socket Set Screw - M5x8','Socket Set Screw - M5x8',
'Socket Set Screw - M5x8',(#63326));
#63397=PRODUCT('Cap Screw - M4x16','Cap Screw - M4x16',
'Cap Screw - M4x16',(#63326));
#63398=PRODUCT('Revolving grip (1)','Revolving grip (1)','Revolving grip (1)',(#63326));
#63399=PRODUCT('Revolving grip','Revolving grip','Revolving grip',(#63326));
#63400=PRESENTATION_STYLE_ASSIGNMENT((#63405));
#63401=PRESENTATION_STYLE_ASSIGNMENT((#63406));
#63402=PRESENTATION_STYLE_ASSIGNMENT((#63407));
#63403=PRESENTATION_STYLE_ASSIGNMENT((#63408));
#63404=PRESENTATION_STYLE_ASSIGNMENT((#63409));
#63405=SURFACE_STYLE_USAGE(.BOTH.,#63410);
#63406=SURFACE_STYLE_USAGE(.BOTH.,#63411);
#63407=SURFACE_STYLE_USAGE(.BOTH.,#63412);
#63408=SURFACE_STYLE_USAGE(.BOTH.,#63413);
#63409=SURFACE_STYLE_USAGE(.BOTH.,#63414);
#63410=SURFACE_SIDE_STYLE('',(#63415));
#63411=SURFACE_SIDE_STYLE('',(#63416));
#63412=SURFACE_SIDE_STYLE('',(#63417));
#63413=SURFACE_SIDE_STYLE('',(#63418));
#63414=SURFACE_SIDE_STYLE('',(#63419));
#63415=SURFACE_STYLE_FILL_AREA(#63420);
#63416=SURFACE_STYLE_FILL_AREA(#63421);
#63417=SURFACE_STYLE_FILL_AREA(#63422);
#63418=SURFACE_STYLE_FILL_AREA(#63423);
#63419=SURFACE_STYLE_FILL_AREA(#63424);
#63420=FILL_AREA_STYLE('Steel - Satin',(#63425));
#63421=FILL_AREA_STYLE('CAD Library Painted - Deep blue',(#63426));
#63422=FILL_AREA_STYLE('CAD Library Painted - Steel gray',(#63427));
#63423=FILL_AREA_STYLE('CAD Library Painted - Graphite',(#63428));
#63424=FILL_AREA_STYLE('CAD Library Painted - Engineering blue',(#63429));
#63425=FILL_AREA_STYLE_COLOUR('Steel - Satin',#63430);
#63426=FILL_AREA_STYLE_COLOUR('CAD Library Painted - Deep blue',#63431);
#63427=FILL_AREA_STYLE_COLOUR('CAD Library Painted - Steel gray',#63432);
#63428=FILL_AREA_STYLE_COLOUR('CAD Library Painted - Graphite',#63433);
#63429=FILL_AREA_STYLE_COLOUR('CAD Library Painted - Engineering blue',
#63434);
#63430=COLOUR_RGB('Steel - Satin',0.627450980392157,0.627450980392157,0.627450980392157);
#63431=COLOUR_RGB('CAD Library Painted - Deep blue',0.0784313725490196,
0.203921568627451,0.349019607843137);
#63432=COLOUR_RGB('CAD Library Painted - Steel gray',0.592156862745098,
0.631372549019608,0.67843137254902);
#63433=COLOUR_RGB('CAD Library Painted - Graphite',0.168627450980392,0.192156862745098,
0.231372549019608);
#63434=COLOUR_RGB('CAD Library Painted - Engineering blue',0.12156862745098,
0.356862745098039,0.6);
#63435=COLOUR_RGB('Dark Blue',0.08,0.2,0.34);
#63436=FILL_AREA_STYLE_COLOUR('',#63435);
#63437=FILL_AREA_STYLE('',(#63436));
#63438=SURFACE_STYLE_FILL_AREA(#63437);
#63439=SURFACE_SIDE_STYLE('',(#63438));
#63440=SURFACE_STYLE_USAGE(.BOTH.,#63439);
#63441=PRESENTATION_STYLE_ASSIGNMENT((#63440));
#63442=COLOUR_RGB('Light Blue',0.38,0.62,0.78);
#63443=FILL_AREA_STYLE_COLOUR('',#63442);
#63444=FILL_AREA_STYLE('',(#63443));
#63445=SURFACE_STYLE_FILL_AREA(#63444);
#63446=SURFACE_SIDE_STYLE('',(#63445));
#63447=SURFACE_STYLE_USAGE(.BOTH.,#63446);
#63448=PRESENTATION_STYLE_ASSIGNMENT((#63447));
#63449=COLOUR_RGB('Sky Blue',0.24,0.69,0.87);
#63450=FILL_AREA_STYLE_COLOUR('',#63449);
#63451=FILL_AREA_STYLE('',(#63450));
#63452=SURFACE_STYLE_FILL_AREA(#63451);
#63453=SURFACE_SIDE_STYLE('',(#63452));
#63454=SURFACE_STYLE_USAGE(.BOTH.,#63453);
#63455=PRESENTATION_STYLE_ASSIGNMENT((#63454));
#63456=COLOUR_RGB('Grey',0.48,0.52,0.57);
#63457=FILL_AREA_STYLE_COLOUR('',#63456);
#63458=FILL_AREA_STYLE('',(#63457));
#63459=SURFACE_STYLE_FILL_AREA(#63458);
#63460=SURFACE_SIDE_STYLE('',(#63459));
#63461=SURFACE_STYLE_USAGE(.BOTH.,#63460);
#63462=PRESENTATION_STYLE_ASSIGNMENT((#63461));
#63463=COLOUR_RGB('Black',0.12,0.14,0.17);
#63464=FILL_AREA_STYLE_COLOUR('',#63463);
#63465=FILL_AREA_STYLE('',(#63464));
#63466=SURFACE_STYLE_FILL_AREA(#63465);
#63467=SURFACE_SIDE_STYLE('',(#63466));
#63468=SURFACE_STYLE_USAGE(.BOTH.,#63467);
#63469=PRESENTATION_STYLE_ASSIGNMENT((#63468));
#63470=COLOUR_RGB('Off White',0.89,0.88,0.83);
#63471=FILL_AREA_STYLE_COLOUR('',#63470);
#63472=FILL_AREA_STYLE('',(#63471));
#63473=SURFACE_STYLE_FILL_AREA(#63472);
#63474=SURFACE_SIDE_STYLE('',(#63473));
#63475=SURFACE_STYLE_USAGE(.BOTH.,#63474);
#63476=PRESENTATION_STYLE_ASSIGNMENT((#63475));
ENDSEC;
END-ISO-10303-21;
